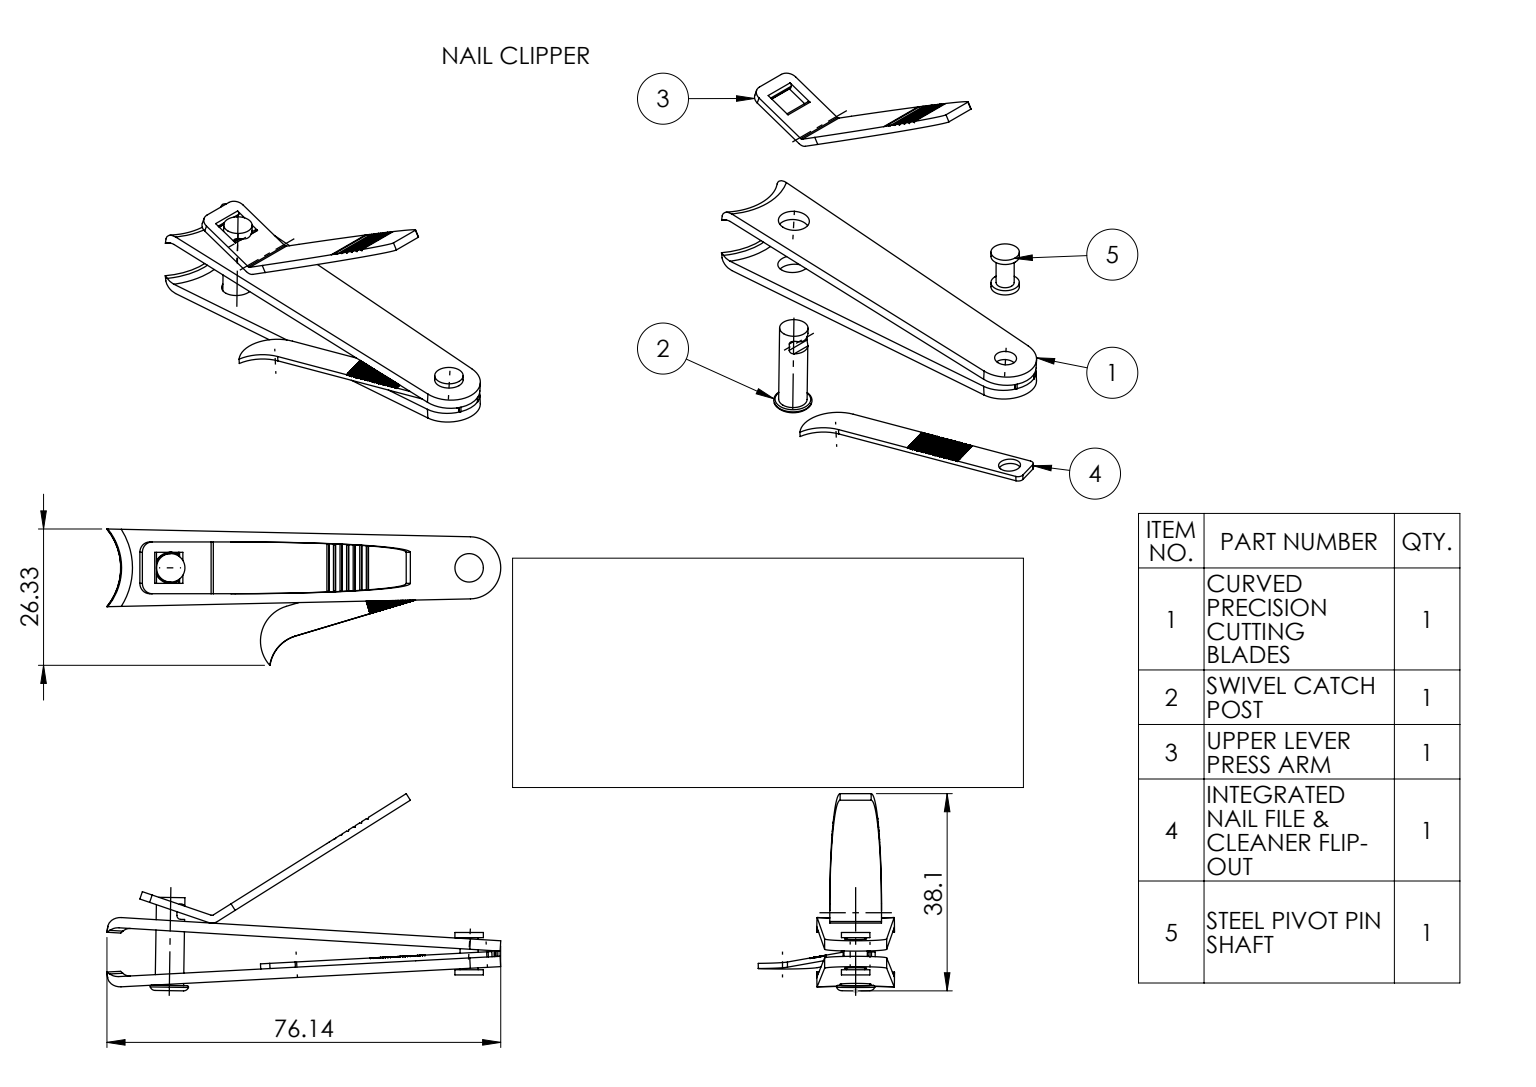
ISO-10303-21;
HEADER;
FILE_DESCRIPTION (('STEP AP214'),
    '1' );
FILE_NAME ('BR-836',
    '2026-09-30T04:43:20',
    ( '' ),
    ( '' ),
    'SwSTEP 2.0',
    'SolidWorks 2026',
    '' );
FILE_SCHEMA (( 'AUTOMOTIVE_DESIGN' ));
ENDSEC;

DATA;
#1 = LINE ( 'NONE', #25573, #52192 ) ;
#2 = VERTEX_POINT ( 'NONE', #10749 ) ;
#3 = B_SPLINE_CURVE_WITH_KNOTS ( 'NONE', 3,
 ( #22146, #34945, #44004, #5128 ),
 .UNSPECIFIED., .F., .F.,
 ( 4, 4 ),
 ( 1.885719144749635755E-05, 0.0003537736795864013565 ),
 .UNSPECIFIED. ) ;
#4 = DIRECTION ( 'NONE',  ( 0.9659258262890682012, -0.2588190451025213501, 0.000000000000000000 ) ) ;
#5 = EDGE_CURVE ( 'NONE', #33225, #52332, #37701, .T. ) ;
#6 = ORIENTED_EDGE ( 'NONE', *, *, #640, .F. ) ;
#7 = FACE_OUTER_BOUND ( 'NONE', #50203, .T. ) ;
#8 = ORIENTED_EDGE ( 'NONE', *, *, #49782, .T. ) ;
#9 = DIRECTION ( 'NONE',  ( 0.7660212471507180654, -0.6427876096865404731, 0.005961354470445141482 ) ) ;
#10 = EDGE_CURVE ( 'NONE', #34917, #49361, #53883, .T. ) ;
#11 = ORIENTED_EDGE ( 'NONE', *, *, #22264, .F. ) ;
#12 = ORIENTED_EDGE ( 'NONE', *, *, #56053, .T. ) ;
#13 = ORIENTED_EDGE ( 'NONE', *, *, #9607, .F. ) ;
#14 = DIRECTION ( 'NONE',  ( -0.6427681459581293666, -0.7660444431189770143, -0.005002170337467561935 ) ) ;
#15 = CARTESIAN_POINT ( 'NONE',  ( -14.94838282604900748, -0.1191753592594197858, 2.588085963191248506 ) ) ;
#16 = FACE_OUTER_BOUND ( 'NONE', #22473, .T. ) ;
#17 = CARTESIAN_POINT ( 'NONE',  ( -15.43471928309396013, -0.1191753592594189115, 4.430961529461709070 ) ) ;
#18 = VERTEX_POINT ( 'NONE', #46192 ) ;
#19 = ORIENTED_EDGE ( 'NONE', *, *, #1841, .F. ) ;
#20 = ORIENTED_EDGE ( 'NONE', *, *, #40291, .F. ) ;
#21 = CARTESIAN_POINT ( 'NONE',  ( -27.06630483948590893, -0.1191753592594197858, 7.295098399573937797 ) ) ;
#22 = EDGE_LOOP ( 'NONE', ( #47630, #41472, #34640 ) ) ;
#23 = PLANE ( 'NONE',  #10320 ) ;
#24 = ORIENTED_EDGE ( 'NONE', *, *, #10341, .T. ) ;
#25 = LINE ( 'NONE', #55156, #19677 ) ;
#26 = FACE_OUTER_BOUND ( 'NONE', #52687, .T. ) ;
#27 = B_SPLINE_CURVE_WITH_KNOTS ( 'NONE', 3,
 ( #5781, #31047, #23391, #22809, #48941, #35902, #48672, #40707, #18006, #52911, #26803, #36426 ),
 .UNSPECIFIED., .F., .F.,
 ( 4, 2, 2, 2, 2, 4 ),
 ( 0.07980989636644560126, 0.1159099261691615840, 0.2318198523383231402, 0.4636397046766463914, 0.6954595570149695316, 0.9272794093314227215 ),
 .UNSPECIFIED. ) ;
#28 = EDGE_LOOP ( 'NONE', ( #23520, #5098, #48877, #45921 ) ) ;
#29 = DIRECTION ( 'NONE',  ( -0.005961354470445682716, -0.6427876096865404731, 0.7660212471507180654 ) ) ;
#30 = EDGE_CURVE ( 'NONE', #53080, #21477, #45939, .T. ) ;
#31 = VERTEX_POINT ( 'NONE', #49893 ) ;
#32 = AXIS2_PLACEMENT_3D ( 'NONE', #18822, #46039, #24446 ) ;
#33 = CARTESIAN_POINT ( 'NONE',  ( -8.975993561185934055, -0.1191753592594197858, 10.41700724906143982 ) ) ;
#34 = EDGE_LOOP ( 'NONE', ( #54000, #22369, #27701, #44259 ) ) ;
#35 = CARTESIAN_POINT ( 'NONE',  ( -12.70458494993575194, -0.1191753592594197858, 11.86531876794841978 ) ) ;
#36 = FACE_OUTER_BOUND ( 'NONE', #31619, .T. ) ;
#37 = CARTESIAN_POINT ( 'NONE',  ( -13.73672976910459909, 0.000000000000000000, 12.22661844811216270 ) ) ;
#38 = ORIENTED_EDGE ( 'NONE', *, *, #21938, .F. ) ;
#39 = CARTESIAN_POINT ( 'NONE',  ( -16.82003048110239973, -0.1191753592594181482, 3.315097473835892039 ) ) ;
#40 = CARTESIAN_POINT ( 'NONE',  ( -17.38829393498713571, 0.000000000000000000, 3.777097248297537124 ) ) ;
#41 = DIRECTION ( 'NONE',  ( 0.007781995580012663651, -3.146120232559066537E-19, -0.9999697198139514409 ) ) ;
#42 = CARTESIAN_POINT ( 'NONE',  ( -4.289188282875421088, -6.206962462949310755, 4.884439966179827231 ) ) ;
#43 = CARTESIAN_POINT ( 'NONE',  ( -6.343177736738851102, -8.196582280829671774, 5.682279223835847937 ) ) ;
#45 = EDGE_CURVE ( 'NONE', #30649, #39352, #46465, .T. ) ;
#44 = LINE ( 'NONE', #33333, #46041 ) ;
#46 = CARTESIAN_POINT ( 'NONE',  ( -17.46532115785441519, 0.000000000000000000, 13.67492996699914265 ) ) ;
#47 = ORIENTED_EDGE ( 'NONE', *, *, #3666, .T. ) ;
#48 = CARTESIAN_POINT ( 'NONE',  ( -10.21144203228149117, 0.000000000000000000, 2.894278973455366444 ) ) ;
#49 = FACE_OUTER_BOUND ( 'NONE', #34512, .T. ) ;
#50 = DIRECTION ( 'NONE',  ( -0.5449076811759708816, 0.6444004775717707689, 0.5364919789714475140 ) ) ;
#51 = ORIENTED_EDGE ( 'NONE', *, *, #37599, .T. ) ;
#52 = CARTESIAN_POINT ( 'NONE',  ( -19.46232870854519703, -3.756034771668159689, 10.40605410012864773 ) ) ;
#53 = CARTESIAN_POINT ( 'NONE',  ( -14.22677752833734566, -0.3560938001956537868, 2.792505858709713795 ) ) ;
#54 = ORIENTED_EDGE ( 'NONE', *, *, #55093, .T. ) ;
#55 = DIRECTION ( 'NONE',  ( -0.005002170337468016433, -0.7660444431189770143, 0.6427681459581293666 ) ) ;
#56 = AXIS2_PLACEMENT_3D ( 'NONE', #16443, #12198, #42577 ) ;
#57 = EDGE_CURVE ( 'NONE', #19141, #38385, #32336, .T. ) ;
#58 = LINE ( 'NONE', #52599, #10348 ) ;
#59 = DIRECTION ( 'NONE',  ( 0.7660212471507180654, -0.6427876096865404731, 0.005961354470445141482 ) ) ;
#60 = ADVANCED_FACE ( 'NONE', ( #15818 ), #6753, .F. ) ;
#61 = CARTESIAN_POINT ( 'NONE',  ( -69.74692240850775704, 2.000000000000830003, -7.382776467523781250 ) ) ;
#62 = ORIENTED_EDGE ( 'NONE', *, *, #8095, .T. ) ;
#63 = ORIENTED_EDGE ( 'NONE', *, *, #47329, .F. ) ;
#64 = PLANE ( 'NONE',  #40295 ) ;
#65 = CARTESIAN_POINT ( 'NONE',  ( 2.072287782118878319, 0.000000000000000000, -2.950529333540147015 ) ) ;
#66 = CARTESIAN_POINT ( 'NONE',  ( -10.20856797877621069, 0.000000000000000000, 2.524969270197602089 ) ) ;
#67 = LINE ( 'NONE', #34732, #24784 ) ;
#68 = EDGE_CURVE ( 'NONE', #2840, #34483, #50479, .T. ) ;
#69 = LINE ( 'NONE', #17405, #45540 ) ;
#70 = VECTOR ( 'NONE', #21292, 999.9999999999998863 ) ;
#71 = FACE_OUTER_BOUND ( 'NONE', #956, .T. ) ;
#72 = ORIENTED_EDGE ( 'NONE', *, *, #35043, .F. ) ;
#73 = DIRECTION ( 'NONE',  ( -0.6427681459581293666, -0.7660444431189770143, -0.005002170337467561935 ) ) ;
#74 = VECTOR ( 'NONE', #36543, 999.9999999999998863 ) ;
#75 = ADVANCED_FACE ( 'NONE', ( #45360 ), #6472, .F. ) ;
#76 = PLANE ( 'NONE',  #14275 ) ;
#77 = EDGE_LOOP ( 'NONE', ( #29388, #6905, #15789, #43672 ) ) ;
#78 = LINE ( 'NONE', #17411, #16572 ) ;
#79 = LINE ( 'NONE', #52063, #49503 ) ;
#80 = DIRECTION ( 'NONE',  ( 0.005002170337468016433, -0.7660444431189770143, -0.6427681459581293666 ) ) ;
#81 = ORIENTED_EDGE ( 'NONE', *, *, #39049, .F. ) ;
#82 = FACE_OUTER_BOUND ( 'NONE', #1972, .T. ) ;
#83 = VERTEX_POINT ( 'NONE', #15002 ) ;
#84 = ORIENTED_EDGE ( 'NONE', *, *, #47098, .T. ) ;
#85 = ORIENTED_EDGE ( 'NONE', *, *, #23256, .T. ) ;
#86 = ORIENTED_EDGE ( 'NONE', *, *, #47911, .T. ) ;
#87 = DIRECTION ( 'NONE',  ( 0.005002170337468016433, -0.7660444431189770143, -0.6427681459581293666 ) ) ;
#89 = EDGE_CURVE ( 'NONE', #51823, #2618, #23778, .T. ) ;
#88 = ORIENTED_EDGE ( 'NONE', *, *, #42803, .T. ) ;
#90 = DIRECTION ( 'NONE',  ( -0.5364919789714478471, 0.6444004775717705469, -0.5449076811759709926 ) ) ;
#91 = AXIS2_PLACEMENT_3D ( 'NONE', #49933, #23822, #53928 ) ;
#92 = VECTOR ( 'NONE', #28630, 1000.000000000000227 ) ;
#93 = VERTEX_POINT ( 'NONE', #7584 ) ;
#94 = CARTESIAN_POINT ( 'NONE',  ( -17.93139508144814442, 0.000000000000000000, 13.85596890686001537 ) ) ;
#95 = ORIENTED_EDGE ( 'NONE', *, *, #27439, .T. ) ;
#96 = CARTESIAN_POINT ( 'NONE',  ( -15.04104892662381054, -1.327505506330656670, 2.681420940547515563 ) ) ;
#97 = EDGE_CURVE ( 'NONE', #51394, #16631, #45637, .T. ) ;
#98 = VERTEX_POINT ( 'NONE', #19810 ) ;
#99 = DIRECTION ( 'NONE',  ( -0.5449076811759708816, 0.6444004775717707689, 0.5364919789714475140 ) ) ;
#100 = DIRECTION ( 'NONE',  ( 0.5449076811759707706, 0.6444004775717708799, -0.5364919789714476250 ) ) ;
#101 = EDGE_CURVE ( 'NONE', #33893, #38385, #37132, .T. ) ;
#102 = DIRECTION ( 'NONE',  ( 0.6427681459581294776, -0.7660444431189769032, 0.005002170337467562802 ) ) ;
#103 = PLANE ( 'NONE',  #32324 ) ;
#104 = DIRECTION ( 'NONE',  ( 0.9999697198139515519, 0.000000000000000000, 0.007781995580013368816 ) ) ;
#105 = ORIENTED_EDGE ( 'NONE', *, *, #27186, .T. ) ;
#106 = EDGE_CURVE ( 'NONE', #30303, #19164, #12974, .T. ) ;
#107 = EDGE_CURVE ( 'NONE', #29873, #51521, #8427, .T. ) ;
#108 = ADVANCED_FACE ( 'NONE', ( #21512 ), #30012, .F. ) ;
#109 = ORIENTED_EDGE ( 'NONE', *, *, #25096, .F. ) ;
#110 = DIRECTION ( 'NONE',  ( 0.005961354470445682716, -0.6427876096865404731, -0.7660212471507180654 ) ) ;
#111 = PLANE ( 'NONE',  #41200 ) ;
#112 = AXIS2_PLACEMENT_3D ( 'NONE', #46198, #6762, #45366 ) ;
#113 = DIRECTION ( 'NONE',  ( 0.007781995580012663651, -3.146120232559066537E-19, -0.9999697198139514409 ) ) ;
#114 = DIRECTION ( 'NONE',  ( -0.7660212471507179544, -0.6427876096865405842, -0.005961354470445141482 ) ) ;
#115 = CARTESIAN_POINT ( 'NONE',  ( -12.13851405436063047, 0.000000000000000000, 11.68505802764555135 ) ) ;
#116 = CARTESIAN_POINT ( 'NONE',  ( -18.13769215924349965, 0.000000000000000000, 6.356589746681873265 ) ) ;
#117 = ORIENTED_EDGE ( 'NONE', *, *, #25709, .T. ) ;
#118 = LINE ( 'NONE', #12391, #16607 ) ;
#119 = CARTESIAN_POINT ( 'NONE',  ( -17.52554100038571860, -1.489407457353157049, 5.933818405385602013 ) ) ;
#120 = ORIENTED_EDGE ( 'NONE', *, *, #23665, .T. ) ;
#121 = DIRECTION ( 'NONE',  ( 0.5449076811759707706, 0.6444004775717708799, -0.5364919789714476250 ) ) ;
#122 = LINE ( 'NONE', #21472, #18778 ) ;
#123 = ADVANCED_FACE ( 'NONE', ( #38236 ), #25209, .F. ) ;
#124 = DIRECTION ( 'NONE',  ( -0.7660212471507179544, -0.6427876096865405842, -0.005961354470445141482 ) ) ;
#125 = FACE_OUTER_BOUND ( 'NONE', #27340, .T. ) ;
#126 = EDGE_CURVE ( 'NONE', #16128, #35650, #30301, .T. ) ;
#127 = LINE ( 'NONE', #17465, #18341 ) ;
#128 = ORIENTED_EDGE ( 'NONE', *, *, #52773, .T. ) ;
#129 = EDGE_LOOP ( 'NONE', ( #42984, #52877, #43620, #27077 ) ) ;
#130 = EDGE_CURVE ( 'NONE', #30420, #39913, #56138, .T. ) ;
#131 = DIRECTION ( 'NONE',  ( 0.007781995580012663651, 0.000000000000000000, -0.9999697198139515519 ) ) ;
#132 = CARTESIAN_POINT ( 'NONE',  ( -22.94165982901027689, 19.41290236794502277, -4.465504107374588472 ) ) ;
#133 = DIRECTION ( 'NONE',  ( -0.5449076811759708816, 0.6444004775717707689, 0.5364919789714475140 ) ) ;
#134 = AXIS2_PLACEMENT_3D ( 'NONE', #24885, #20335, #55533 ) ;
#135 = EDGE_CURVE ( 'NONE', #41809, #20314, #43076, .T. ) ;
#136 = AXIS2_PLACEMENT_3D ( 'NONE', #8040, #24490, #3201 ) ;
#137 = DIRECTION ( 'NONE',  ( 0.9999697198139515519, 0.000000000000000000, 0.007781995580013368816 ) ) ;
#138 = DIRECTION ( 'NONE',  ( 0.007781995580012663651, 0.000000000000000000, -0.9999697198139515519 ) ) ;
#139 = CARTESIAN_POINT ( 'NONE',  ( -18.03530320978490664, 0.7721120973665048792, 3.662821561289850703 ) ) ;
#140 = DIRECTION ( 'NONE',  ( 0.5364919789714477361, 0.6444004775717706579, 0.5449076811759711036 ) ) ;
#141 = EDGE_CURVE ( 'NONE', #45048, #20126, #4465, .T. ) ;
#142 = EDGE_LOOP ( 'NONE', ( #43408, #23853, #54595 ) ) ;
#143 = DIRECTION ( 'NONE',  ( 0.5449076811759707706, 0.6444004775717708799, -0.5364919789714476250 ) ) ;
#144 = CARTESIAN_POINT ( 'NONE',  ( -12.60458797795435615, 0.000000000000000000, 11.86609696750642229 ) ) ;
#145 = AXIS2_PLACEMENT_3D ( 'NONE', #38403, #43503, #3755 ) ;
#146 = ORIENTED_EDGE ( 'NONE', *, *, #35409, .F. ) ;
#147 = LINE ( 'NONE', #43889, #14715 ) ;
#148 = ORIENTED_EDGE ( 'NONE', *, *, #30639, .T. ) ;
#149 = DIRECTION ( 'NONE',  ( 0.007781995580012663651, 0.000000000000000000, -0.9999697198139515519 ) ) ;
#150 = DIRECTION ( 'NONE',  ( 0.005961354470445682716, -0.6427876096865404731, -0.7660212471507180654 ) ) ;
#151 = ORIENTED_EDGE ( 'NONE', *, *, #26951, .F. ) ;
#152 = AXIS2_PLACEMENT_3D ( 'NONE', #22680, #53358, #9066 ) ;
#153 = ORIENTED_EDGE ( 'NONE', *, *, #46826, .T. ) ;
#154 = VECTOR ( 'NONE', #54316, 999.9999999999998863 ) ;
#155 = ORIENTED_EDGE ( 'NONE', *, *, #18719, .T. ) ;
#156 = VERTEX_POINT ( 'NONE', #55864 ) ;
#157 = ORIENTED_EDGE ( 'NONE', *, *, #3395, .T. ) ;
#158 = EDGE_LOOP ( 'NONE', ( #12558, #55338, #5576, #52336 ) ) ;
#159 = LINE ( 'NONE', #30004, #37792 ) ;
#160 = DIRECTION ( 'NONE',  ( -0.5364919789714478471, 0.6444004775717705469, -0.5449076811759709926 ) ) ;
#161 = LINE ( 'NONE', #43615, #10427 ) ;
#162 = ORIENTED_EDGE ( 'NONE', *, *, #35168, .T. ) ;
#163 = DIRECTION ( 'NONE',  ( 0.9999697198139515519, 0.000000000000000000, 0.007781995580013368816 ) ) ;
#164 = ORIENTED_EDGE ( 'NONE', *, *, #30145, .F. ) ;
#165 = VERTEX_POINT ( 'NONE', #25754 ) ;
#166 = CARTESIAN_POINT ( 'NONE',  ( -28.92982233430281980, 0.000000000000000000, 7.919257187036034651 ) ) ;
#167 = DIRECTION ( 'NONE',  ( 0.000000000000000000, -0.000000000000000000, -1.000000000000000000 ) ) ;
#168 = PLANE ( 'NONE',  #1458 ) ;
#169 = ORIENTED_EDGE ( 'NONE', *, *, #7771, .F. ) ;
#170 = LINE ( 'NONE', #34552, #2862 ) ;
#171 = VERTEX_POINT ( 'NONE', #17226 ) ;
#172 = EDGE_CURVE ( 'NONE', #2345, #30417, #47903, .T. ) ;
#173 = EDGE_CURVE ( 'NONE', #12870, #165, #47619, .T. ) ;
#174 = VECTOR ( 'NONE', #52609, 999.9999999999998863 ) ;
#175 = AXIS2_PLACEMENT_3D ( 'NONE', #29245, #50566, #11082 ) ;
#176 = DIRECTION ( 'NONE',  ( -0.6246952433987893460, -0.7422098413412802076, 0.2426528472758542054 ) ) ;
#177 = FACE_OUTER_BOUND ( 'NONE', #19384, .T. ) ;
#178 = ADVANCED_FACE ( 'NONE', ( #38828 ), #34544, .F. ) ;
#179 = PLANE ( 'NONE',  #54119 ) ;
#180 = VECTOR ( 'NONE', #20646, 999.9999999999998863 ) ;
#181 = VECTOR ( 'NONE', #8523, 999.9999999999998863 ) ;
#182 = CARTESIAN_POINT ( 'NONE',  ( -13.92566315350489958, 0.000000000000000000, 2.496041976053526401 ) ) ;
#183 = DIRECTION ( 'NONE',  ( 0.9999697198139515519, 0.000000000000000000, 0.007781995580013368816 ) ) ;
#184 = PLANE ( 'NONE',  #4946 ) ;
#185 = DIRECTION ( 'NONE',  ( 0.9999697198139515519, 0.000000000000000000, 0.007781995580013368816 ) ) ;
#186 = CARTESIAN_POINT ( 'NONE',  ( -66.51694242614880181, -11.33548347488676278, 2.024546322512585039 ) ) ;
#187 = VERTEX_POINT ( 'NONE', #9005 ) ;
#188 = LINE ( 'NONE', #21229, #46462 ) ;
#189 = LINE ( 'NONE', #16995, #9319 ) ;
#190 = FACE_OUTER_BOUND ( 'NONE', #52164, .T. ) ;
#191 = CARTESIAN_POINT ( 'NONE',  ( -10.67549210721878694, 8.288742281967422798, 0.9283501000179719131 ) ) ;
#192 = PRESENTATION_LAYER_ASSIGNMENT (  '', '', ( #25623 ) ) ;
#193 = CARTESIAN_POINT ( 'NONE',  ( -28.44450197225234334, 14.50378416766731959, -4.731833325462559969 ) ) ;
#194 = DIRECTION ( 'NONE',  ( 0.000000000000000000, -0.000000000000000000, -1.000000000000000000 ) ) ;
#195 = ADVANCED_FACE ( 'NONE', ( #42236 ), #20662, .F. ) ;
#196 = DIRECTION ( 'NONE',  ( 0.005961354470445682716, -0.6427876096865404731, -0.7660212471507180654 ) ) ;
#197 = DIRECTION ( 'NONE',  ( 0.5449076811759707706, 0.6444004775717708799, -0.5364919789714476250 ) ) ;
#198 = CONTEXT_DEPENDENT_SHAPE_REPRESENTATION ( #49272, #18769 ) ;
#199 = ORIENTED_EDGE ( 'NONE', *, *, #4188, .F. ) ;
#200 = ADVANCED_FACE ( 'NONE', ( #33997 ), #16371, .F. ) ;
#201 = FACE_OUTER_BOUND ( 'NONE', #9129, .T. ) ;
#202 = FACE_OUTER_BOUND ( 'NONE', #53678, .T. ) ;
#203 = DIRECTION ( 'NONE',  ( 0.6427681459581294776, -0.7660444431189769032, 0.005002170337467562802 ) ) ;
#204 = EDGE_CURVE ( 'NONE', #54577, #15326, #19532, .T. ) ;
#205 = DIRECTION ( 'NONE',  ( 0.9999697198139515519, 0.000000000000000000, 0.007781995580013368816 ) ) ;
#206 = CARTESIAN_POINT ( 'NONE',  ( -13.48976679171663484, 0.000000000000000000, 6.192754920399180740 ) ) ;
#207 = VECTOR ( 'NONE', #19976, 1000.000000000000227 ) ;
#208 = EDGE_CURVE ( 'NONE', #16268, #38932, #12121, .T. ) ;
#209 = CARTESIAN_POINT ( 'NONE',  ( -15.52531589500150666, 0.000000000000000000, 3.222257248149021258 ) ) ;
#210 = LINE ( 'NONE', #17557, #51006 ) ;
#211 = CARTESIAN_POINT ( 'NONE',  ( -19.32961685222932147, 0.000000000000000000, 14.39908572644263351 ) ) ;
#212 = CARTESIAN_POINT ( 'NONE',  ( -17.36187534420177769, 4.333955019861509328, 10.73802165171122347 ) ) ;
#213 = EDGE_CURVE ( 'NONE', #291, #19762, #47053, .T. ) ;
#214 = AXIS2_PLACEMENT_3D ( 'NONE', #5223, #35051, #73 ) ;
#215 = EDGE_LOOP ( 'NONE', ( #36869, #50678, #13094, #16447 ) ) ;
#216 = DIRECTION ( 'NONE',  ( 0.5364919789714477361, 0.6444004775717706579, 0.5449076811759711036 ) ) ;
#217 = EDGE_CURVE ( 'NONE', #7467, #3951, #3878, .T. ) ;
#218 = VECTOR ( 'NONE', #12479, 1000.000000000000227 ) ;
#219 = AXIS2_PLACEMENT_3D ( 'NONE', #34025, #46802, #8180 ) ;
#220 = EDGE_LOOP ( 'NONE', ( #56199, #45802, #49366, #38955 ) ) ;
#221 = ADVANCED_FACE ( 'NONE', ( #13537 ), #1011, .F. ) ;
#222 = VECTOR ( 'NONE', #40260, 1000.000000000000227 ) ;
#223 = VERTEX_POINT ( 'NONE', #1301 ) ;
#224 = EDGE_LOOP ( 'NONE', ( #49282, #54509, #50774, #34578 ) ) ;
#225 = AXIS2_PLACEMENT_3D ( 'NONE', #48781, #44235, #9876 ) ;
#226 = ORIENTED_EDGE ( 'NONE', *, *, #56206, .F. ) ;
#227 = ORIENTED_EDGE ( 'NONE', *, *, #29291, .F. ) ;
#228 = CARTESIAN_POINT ( 'NONE',  ( -14.01701317841955508, 0.000000000000000000, 2.326005055450897085 ) ) ;
#229 = DIRECTION ( 'NONE',  ( -0.005961354470445682716, -0.6427876096865404731, 0.7660212471507180654 ) ) ;
#230 = ORIENTED_EDGE ( 'NONE', *, *, #6847, .F. ) ;
#231 = ORIENTED_EDGE ( 'NONE', *, *, #14544, .F. ) ;
#232 = VECTOR ( 'NONE', #3897, 1000.000000000000227 ) ;
#233 = AXIS2_PLACEMENT_3D ( 'NONE', #39851, #932, #52902 ) ;
#234 = LINE ( 'NONE', #25830, #10239 ) ;
#235 = VERTEX_POINT ( 'NONE', #4730 ) ;
#236 = CARTESIAN_POINT ( 'NONE',  ( -18.67619601524082285, 0.000000000000000000, 3.936400510096834893 ) ) ;
#237 = LINE ( 'NONE', #8811, #24972 ) ;
#238 = ORIENTED_EDGE ( 'NONE', *, *, #26646, .F. ) ;
#239 = FACE_OUTER_BOUND ( 'NONE', #22439, .T. ) ;
#240 = AXIS2_PLACEMENT_3D ( 'NONE', #41868, #37631, #6419 ) ;
#242 = ORIENTED_EDGE ( 'NONE', *, *, #47787, .F. ) ;
#241 = EDGE_CURVE ( 'NONE', #29572, #36873, #1603, .T. ) ;
#243 = DIRECTION ( 'NONE',  ( 0.000000000000000000, -1.000000000000000000, 0.000000000000000000 ) ) ;
#244 = VECTOR ( 'NONE', #39775, 1000.000000000000114 ) ;
#245 = EDGE_CURVE ( 'NONE', #18842, #26839, #48755, .T. ) ;
#246 = EDGE_CURVE ( 'NONE', #931, #21351, #36247, .T. ) ;
#247 = CARTESIAN_POINT ( 'NONE',  ( -13.46034487804917390, 5.305366725996514710, 1.741117822157838724 ) ) ;
#248 = EDGE_LOOP ( 'NONE', ( #22673, #25406, #16303, #10944 ) ) ;
#249 = PLANE ( 'NONE',  #50315 ) ;
#250 = CARTESIAN_POINT ( 'NONE',  ( -14.17032429916292813, 0.000000000000000000, 8.234125069766777827 ) ) ;
#251 = CARTESIAN_POINT ( 'NONE',  ( -11.20636620717317378, 0.000000000000000000, 11.32298014792380414 ) ) ;
#252 = VECTOR ( 'NONE', #13641, 999.9999999999998863 ) ;
#253 = ORIENTED_EDGE ( 'NONE', *, *, #19870, .F. ) ;
#254 = CARTESIAN_POINT ( 'NONE',  ( -23.33849165029409889, 0.000000000000000000, 5.946783852668351855 ) ) ;
#255 = ORIENTED_EDGE ( 'NONE', *, *, #35065, .T. ) ;
#256 = VECTOR ( 'NONE', #15844, 1000.000000000000227 ) ;
#257 = AXIS2_PLACEMENT_3D ( 'NONE', #26686, #13372, #44005 ) ;
#258 = DIRECTION ( 'NONE',  ( -0.6427681459581293666, -0.7660444431189770143, -0.005002170337467561935 ) ) ;
#259 = LINE ( 'NONE', #22700, #51384 ) ;
#260 = DIRECTION ( 'NONE',  ( -0.9999697198139514409, -0.000000000000000000, -0.007781995580013368816 ) ) ;
#261 = DIRECTION ( 'NONE',  ( -0.6427681459581293666, -0.7660444431189770143, -0.005002170337467561935 ) ) ;
#262 = PLANE ( 'NONE',  #7783 ) ;
#263 = CARTESIAN_POINT ( 'NONE',  ( -18.19747506107908563, 0.000000000000000000, 14.03856424583689311 ) ) ;
#264 = DIRECTION ( 'NONE',  ( -0.7660212471507179544, -0.6427876096865405842, -0.005961354470445141482 ) ) ;
#265 = AXIS2_PLACEMENT_3D ( 'NONE', #36413, #10611, #26789 ) ;
#266 = DIRECTION ( 'NONE',  ( 0.000000000000000000, -0.000000000000000000, -1.000000000000000000 ) ) ;
#267 = VECTOR ( 'NONE', #8315, 999.9999999999998863 ) ;
#268 = CARTESIAN_POINT ( 'NONE',  ( -23.33771345073609638, -0.1191753592594197858, 5.846786880686956955 ) ) ;
#269 = ORIENTED_EDGE ( 'NONE', *, *, #16189, .T. ) ;
#270 = DIRECTION ( 'NONE',  ( -0.005002170337468016433, -0.7660444431189770143, 0.6427681459581293666 ) ) ;
#271 = LINE ( 'NONE', #1112, #10920 ) ;
#272 = CARTESIAN_POINT ( 'NONE',  ( 2.072287782118878319, 0.000000000000000000, -2.950529333540147015 ) ) ;
#273 = CARTESIAN_POINT ( 'NONE',  ( -11.87243407472968926, 0.000000000000000000, 11.50246268866867361 ) ) ;
#274 = AXIS2_PLACEMENT_3D ( 'NONE', #26963, #39157, #26121 ) ;
#275 = AXIS2_PLACEMENT_3D ( 'NONE', #49131, #52299, #27016 ) ;
#276 = EDGE_CURVE ( 'NONE', #2654, #52427, #22050, .T. ) ;
#277 = FACE_OUTER_BOUND ( 'NONE', #5267, .T. ) ;
#278 = CARTESIAN_POINT ( 'NONE',  ( -16.79925329029790149, 0.000000000000000000, 13.49544742625427496 ) ) ;
#279 = ORIENTED_EDGE ( 'NONE', *, *, #9058, .T. ) ;
#280 = VERTEX_POINT ( 'NONE', #756 ) ;
#281 = EDGE_CURVE ( 'NONE', #14069, #52686, #39928, .T. ) ;
#282 = DIRECTION ( 'NONE',  ( 0.005002170337468016433, -0.7660444431189770143, -0.6427681459581293666 ) ) ;
#283 = CARTESIAN_POINT ( 'NONE',  ( -17.73140113748535285, 0.000000000000000000, 13.85752530597602039 ) ) ;
#284 = ORIENTED_EDGE ( 'NONE', *, *, #29998, .F. ) ;
#285 = VECTOR ( 'NONE', #53236, 1000.000000000000227 ) ;
#286 = FACE_OUTER_BOUND ( 'NONE', #8165, .T. ) ;
#287 = EDGE_LOOP ( 'NONE', ( #31043, #13115, #52818, #45322 ) ) ;
#288 = CARTESIAN_POINT ( 'NONE',  ( -19.79569077582305070, 0.000000000000000000, 14.58012466630350445 ) ) ;
#289 = EDGE_CURVE ( 'NONE', #36837, #44524, #470, .T. ) ;
#290 = VECTOR ( 'NONE', #6881, 999.9999999999998863 ) ;
#291 = VERTEX_POINT ( 'NONE', #9262 ) ;
#292 = CARTESIAN_POINT ( 'NONE',  ( -18.44716714978218164, 2.876837460659007473, 8.768207690109344199 ) ) ;
#293 = ORIENTED_EDGE ( 'NONE', *, *, #18760, .T. ) ;
#294 = VERTEX_POINT ( 'NONE', #53546 ) ;
#295 = ORIENTED_EDGE ( 'NONE', *, *, #8160, .T. ) ;
#296 = CARTESIAN_POINT ( 'NONE',  ( -15.86710544311044302, 0.000000000000000000, 13.13336954653252953 ) ) ;
#297 = VECTOR ( 'NONE', #13524, 1000.000000000000000 ) ;
#298 = FACE_OUTER_BOUND ( 'NONE', #53215, .T. ) ;
#299 = DIRECTION ( 'NONE',  ( -0.1139275668495183524, 0.9934890585767659488, 4.694855797473114533E-16 ) ) ;
#300 = EDGE_CURVE ( 'NONE', #33548, #11209, #18927, .T. ) ;
#301 = AXIS2_PLACEMENT_3D ( 'NONE', #8298, #21377, #55722 ) ;
#302 = VECTOR ( 'NONE', #4764, 999.9999999999998863 ) ;
#303 = DIRECTION ( 'NONE',  ( 0.007781995580012663651, 0.000000000000000000, -0.9999697198139515519 ) ) ;
#304 = EDGE_LOOP ( 'NONE', ( #25150, #34611, #28054, #8360, #39695 ) ) ;
#305 = ORIENTED_EDGE ( 'NONE', *, *, #38261, .F. ) ;
#306 = EDGE_CURVE ( 'NONE', #53467, #42919, #52440, .T. ) ;
#307 = VECTOR ( 'NONE', #12261, 1000.000000000000114 ) ;
#308 = VERTEX_POINT ( 'NONE', #35146 ) ;
#309 = VECTOR ( 'NONE', #14747, 999.9999999999998863 ) ;
#310 = B_SPLINE_CURVE_WITH_KNOTS ( 'NONE', 3,
 ( #32716, #11134, #41787, #2878 ),
 .UNSPECIFIED., .F., .F.,
 ( 4, 4 ),
 ( 0.000000000000000000, 0.0003538863460372422966 ),
 .UNSPECIFIED. ) ;
#311 = DIRECTION ( 'NONE',  ( 0.9999697198139515519, 0.000000000000000000, 0.007781995580013368816 ) ) ;
#312 = ORIENTED_EDGE ( 'NONE', *, *, #31310, .T. ) ;
#313 = DIRECTION ( 'NONE',  ( 0.000000000000000000, -0.000000000000000000, -1.000000000000000000 ) ) ;
#314 = EDGE_CURVE ( 'NONE', #9163, #26799, #27158, .T. ) ;
#315 = ORIENTED_EDGE ( 'NONE', *, *, #40972, .T. ) ;
#316 = PLANE ( 'NONE',  #44171 ) ;
#317 = LINE ( 'NONE', #31273, #54806 ) ;
#318 = ORIENTED_EDGE ( 'NONE', *, *, #12951, .T. ) ;
#319 = EDGE_CURVE ( 'NONE', #50963, #26160, #44464, .T. ) ;
#320 = CARTESIAN_POINT ( 'NONE',  ( -27.99767448711536133, 0.000000000000000000, 7.557179307314289218 ) ) ;
#321 = ORIENTED_EDGE ( 'NONE', *, *, #1045, .T. ) ;
#322 = EDGE_CURVE ( 'NONE', #38023, #19674, #26588, .T. ) ;
#323 = LINE ( 'NONE', #12572, #26385 ) ;
#324 = VECTOR ( 'NONE', #8090, 1000.000000000000227 ) ;
#325 = ORIENTED_EDGE ( 'NONE', *, *, #12524, .F. ) ;
#326 = CARTESIAN_POINT ( 'NONE',  ( -20.54049170961573267, 0.000000000000000000, 4.660556269540326646 ) ) ;
#327 = CARTESIAN_POINT ( 'NONE',  ( -17.33634854152196780, -0.1191753592594171213, 9.952400094065581015 ) ) ;
#328 = DIRECTION ( 'NONE',  ( 0.6427681459581294776, -0.7660444431189769032, 0.005002170337467562802 ) ) ;
#329 = VERTEX_POINT ( 'NONE', #5025 ) ;
#330 = VECTOR ( 'NONE', #29769, 999.9999999999998863 ) ;
#331 = EDGE_CURVE ( 'NONE', #20000, #39753, #13803, .T. ) ;
#332 = LINE ( 'NONE', #21661, #54656 ) ;
#333 = CARTESIAN_POINT ( 'NONE',  ( -17.75117697256323268, -2.298917212465658277, 7.350006499361532164 ) ) ;
#334 = CARTESIAN_POINT ( 'NONE',  ( -17.36532418587302473, -0.1191753592594177458, 13.67570816655714516 ) ) ;
#335 = VECTOR ( 'NONE', #1032, 999.9999999999998863 ) ;
#336 = LINE ( 'NONE', #47792, #17706 ) ;
#337 = LINE ( 'NONE', #39552, #37612 ) ;
#338 = DIRECTION ( 'NONE',  ( 0.9999697198139515519, 0.000000000000000000, 0.007781995580013368816 ) ) ;
#339 = EDGE_CURVE ( 'NONE', #23586, #15428, #53300, .T. ) ;
#340 = DIRECTION ( 'NONE',  ( -0.7660212471507179544, -0.6427876096865405842, -0.005961354470445141482 ) ) ;
#341 = ORIENTED_EDGE ( 'NONE', *, *, #38336, .T. ) ;
#342 = CARTESIAN_POINT ( 'NONE',  ( 2.072287782118878319, 0.000000000000000000, -2.950529333540147015 ) ) ;
#343 = LINE ( 'NONE', #21391, #3196 ) ;
#344 = DIRECTION ( 'NONE',  ( 0.007781995580012662783, 0.000000000000000000, -0.9999697198139514409 ) ) ;
#345 = VERTEX_POINT ( 'NONE', #31128 ) ;
#346 = VECTOR ( 'NONE', #15392, 999.9999999999998863 ) ;
#347 = DIRECTION ( 'NONE',  ( 0.7660212471507180654, -0.6427876096865404731, 0.005961354470445141482 ) ) ;
#348 = FACE_OUTER_BOUND ( 'NONE', #54993, .T. ) ;
#349 = VERTEX_POINT ( 'NONE', #31706 ) ;
#350 = VECTOR ( 'NONE', #2759, 999.9999999999998863 ) ;
#351 = CARTESIAN_POINT ( 'NONE',  ( -6.110905869600904872, 1.712176620043476140E-14, 3.600000000000000089 ) ) ;
#352 = DIRECTION ( 'NONE',  ( 0.5449076811759707706, 0.6444004775717708799, -0.5364919789714476250 ) ) ;
#353 = DIRECTION ( 'NONE',  ( 0.7660212471507180654, -0.6427876096865404731, 0.005961354470445141482 ) ) ;
#354 = CARTESIAN_POINT ( 'NONE',  ( -69.95337746243399124, 0.1332479302464926740, -7.442420802399271729 ) ) ;
#355 = ORIENTED_EDGE ( 'NONE', *, *, #29279, .T. ) ;
#356 = VECTOR ( 'NONE', #10520, 1000.000000000000114 ) ;
#357 = VECTOR ( 'NONE', #13768, 1000.000000000000000 ) ;
#358 = ORIENTED_EDGE ( 'NONE', *, *, #4456, .T. ) ;
#359 = CARTESIAN_POINT ( 'NONE',  ( -19.33878870862964305, -1.975113310420658852, 7.435271445270302593 ) ) ;
#360 = DIRECTION ( 'NONE',  ( 0.007781995580012662783, 0.000000000000000000, -0.9999697198139514409 ) ) ;
#361 = DIRECTION ( 'NONE',  ( -0.9999697198139514409, -0.000000000000000000, -0.007781995580013368816 ) ) ;
#362 = PLANE ( 'NONE',  #37468 ) ;
#363 = DIRECTION ( 'NONE',  ( 0.5449076811759707706, 0.6444004775717708799, -0.5364919789714476250 ) ) ;
#364 = FACE_OUTER_BOUND ( 'NONE', #14108, .T. ) ;
#365 = EDGE_CURVE ( 'NONE', #15522, #6083, #49011, .T. ) ;
#366 = EDGE_LOOP ( 'NONE', ( #1218, #51641 ) ) ;
#367 = LINE ( 'NONE', #4924, #1109 ) ;
#368 = VECTOR ( 'NONE', #37920, 1000.000000000000227 ) ;
#369 = FACE_OUTER_BOUND ( 'NONE', #44588, .T. ) ;
#370 = VERTEX_POINT ( 'NONE', #48452 ) ;
#371 = AXIS2_PLACEMENT_3D ( 'NONE', #6600, #33303, #28757 ) ;
#372 = DIRECTION ( 'NONE',  ( 0.005961354470445682716, -0.6427876096865404731, -0.7660212471507180654 ) ) ;
#373 = CARTESIAN_POINT ( 'NONE',  ( -27.13182931993292257, 16.99370688441070953, -4.657437592157545936 ) ) ;
#374 = AXIS2_PLACEMENT_3D ( 'NONE', #30248, #4416, #8373 ) ;
#375 = LINE ( 'NONE', #930, #8550 ) ;
#376 = EDGE_CURVE ( 'NONE', #36173, #27809, #10111, .T. ) ;
#377 = ORIENTED_EDGE ( 'NONE', *, *, #20121, .F. ) ;
#378 = PLANE ( 'NONE',  #3086 ) ;
#379 = VECTOR ( 'NONE', #26653, 1000.000000000000114 ) ;
#380 = ORIENTED_EDGE ( 'NONE', *, *, #23171, .F. ) ;
#381 = EDGE_CURVE ( 'NONE', #34243, #38141, #26893, .T. ) ;
#382 = ADVANCED_FACE ( 'NONE', ( #5312 ), #20295, .F. ) ;
#383 = ORIENTED_EDGE ( 'NONE', *, *, #43761, .F. ) ;
#384 = EDGE_LOOP ( 'NONE', ( #49839, #18862, #38770, #29467 ) ) ;
#385 = ORIENTED_EDGE ( 'NONE', *, *, #20357, .F. ) ;
#386 = VECTOR ( 'NONE', #38602, 999.9999999999998863 ) ;
#387 = PLANE ( 'NONE',  #36628 ) ;
#388 = ORIENTED_EDGE ( 'NONE', *, *, #50925, .F. ) ;
#389 = CARTESIAN_POINT ( 'NONE',  ( -18.35912213213254773, 0.000000000000000000, 9.109517029665196830 ) ) ;
#390 = VECTOR ( 'NONE', #55175, 999.9999999999998863 ) ;
#391 = ORIENTED_EDGE ( 'NONE', *, *, #38213, .F. ) ;
#392 = LINE ( 'NONE', #30530, #43118 ) ;
#393 = EDGE_CURVE ( 'NONE', #50596, #19103, #2684, .T. ) ;
#394 = VERTEX_POINT ( 'NONE', #27729 ) ;
#395 = DIRECTION ( 'NONE',  ( 0.8531650599175527594, 0.4028455766673922356, -0.3313982828793700652 ) ) ;
#396 = ORIENTED_EDGE ( 'NONE', *, *, #51721, .F. ) ;
#397 = EDGE_CURVE ( 'NONE', #27291, #53062, #24006, .T. ) ;
#398 = VECTOR ( 'NONE', #12673, 999.9999999999998863 ) ;
#399 = VECTOR ( 'NONE', #24658, 1000.000000000000227 ) ;
#400 = LINE ( 'NONE', #29953, #50150 ) ;
#401 = LINE ( 'NONE', #38179, #16866 ) ;
#402 = DIRECTION ( 'NONE',  ( -0.5449076811759708816, 0.6444004775717707689, 0.5364919789714475140 ) ) ;
#403 = CARTESIAN_POINT ( 'NONE',  ( -26.13337879274045505, 0.000000000000000000, 6.833023547870798353 ) ) ;
#404 = DIRECTION ( 'NONE',  ( 0.5449076811759707706, 0.6444004775717708799, -0.5364919789714476250 ) ) ;
#405 = ORIENTED_EDGE ( 'NONE', *, *, #31844, .T. ) ;
#406 = EDGE_CURVE ( 'NONE', #17338, #35631, #37331, .T. ) ;
#407 = ORIENTED_EDGE ( 'NONE', *, *, #12412, .F. ) ;
#408 = PLANE ( 'NONE',  #43098 ) ;
#409 = LINE ( 'NONE', #47855, #23972 ) ;
#410 = FACE_OUTER_BOUND ( 'NONE', #52245, .T. ) ;
#411 = VECTOR ( 'NONE', #55065, 1000.000000000000227 ) ;
#412 = ADVANCED_FACE ( 'NONE', ( #32269 ), #15751, .F. ) ;
#413 = CARTESIAN_POINT ( 'NONE',  ( -11.79828090536769203, 0.000000000000000000, 1.973939673224830660 ) ) ;
#414 = AXIS2_PLACEMENT_3D ( 'NONE', #46926, #25913, #21902 ) ;
#415 = DIRECTION ( 'NONE',  ( 0.007781995580012662783, 0.000000000000000000, -0.9999697198139514409 ) ) ;
#416 = DIRECTION ( 'NONE',  ( 0.005002170337468016433, -0.7660444431189770143, -0.6427681459581293666 ) ) ;
#417 = ORIENTED_EDGE ( 'NONE', *, *, #24919, .T. ) ;
#418 = DIRECTION ( 'NONE',  ( -0.2588190451025176864, -0.9659258262890692004, 0.000000000000000000 ) ) ;
#419 = DIRECTION ( 'NONE',  ( 0.007781995580012663651, -3.146120232559066537E-19, -0.9999697198139514409 ) ) ;
#420 = AXIS2_PLACEMENT_3D ( 'NONE', #54266, #23873, #24706 ) ;
#421 = ORIENTED_EDGE ( 'NONE', *, *, #9837, .T. ) ;
#422 = DIRECTION ( 'NONE',  ( -0.7660212471507179544, -0.6427876096865405842, -0.005961354470445141482 ) ) ;
#423 = CARTESIAN_POINT ( 'NONE',  ( -27.99845268667336384, -0.1191753592594197858, 7.657176279295684118 ) ) ;
#424 = VECTOR ( 'NONE', #53367, 1000.000000000000227 ) ;
#425 = LINE ( 'NONE', #973, #5079 ) ;
#426 = FACE_OUTER_BOUND ( 'NONE', #14338, .T. ) ;
#427 = CARTESIAN_POINT ( 'NONE',  ( -14.15727168602579766, 0.000000000000000000, 6.556892312772929721 ) ) ;
#428 = VERTEX_POINT ( 'NONE', #28541 ) ;
#429 = VECTOR ( 'NONE', #53252, 999.9999999999998863 ) ;
#430 = ORIENTED_EDGE ( 'NONE', *, *, #18527, .F. ) ;
#431 = AXIS2_PLACEMENT_3D ( 'NONE', #56006, #3733, #42926 ) ;
#432 = CARTESIAN_POINT ( 'NONE',  ( -11.26448342554532012, -0.1191753592594185784, 5.940743548404852525 ) ) ;
#433 = CARTESIAN_POINT ( 'NONE',  ( 0.4518049228021103203, -3.655895688227122076, 5.998622290806040702 ) ) ;
#434 = LINE ( 'NONE', #30827, #44226 ) ;
#435 = AXIS2_PLACEMENT_3D ( 'NONE', #40606, #36325, #43706 ) ;
#436 = CARTESIAN_POINT ( 'NONE',  ( -13.73672976910459909, 0.000000000000000000, 12.22661844811216270 ) ) ;
#437 = DIRECTION ( 'NONE',  ( 0.6427681459581294776, -0.7660444431189769032, 0.005002170337467562802 ) ) ;
#438 = EDGE_CURVE ( 'NONE', #41253, #2345, #2131, .T. ) ;
#439 = DIRECTION ( 'NONE',  ( -0.5449076811759708816, 0.6444004775717707689, 0.5364919789714475140 ) ) ;
#440 = CARTESIAN_POINT ( 'NONE',  ( -27.06552663992790997, 0.000000000000000000, 7.195101427592543786 ) ) ;
#441 = VERTEX_POINT ( 'NONE', #46137 ) ;
#442 = VECTOR ( 'NONE', #33608, 999.9999999999998863 ) ;
#443 = FACE_OUTER_BOUND ( 'NONE', #30904, .T. ) ;
#444 = VECTOR ( 'NONE', #34245, 1000.000000000000000 ) ;
#445 = LINE ( 'NONE', #48427, #46891 ) ;
#446 = ADVANCED_FACE ( 'NONE', ( #32795 ), #44037, .T. ) ;
#447 = EDGE_CURVE ( 'NONE', #485, #27823, #40779, .T. ) ;
#448 = ORIENTED_EDGE ( 'NONE', *, *, #34618, .F. ) ;
#449 = CARTESIAN_POINT ( 'NONE',  ( -16.04172443374966761, 4.495856970884011261, 2.769640905047572321 ) ) ;
#450 = EDGE_LOOP ( 'NONE', ( #19965, #9347, #24938, #27730 ) ) ;
#451 = DIRECTION ( 'NONE',  ( 0.9321478471874541372, 0.000000000000000000, -0.3620778797217453771 ) ) ;
#452 = ADVANCED_FACE ( 'NONE', ( #1852 ), #50104, .F. ) ;
#453 = ADVANCED_FACE ( 'NONE', ( #7244 ), #2428, .F. ) ;
#454 = LINE ( 'NONE', #35131, #43843 ) ;
#455 = EDGE_CURVE ( 'NONE', #37705, #6581, #56077, .T. ) ;
#456 = ORIENTED_EDGE ( 'NONE', *, *, #13239, .F. ) ;
#457 = ORIENTED_EDGE ( 'NONE', *, *, #32580, .T. ) ;
#458 = EDGE_CURVE ( 'NONE', #51710, #23249, #53825, .T. ) ;
#459 = VECTOR ( 'NONE', #16090, 1000.000000000000114 ) ;
#460 = VERTEX_POINT ( 'NONE', #2963 ) ;
#461 = ORIENTED_EDGE ( 'NONE', *, *, #35316, .F. ) ;
#462 = ORIENTED_EDGE ( 'NONE', *, *, #15003, .T. ) ;
#463 = AXIS2_PLACEMENT_3D ( 'NONE', #24547, #54121, #23720 ) ;
#464 = ORIENTED_EDGE ( 'NONE', *, *, #30689, .T. ) ;
#465 = DIRECTION ( 'NONE',  ( -0.005002170337468016433, -0.7660444431189770143, 0.6427681459581293666 ) ) ;
#466 = CARTESIAN_POINT ( 'NONE',  ( 2.072287782118878319, 0.000000000000000000, -2.950529333540147015 ) ) ;
#467 = DIRECTION ( 'NONE',  ( 0.007781995580012663651, -3.146120232559066537E-19, -0.9999697198139514409 ) ) ;
#468 = AXIS2_PLACEMENT_3D ( 'NONE', #39473, #17904, #31219 ) ;
#469 = EDGE_LOOP ( 'NONE', ( #53568, #47753, #23192, #24265 ) ) ;
#470 = LINE ( 'NONE', #52994, #35822 ) ;
#471 = EDGE_CURVE ( 'NONE', #12574, #40953, #33382, .T. ) ;
#472 = ORIENTED_EDGE ( 'NONE', *, *, #19438, .F. ) ;
#473 = AXIS2_PLACEMENT_3D ( 'NONE', #21788, #43922, #34860 ) ;
#474 = EDGE_LOOP ( 'NONE', ( #13344, #7979, #54982, #50764 ) ) ;
#475 = EDGE_CURVE ( 'NONE', #5277, #30292, #6413, .T. ) ;
#476 = AXIS2_PLACEMENT_3D ( 'NONE', #44666, #26511, #49210 ) ;
#477 = AXIS2_PLACEMENT_3D ( 'NONE', #5497, #53744, #35905 ) ;
#478 = CARTESIAN_POINT ( 'NONE',  ( -16.79925329029790149, 0.000000000000000000, 13.49544742625427496 ) ) ;
#479 = DIRECTION ( 'NONE',  ( -0.6427681459581293666, -0.7660444431189770143, -0.005002170337467561935 ) ) ;
#480 = EDGE_CURVE ( 'NONE', #29959, #40913, #28257, .T. ) ;
#481 = AXIS2_PLACEMENT_3D ( 'NONE', #37816, #3148, #21324 ) ;
#482 = CARTESIAN_POINT ( 'NONE',  ( -17.46532115785441519, 0.000000000000000000, 13.67492996699914265 ) ) ;
#483 = ORIENTED_EDGE ( 'NONE', *, *, #47027, .F. ) ;
#484 = DIRECTION ( 'NONE',  ( 0.000000000000000000, 0.000000000000000000, 1.000000000000000000 ) ) ;
#485 = VERTEX_POINT ( 'NONE', #6690 ) ;
#486 = VECTOR ( 'NONE', #22922, 1000.000000000000000 ) ;
#487 = ADVANCED_FACE ( 'NONE', ( #41340 ), #54375, .F. ) ;
#488 = VECTOR ( 'NONE', #16446, 1000.000000000000227 ) ;
#489 = CARTESIAN_POINT ( 'NONE',  ( -9.274408763410345813, 2.384096728371167817, 3.117008339208958034 ) ) ;
#490 = FACE_OUTER_BOUND ( 'NONE', #41737, .T. ) ;
#491 = AXIS2_PLACEMENT_3D ( 'NONE', #51141, #37826, #24737 ) ;
#492 = DIRECTION ( 'NONE',  ( -0.9997703818010067467, 0.000000000000000000, -0.02142857142857158143 ) ) ;
#493 = AXIS2_PLACEMENT_3D ( 'NONE', #21084, #8312, #42665 ) ;
#494 = DIRECTION ( 'NONE',  ( 0.007781995580012663651, -3.146120232559066537E-19, -0.9999697198139514409 ) ) ;
#495 = CARTESIAN_POINT ( 'NONE',  ( 4.866417447938704122, 0.000000000000000000, 1.967953638241001002 ) ) ;
#496 = CARTESIAN_POINT ( 'NONE',  ( 6.057149706651311583, -1.000000014492634426, -0.7725429650402538817 ) ) ;
#497 = LINE ( 'NONE', #34563, #49322 ) ;
#498 = CARTESIAN_POINT ( 'NONE',  ( -16.43317633868556626, -0.1191753592594197858, 13.31363028683540151 ) ) ;
#499 = ORIENTED_EDGE ( 'NONE', *, *, #29532, .F. ) ;
#500 = CARTESIAN_POINT ( 'NONE',  ( -16.81190032086591302, 0.000000000000000000, 3.212244750653343583 ) ) ;
#501 = LINE ( 'NONE', #50440, #2942 ) ;
#502 = CARTESIAN_POINT ( 'NONE',  ( -8.129252104341238905, 0.000000000000000000, 6.065145671608219935 ) ) ;
#503 = DIRECTION ( 'NONE',  ( -0.7660212471507179544, -0.6427876096865405842, -0.005961354470445141482 ) ) ;
#504 = DIRECTION ( 'NONE',  ( 0.000000000000000000, -0.000000000000000000, -1.000000000000000000 ) ) ;
#505 = LINE ( 'NONE', #40549, #49453 ) ;
#506 = LINE ( 'NONE', #14144, #19589 ) ;
#507 = AXIS2_PLACEMENT_3D ( 'NONE', #4307, #52278, #48266 ) ;
#508 = LINE ( 'NONE', #12467, #14837 ) ;
#509 = VECTOR ( 'NONE', #35497, 999.9999999999998863 ) ;
#510 = ORIENTED_EDGE ( 'NONE', *, *, #7779, .T. ) ;
#511 = DIRECTION ( 'NONE',  ( 0.005002170337468016433, -0.7660444431189770143, -0.6427681459581293666 ) ) ;
#512 = DIRECTION ( 'NONE',  ( -0.7660212471507179544, -0.6427876096865405842, -0.005961354470445141482 ) ) ;
#513 = CARTESIAN_POINT ( 'NONE',  ( -11.87243407472968926, 0.000000000000000000, 11.50246268866867361 ) ) ;
#514 = AXIS2_PLACEMENT_3D ( 'NONE', #20814, #20245, #54594 ) ;
#515 = DIRECTION ( 'NONE',  ( 0.6427681459581294776, -0.7660444431189769032, 0.005002170337467562802 ) ) ;
#516 = AXIS2_PLACEMENT_3D ( 'NONE', #41205, #19635, #11091 ) ;
#517 = DIRECTION ( 'NONE',  ( 0.5449076811759707706, 0.6444004775717708799, -0.5364919789714476250 ) ) ;
#518 = EDGE_CURVE ( 'NONE', #53934, #18987, #43004, .T. ) ;
#519 = DIRECTION ( 'NONE',  ( 0.007781995580012662783, 0.000000000000000000, -0.9999697198139514409 ) ) ;
#520 = DIRECTION ( 'NONE',  ( -0.5449076811759708816, 0.6444004775717707689, 0.5364919789714475140 ) ) ;
#521 = AXIS2_PLACEMENT_3D ( 'NONE', #2355, #53746, #14865 ) ;
#522 = EDGE_CURVE ( 'NONE', #20635, #3861, #4114, .T. ) ;
#523 = FACE_OUTER_BOUND ( 'NONE', #1524, .T. ) ;
#524 = VECTOR ( 'NONE', #3188, 999.9999999999998863 ) ;
#525 = DIRECTION ( 'NONE',  ( 0.007781995580012663651, 0.000000000000000000, -0.9999697198139515519 ) ) ;
#526 = EDGE_CURVE ( 'NONE', #25674, #51083, #56082, .T. ) ;
#527 = VECTOR ( 'NONE', #10360, 1000.000000000000227 ) ;
#528 = EDGE_CURVE ( 'NONE', #1446, #21707, #38460, .T. ) ;
#529 = EDGE_CURVE ( 'NONE', #49849, #20973, #21442, .T. ) ;
#530 = VERTEX_POINT ( 'NONE', #7826 ) ;
#531 = AXIS2_PLACEMENT_3D ( 'NONE', #51602, #12442, #13280 ) ;
#532 = VECTOR ( 'NONE', #47092, 1000.000000000000227 ) ;
#533 = ADVANCED_FACE ( 'NONE', ( #51248 ), #3542, .F. ) ;
#534 = AXIS2_PLACEMENT_3D ( 'NONE', #24826, #46384, #7499 ) ;
#535 = ORIENTED_EDGE ( 'NONE', *, *, #54295, .T. ) ;
#536 = VECTOR ( 'NONE', #8972, 999.9999999999998863 ) ;
#537 = ORIENTED_EDGE ( 'NONE', *, *, #7657, .T. ) ;
#538 = ORIENTED_EDGE ( 'NONE', *, *, #30952, .T. ) ;
#539 = ORIENTED_EDGE ( 'NONE', *, *, #36020, .F. ) ;
#540 = DIRECTION ( 'NONE',  ( 0.000000000000000000, -1.000000000000000000, 0.000000000000000000 ) ) ;
#541 = CARTESIAN_POINT ( 'NONE',  ( -29.86352658060627618, 0.000000000000000000, 8.481329010720569883 ) ) ;
#542 = ORIENTED_EDGE ( 'NONE', *, *, #52767, .T. ) ;
#543 = ORIENTED_EDGE ( 'NONE', *, *, #26233, .T. ) ;
#544 = EDGE_CURVE ( 'NONE', #8877, #51526, #29948, .T. ) ;
#545 = VECTOR ( 'NONE', #143, 1000.000000000000114 ) ;
#546 = DIRECTION ( 'NONE',  ( 0.007781995580012663651, 0.000000000000000000, -0.9999697198139515519 ) ) ;
#547 = VERTEX_POINT ( 'NONE', #50943 ) ;
#548 = EDGE_CURVE ( 'NONE', #41034, #45002, #12631, .T. ) ;
#549 = PLANE ( 'NONE',  #48198 ) ;
#550 = CARTESIAN_POINT ( 'NONE',  ( -18.76354595665420177, -0.1191753592594177458, 14.21882498613976331 ) ) ;
#551 = ORIENTED_EDGE ( 'NONE', *, *, #39784, .T. ) ;
#552 = VECTOR ( 'NONE', #28211, 1000.000000000000227 ) ;
#553 = CARTESIAN_POINT ( 'NONE',  ( 2.072287782118878319, 0.000000000000000000, -2.950529333540147015 ) ) ;
#554 = EDGE_LOOP ( 'NONE', ( #27214, #4765, #35761, #21660 ) ) ;
#555 = EDGE_CURVE ( 'NONE', #23263, #55993, #51792, .T. ) ;
#556 = DIRECTION ( 'NONE',  ( 0.007781995580012662783, 0.000000000000000000, -0.9999697198139514409 ) ) ;
#557 = VECTOR ( 'NONE', #29488, 999.9999999999998863 ) ;
#558 = EDGE_CURVE ( 'NONE', #9839, #31046, #34234, .T. ) ;
#559 = CARTESIAN_POINT ( 'NONE',  ( -16.72498074857254124, 0.000000000000000000, 3.951585318476526165 ) ) ;
#560 = CARTESIAN_POINT ( 'NONE',  ( -12.14776819164751309, 3.686347215771509145, 7.649850626033056322 ) ) ;
#561 = AXIS2_PLACEMENT_3D ( 'NONE', #36902, #10769, #32613 ) ;
#562 = VECTOR ( 'NONE', #9493, 1000.000000000000000 ) ;
#563 = VERTEX_POINT ( 'NONE', #20602 ) ;
#564 = DIRECTION ( 'NONE',  ( -0.005961354470445682716, -0.6427876096865404731, 0.7660212471507180654 ) ) ;
#565 = LINE ( 'NONE', #9928, #26557 ) ;
#566 = FACE_OUTER_BOUND ( 'NONE', #49151, .T. ) ;
#567 = ORIENTED_EDGE ( 'NONE', *, *, #4643, .T. ) ;
#568 = CARTESIAN_POINT ( 'NONE',  ( -24.26908309836554878, 0.000000000000000000, 6.108867788427308376 ) ) ;
#569 = ORIENTED_EDGE ( 'NONE', *, *, #49303, .F. ) ;
#570 = VECTOR ( 'NONE', #19577, 1000.000000000000227 ) ;
#571 = AXIS2_PLACEMENT_3D ( 'NONE', #25411, #12058, #16909 ) ;
#572 = CARTESIAN_POINT ( 'NONE',  ( -14.31835180280831032, 0.7721120973665051013, 3.710222702829293784 ) ) ;
#573 = LINE ( 'NONE', #48546, #32385 ) ;
#574 = CARTESIAN_POINT ( 'NONE',  ( -14.56888064431065821, -0.1191753592594197858, 12.58947452739191064 ) ) ;
#575 = CARTESIAN_POINT ( 'NONE',  ( -18.67775241435682432, 0.000000000000000000, 4.136394454059623804 ) ) ;
#576 = DIRECTION ( 'NONE',  ( -0.7660212471507179544, -0.6427876096865405842, -0.005961354470445141482 ) ) ;
#577 = DIRECTION ( 'NONE',  ( -0.005961354470445682716, -0.6427876096865404731, 0.7660212471507180654 ) ) ;
#578 = FACE_OUTER_BOUND ( 'NONE', #34988, .T. ) ;
#579 = AXIS2_PLACEMENT_3D ( 'NONE', #39286, #43295, #22800 ) ;
#580 = VECTOR ( 'NONE', #27612, 1000.000000000000227 ) ;
#581 = DIRECTION ( 'NONE',  ( -0.6427681459581293666, -0.7660444431189770143, -0.005002170337467561935 ) ) ;
#582 =( NAMED_UNIT ( * ) PLANE_ANGLE_UNIT ( ) SI_UNIT ( $, .RADIAN. ) );
#583 = DIRECTION ( 'NONE',  ( 0.007781995580012662783, 0.000000000000000000, -0.9999697198139514409 ) ) ;
#584 = ORIENTED_EDGE ( 'NONE', *, *, #25515, .T. ) ;
#585 = CARTESIAN_POINT ( 'NONE',  ( -29.86352658060627618, 0.000000000000000000, 8.481329010720569883 ) ) ;
#586 = DIRECTION ( 'NONE',  ( 0.005961354470445682716, -0.6427876096865404731, -0.7660212471507180654 ) ) ;
#587 = DIRECTION ( 'NONE',  ( 0.5364919789714477361, 0.6444004775717706579, 0.5449076811759711036 ) ) ;
#588 = FACE_OUTER_BOUND ( 'NONE', #19042, .T. ) ;
#589 = DIRECTION ( 'NONE',  ( 0.7660212471507180654, -0.6427876096865404731, 0.005961354470445141482 ) ) ;
#590 = CARTESIAN_POINT ( 'NONE',  ( -16.06709938707323460, 0.000000000000000000, 13.13181314741652628 ) ) ;
#591 = VECTOR ( 'NONE', #18457, 1000.000000000000227 ) ;
#592 = EDGE_LOOP ( 'NONE', ( #35703, #16663, #21212, #3946 ) ) ;
#593 = VERTEX_POINT ( 'NONE', #47249 ) ;
#594 = DIRECTION ( 'NONE',  ( 0.005002170337468016433, -0.7660444431189770143, -0.6427681459581293666 ) ) ;
#595 = CARTESIAN_POINT ( 'NONE',  ( -30.79411802867772607, 0.000000000000000000, 8.643412946479525516 ) ) ;
#596 = AXIS2_PLACEMENT_3D ( 'NONE', #22993, #40312, #41442 ) ;
#597 = ADVANCED_FACE ( 'NONE', ( #12900 ), #30231, .F. ) ;
#598 = ORIENTED_EDGE ( 'NONE', *, *, #54063, .F. ) ;
#599 = LINE ( 'NONE', #43470, #29524 ) ;
#600 = AXIS2_PLACEMENT_3D ( 'NONE', #53044, #795, #17864 ) ;
#601 = ORIENTED_EDGE ( 'NONE', *, *, #47560, .F. ) ;
#602 = DIRECTION ( 'NONE',  ( 0.5364919789714477361, 0.6444004775717706579, 0.5449076811759711036 ) ) ;
#603 = ADVANCED_FACE ( 'NONE', ( #16312 ), #46704, .F. ) ;
#604 = ADVANCED_FACE ( 'NONE', ( #8660 ), #46992, .F. ) ;
#605 = VECTOR ( 'NONE', #30042, 1000.000000000000227 ) ;
#606 = VERTEX_POINT ( 'NONE', #33927 ) ;
#607 = VERTEX_POINT ( 'NONE', #29699 ) ;
#608 = VERTEX_POINT ( 'NONE', #43310 ) ;
#609 = CARTESIAN_POINT ( 'NONE',  ( -19.53004645065075096, 0.000000000000000000, 6.145748067415055971 ) ) ;
#610 = PLANE ( 'NONE',  #25062 ) ;
#611 = DIRECTION ( 'NONE',  ( -0.6246952433987894571, 0.7422098413412802076, 0.2426528472758539834 ) ) ;
#612 = VECTOR ( 'NONE', #28011, 1000.000000000000227 ) ;
#613 = LINE ( 'NONE', #17941, #43776 ) ;
#614 = ORIENTED_EDGE ( 'NONE', *, *, #13717, .F. ) ;
#615 = ORIENTED_EDGE ( 'NONE', *, *, #49932, .F. ) ;
#616 = VECTOR ( 'NONE', #50544, 1000.000000000000000 ) ;
#617 = VECTOR ( 'NONE', #49691, 1000.000000000000000 ) ;
#618 = CARTESIAN_POINT ( 'NONE',  ( -24.26986129792355129, -0.1191753592594197858, 6.208864760408702388 ) ) ;
#619 = EDGE_LOOP ( 'NONE', ( #16851, #28850, #45454, #750 ) ) ;
#620 = DIRECTION ( 'NONE',  ( -0.6427681459581293666, -0.7660444431189770143, -0.005002170337467561935 ) ) ;
#621 = VERTEX_POINT ( 'NONE', #21132 ) ;
#622 = DIRECTION ( 'NONE',  ( 0.007781995580012663651, -3.146120232559066537E-19, -0.9999697198139514409 ) ) ;
#623 = LINE ( 'NONE', #13414, #8577 ) ;
#624 = ORIENTED_EDGE ( 'NONE', *, *, #35606, .T. ) ;
#625 = LINE ( 'NONE', #17951, #37691 ) ;
#626 = ORIENTED_EDGE ( 'NONE', *, *, #33083, .F. ) ;
#627 = EDGE_CURVE ( 'NONE', #9201, #34530, #21715, .T. ) ;
#628 = VECTOR ( 'NONE', #26135, 1000.000000000000000 ) ;
#629 = DIRECTION ( 'NONE',  ( 0.7660212471507180654, -0.6427876096865404731, 0.005961354470445141482 ) ) ;
#631 = ADVANCED_FACE ( 'NONE', ( #8097 ), #25681, .F. ) ;
#630 = ORIENTED_EDGE ( 'NONE', *, *, #51305, .F. ) ;
#632 = PLANE ( 'NONE',  #51220 ) ;
#633 = DIRECTION ( 'NONE',  ( 0.7660212471507180654, -0.6427876096865404731, 0.005961354470445141482 ) ) ;
#634 = PLANE ( 'NONE',  #54566 ) ;
#635 = EDGE_CURVE ( 'NONE', #12509, #54234, #44135, .T. ) ;
#636 = VERTEX_POINT ( 'NONE', #26809 ) ;
#637 = FACE_OUTER_BOUND ( 'NONE', #19734, .T. ) ;
#638 = CARTESIAN_POINT ( 'NONE',  ( -12.13851405436063047, 0.000000000000000000, 11.68505802764555135 ) ) ;
#639 = VECTOR ( 'NONE', #8987, 1000.000000000000227 ) ;
#640 = EDGE_CURVE ( 'NONE', #7467, #15470, #13194, .T. ) ;
#641 = CARTESIAN_POINT ( 'NONE',  ( -69.63135658628988267, 1.044799017367015193, 7.493821216008851316 ) ) ;
#642 = PLANE ( 'NONE',  #54018 ) ;
#643 = FACE_OUTER_BOUND ( 'NONE', #43485, .T. ) ;
#644 = CARTESIAN_POINT ( 'NONE',  ( -6.856675100204708606, -8.693987235299761807, 5.881739038249853557 ) ) ;
#645 = VECTOR ( 'NONE', #14355, 999.9999999999998863 ) ;
#646 = PLANE ( 'NONE',  #28564 ) ;
#647 = ORIENTED_EDGE ( 'NONE', *, *, #17303, .F. ) ;
#648 = LINE ( 'NONE', #35292, #46115 ) ;
#649 = LINE ( 'NONE', #10277, #15006 ) ;
#650 = DIRECTION ( 'NONE',  ( 0.5449076811759707706, 0.6444004775717708799, -0.5364919789714476250 ) ) ;
#651 = ORIENTED_EDGE ( 'NONE', *, *, #50347, .T. ) ;
#652 = DIRECTION ( 'NONE',  ( 0.000000000000000000, -0.000000000000000000, -1.000000000000000000 ) ) ;
#653 = CARTESIAN_POINT ( 'NONE',  ( 4.930947970565944694, -1.129146301979397693, 1.967953638241001446 ) ) ;
#654 = EDGE_LOOP ( 'NONE', ( #18887, #14699, #6276, #17282 ) ) ;
#655 = DIRECTION ( 'NONE',  ( 0.6427681459581294776, -0.7660444431189769032, 0.005002170337467562802 ) ) ;
#656 = AXIS2_PLACEMENT_3D ( 'NONE', #49372, #27815, #45127 ) ;
#657 = CARTESIAN_POINT ( 'NONE',  ( -32.65841372305263235, 0.000000000000000000, 9.367568705923016381 ) ) ;
#658 = LINE ( 'NONE', #8914, #45018 ) ;
#659 = FACE_OUTER_BOUND ( 'NONE', #24133, .T. ) ;
#660 = EDGE_LOOP ( 'NONE', ( #9631, #12538, #45330, #12184 ) ) ;
#661 = VERTEX_POINT ( 'NONE', #44397 ) ;
#662 = PLANE ( 'NONE',  #17637 ) ;
#663 = CARTESIAN_POINT ( 'NONE',  ( -13.07066190154808361, 0.000000000000000000, 12.04713590736729678 ) ) ;
#664 = DIRECTION ( 'NONE',  ( -0.6427681459581293666, -0.7660444431189770143, -0.005002170337467561935 ) ) ;
#665 = ADVANCED_FACE ( 'NONE', ( #14026 ), #9200, .F. ) ;
#666 = CARTESIAN_POINT ( 'NONE',  ( -17.73140113748535285, 0.000000000000000000, 13.85752530597602039 ) ) ;
#667 = EDGE_CURVE ( 'NONE', #48589, #43836, #26245, .T. ) ;
#668 = CARTESIAN_POINT ( 'NONE',  ( -14.15179153153711944, -3.594132820645663084, 2.263685890564126613 ) ) ;
#669 = DIRECTION ( 'NONE',  ( -0.5364919789714478471, 0.6444004775717705469, -0.5449076811759709926 ) ) ;
#670 = ORIENTED_EDGE ( 'NONE', *, *, #55307, .F. ) ;
#671 = LINE ( 'NONE', #17991, #33788 ) ;
#672 = EDGE_CURVE ( 'NONE', #23998, #48095, #5247, .T. ) ;
#673 = DIRECTION ( 'NONE',  ( 0.007781995580012663651, 0.000000000000000000, -0.9999697198139515519 ) ) ;
#674 = ORIENTED_EDGE ( 'NONE', *, *, #1413, .T. ) ;
#675 = DIRECTION ( 'NONE',  ( 0.2113248654051873565, 0.7886751345948123104, 0.5773502691896265082 ) ) ;
#676 = LINE ( 'NONE', #5229, #15931 ) ;
#677 = DIRECTION ( 'NONE',  ( 0.9999697198139515519, 0.000000000000000000, 0.007781995580013368816 ) ) ;
#678 = VERTEX_POINT ( 'NONE', #1225 ) ;
#679 = CARTESIAN_POINT ( 'NONE',  ( -14.93495759592298988, 0.000000000000000000, 12.77129166681078409 ) ) ;
#680 = ORIENTED_EDGE ( 'NONE', *, *, #9478, .T. ) ;
#681 = EDGE_CURVE ( 'NONE', #23840, #12179, #22555, .T. ) ;
#682 = VERTEX_POINT ( 'NONE', #21973 ) ;
#683 = AXIS2_PLACEMENT_3D ( 'NONE', #13512, #43590, #4698 ) ;
#684 = ORIENTED_EDGE ( 'NONE', *, *, #35245, .F. ) ;
#685 =( BOUNDED_SURFACE ( )  B_SPLINE_SURFACE ( 3, 2, ( 
 ( #15116, #40673, #41213 ),
 ( #40925, #15367, #2009 ),
 ( #44927, #36680, #10586 ),
 ( #28148, #36390, #6041 ),
 ( #45740, #50283, #49989 ),
 ( #19904, #11101, #45457 ),
 ( #10837, #28728, #2308 ),
 ( #24185, #6868, #23354 ),
 ( #1745, #11397, #28423 ),
 ( #45205, #10278, #53441 ),
 ( #19067, #14539, #27899 ),
 ( #6572, #36975, #5739 ),
 ( #23063, #6307, #41503 ),
 ( #54273, #19644, #32439 ),
 ( #32683, #2586, #37220 ),
 ( #53703, #54524, #40385 ),
 ( #49165, #15631, #14818 ),
 ( #32970, #27603, #31853 ),
 ( #1480, #32145, #49470 ),
 ( #18819, #23610, #19344 ),
 ( #53999, #36140, #49740 ),
 ( #23885, #12789, #11933 ),
 ( #42345, #38343, #25300 ),
 ( #33807, #42604, #51427 ),
 ( #41750, #37811, #12527 ),
 ( #7144, #33274, #34109 ),
 ( #3698, #29846, #24716 ),
 ( #54824, #34380, #55668 ) ),
 .UNSPECIFIED., .F., .F., .T. ) 
 B_SPLINE_SURFACE_WITH_KNOTS ( ( 4, 2, 2, 2, 2, 2, 2, 2, 2, 2, 2, 2, 2, 4 ),
 ( 3, 3 ),
 ( 0.005951394764495079696, 0.008223488340404871977, 0.009359535128359769418, 0.01049558191631466512, 0.01276767549222445827, 0.01390372228017935571, 0.01503976906813425142, 0.01617581585608914713, 0.01731186264404404457, 0.01958395621995383598, 0.02072000300790872995, 0.02185604979586362739, 0.02299209658381852484, 0.02412814337177342228 ),
 ( 0.000000000000000000, 1.000000000000000000 ),
 .UNSPECIFIED. ) 
 GEOMETRIC_REPRESENTATION_ITEM ( )  RATIONAL_B_SPLINE_SURFACE ( (
 ( 1.000000000000000000, 0.9218171296615420562, 1.000000000000000000),
 ( 1.000000000000000000, 0.9219582590456437687, 1.000000000000000000),
 ( 1.000000000000000000, 0.9217654209472763149, 1.000000000000000000),
 ( 1.000000000000000000, 0.9218193965238216103, 1.000000000000000000),
 ( 1.000000000000000000, 0.9217886515250015567, 1.000000000000000000),
 ( 1.000000000000000000, 0.9217705453232085677, 1.000000000000000000),
 ( 1.000000000000000000, 0.9217728555239398380, 1.000000000000000000),
 ( 1.000000000000000000, 0.9217839018313299659, 1.000000000000000000),
 ( 1.000000000000000000, 0.9217902773711394993, 1.000000000000000000),
 ( 1.000000000000000000, 0.9218159477363486731, 1.000000000000000000),
 ( 1.000000000000000000, 0.9218381644591753243, 1.000000000000000000),
 ( 1.000000000000000000, 0.9218170478689924341, 1.000000000000000000),
 ( 1.000000000000000000, 0.9218183721981643153, 1.000000000000000000),
 ( 1.000000000000000000, 0.9218243750428467553, 1.000000000000000000),
 ( 1.000000000000000000, 0.9218291361982778875, 1.000000000000000000),
 ( 1.000000000000000000, 0.9218339850783857647, 1.000000000000000000),
 ( 1.000000000000000000, 0.9218340914611712344, 1.000000000000000000),
 ( 1.000000000000000000, 0.9218311426327383540, 1.000000000000000000),
 ( 1.000000000000000000, 0.9218408506515718415, 1.000000000000000000),
 ( 1.000000000000000000, 0.9218298856236216698, 1.000000000000000000),
 ( 1.000000000000000000, 0.9218235216668148047, 1.000000000000000000),
 ( 1.000000000000000000, 0.9218049054835019129, 1.000000000000000000),
 ( 1.000000000000000000, 0.9217926302239767278, 1.000000000000000000),
 ( 1.000000000000000000, 0.9217749384505029564, 1.000000000000000000),
 ( 1.000000000000000000, 0.9217695517188592147, 1.000000000000000000),
 ( 1.000000000000000000, 0.9217886187906866313, 1.000000000000000000),
 ( 1.000000000000000000, 0.9218984684751942993, 1.000000000000000000),
 ( 1.000000000000000000, 0.9217608302862917435, 1.000000000000000000) ) ) 
 REPRESENTATION_ITEM ( '' )  SURFACE ( )  );
#686 = ORIENTED_EDGE ( 'NONE', *, *, #20248, .T. ) ;
#687 = DIRECTION ( 'NONE',  ( 0.5364919789714477361, 0.6444004775717706579, 0.5449076811759711036 ) ) ;
#688 = ORIENTED_EDGE ( 'NONE', *, *, #44373, .T. ) ;
#689 = CYLINDRICAL_SURFACE ( 'NONE', #24963, 5.241923709989091407 ) ;
#690 = VECTOR ( 'NONE', #32497, 999.9999999999998863 ) ;
#691 = ORIENTED_EDGE ( 'NONE', *, *, #53911, .F. ) ;
#692 = LINE ( 'NONE', #17737, #6878 ) ;
#693 = VERTEX_POINT ( 'NONE', #18268 ) ;
#694 = CARTESIAN_POINT ( 'NONE',  ( -30.79489622823572859, -0.1191753592594197858, 8.743409918460921304 ) ) ;
#695 = VERTEX_POINT ( 'NONE', #5499 ) ;
#696 = CARTESIAN_POINT ( 'NONE',  ( -11.33208760941060333, 0.000000000000000000, 1.777561641030050543 ) ) ;
#697 = CARTESIAN_POINT ( 'NONE',  ( -23.39689027546016220, 18.96061615304027370, 4.493364425890089109 ) ) ;
#698 = DIRECTION ( 'NONE',  ( 0.5449076811759707706, 0.6444004775717708799, -0.5364919789714476250 ) ) ;
#699 = DIRECTION ( 'NONE',  ( 0.5364919789714477361, 0.6444004775717706579, 0.5449076811759711036 ) ) ;
#700 = FACE_OUTER_BOUND ( 'NONE', #10945, .T. ) ;
#701 = ORIENTED_EDGE ( 'NONE', *, *, #46881, .T. ) ;
#702 = ORIENTED_EDGE ( 'NONE', *, *, #51890, .F. ) ;
#703 = DIRECTION ( 'NONE',  ( 0.5449076811759707706, 0.6444004775717708799, -0.5364919789714476250 ) ) ;
#704 = EDGE_CURVE ( 'NONE', #51394, #48900, #35074, .T. ) ;
#705 = PLANE ( 'NONE',  #42988 ) ;
#706 = CARTESIAN_POINT ( 'NONE',  ( -17.92576495860976493, -3.594132820645661308, 9.543491873778670254 ) ) ;
#707 = LINE ( 'NONE', #5517, #23983 ) ;
#708 = LINE ( 'NONE', #56098, #4999 ) ;
#709 = CARTESIAN_POINT ( 'NONE',  ( -70.02519189693502710, -0.1222117011752772570, -7.502262482362483276 ) ) ;
#710 = ORIENTED_EDGE ( 'NONE', *, *, #19298, .F. ) ;
#711 = CARTESIAN_POINT ( 'NONE',  ( -11.16526465312192506, 0.000000000000000000, 6.041518719944250826 ) ) ;
#712 = CARTESIAN_POINT ( 'NONE',  ( -18.61514292449499663, 0.000000000000000000, 7.999528407239896666 ) ) ;
#713 = VERTEX_POINT ( 'NONE', #30793 ) ;
#714 = EDGE_CURVE ( 'NONE', #18910, #36080, #39864, .T. ) ;
#715 = LINE ( 'NONE', #35102, #2539 ) ;
#716 = DIRECTION ( 'NONE',  ( -0.5364919789714478471, 0.6444004775717705469, -0.5449076811759709926 ) ) ;
#717 = FACE_OUTER_BOUND ( 'NONE', #44823, .T. ) ;
#718 = EDGE_CURVE ( 'NONE', #14438, #53765, #392, .T. ) ;
#719 = EDGE_CURVE ( 'NONE', #45990, #23916, #47841, .T. ) ;
#720 = CARTESIAN_POINT ( 'NONE',  ( -28.93137873341882127, 0.000000000000000000, 8.119251130998824451 ) ) ;
#721 = CARTESIAN_POINT ( 'NONE',  ( -11.19767518203325807, -2.298917212465660054, 1.157530937302438057 ) ) ;
#722 = VERTEX_POINT ( 'NONE', #35907 ) ;
#723 = ORIENTED_EDGE ( 'NONE', *, *, #7385, .F. ) ;
#724 = LINE ( 'NONE', #22590, #4018 ) ;
#725 = PLANE ( 'NONE',  #5945 ) ;
#726 = CARTESIAN_POINT ( 'NONE',  ( -8.409922665610809034, 0.000000000000000000, 10.23674650875856962 ) ) ;
#727 = EDGE_CURVE ( 'NONE', #44683, #32191, #692, .T. ) ;
#728 = VECTOR ( 'NONE', #25296, 999.9999999999998863 ) ;
#729 = CARTESIAN_POINT ( 'NONE',  ( -13.20656186341736316, 0.000000000000000000, 3.809640454209623606 ) ) ;
#730 = EDGE_CURVE ( 'NONE', #36112, #44493, #22276, .T. ) ;
#731 = LINE ( 'NONE', #17782, #17679 ) ;
#732 = CARTESIAN_POINT ( 'NONE',  ( -16.70782865829815833, 23.01200647243835462, -4.019104856592038644 ) ) ;
#733 = DIRECTION ( 'NONE',  ( -0.7660212471507179544, -0.6427876096865405842, -0.005961354470445141482 ) ) ;
#734 = EDGE_CURVE ( 'NONE', #931, #20189, #34762, .T. ) ;
#735 = LINE ( 'NONE', #27135, #14181 ) ;
#736 = CARTESIAN_POINT ( 'NONE',  ( -10.47421230394850866, 0.000000000000000000, 10.95934586908605723 ) ) ;
#737 = EDGE_LOOP ( 'NONE', ( #27448, #47886, #41645, #33349 ) ) ;
#738 = FACE_OUTER_BOUND ( 'NONE', #7670, .T. ) ;
#739 = EDGE_LOOP ( 'NONE', ( #34761, #3095, #2567, #15272 ) ) ;
#740 = LINE ( 'NONE', #40192, #35004 ) ;
#741 = CARTESIAN_POINT ( 'NONE',  ( -13.11188176427955021, -5.051250379848162275, 10.06499431649357135 ) ) ;
#742 = ADVANCED_FACE ( 'NONE', ( #43558 ), #48679, .F. ) ;
#743 = EDGE_LOOP ( 'NONE', ( #16734, #26904, #34478, #37376 ) ) ;
#744 = CARTESIAN_POINT ( 'NONE',  ( -19.53447690327204000, 0.000000000000000000, 6.715051714635608349 ) ) ;
#745 = ORIENTED_EDGE ( 'NONE', *, *, #46697, .F. ) ;
#746 = EDGE_CURVE ( 'NONE', #48518, #40704, #31739, .T. ) ;
#747 = EDGE_LOOP ( 'NONE', ( #1784, #12752, #14548, #47746 ) ) ;
#748 = EDGE_LOOP ( 'NONE', ( #4796, #32251, #45492, #46225 ) ) ;
#749 = CARTESIAN_POINT ( 'NONE',  ( -22.40556560354864146, -0.1191753592594197858, 5.484709000965211523 ) ) ;
#750 = ORIENTED_EDGE ( 'NONE', *, *, #21517, .T. ) ;
#751 = ORIENTED_EDGE ( 'NONE', *, *, #19934, .F. ) ;
#752 = DIRECTION ( 'NONE',  ( -0.9999697198139514409, -0.000000000000000000, -0.007781995580013368816 ) ) ;
#753 = CARTESIAN_POINT ( 'NONE',  ( -15.06223539727642446, 0.000000000000000000, 3.425867103879820519 ) ) ;
#754 = EDGE_LOOP ( 'NONE', ( #38885, #6213, #1229, #11222 ) ) ;
#755 = EDGE_LOOP ( 'NONE', ( #56123, #8490, #39156, #20788 ) ) ;
#756 = CARTESIAN_POINT ( 'NONE',  ( -57.52614991588065152, -8.291364278369169227, 3.000000000000006661 ) ) ;
#757 = ORIENTED_EDGE ( 'NONE', *, *, #46611, .F. ) ;
#758 = ORIENTED_EDGE ( 'NONE', *, *, #26540, .F. ) ;
#759 = DIRECTION ( 'NONE',  ( 0.5449076811759707706, 0.6444004775717708799, -0.5364919789714476250 ) ) ;
#760 = CARTESIAN_POINT ( 'NONE',  ( -19.69569380384165669, -0.1191753592594177458, 14.58090286586150697 ) ) ;
#761 = CARTESIAN_POINT ( 'NONE',  ( -67.73103538350329700, -11.31014138737506336, -7.469194291234003913 ) ) ;
#762 = ORIENTED_EDGE ( 'NONE', *, *, #37791, .F. ) ;
#763 = FACE_OUTER_BOUND ( 'NONE', #43535, .T. ) ;
#764 = EDGE_LOOP ( 'NONE', ( #4573, #19800, #42115, #4177 ) ) ;
#765 = CIRCLE ( 'NONE', #52451, 6.999999999999988454 ) ;
#766 = EDGE_CURVE ( 'NONE', #40769, #6080, #17627, .T. ) ;
#767 = DIRECTION ( 'NONE',  ( 0.7660212471507180654, -0.6427876096865404731, 0.005961354470445141482 ) ) ;
#768 = CARTESIAN_POINT ( 'NONE',  ( -17.73140113748535285, 0.000000000000000000, 13.85752530597602039 ) ) ;
#769 = CARTESIAN_POINT ( 'NONE',  ( -18.33768610320628767, 0.000000000000000000, 6.355033347565870017 ) ) ;
#770 = CARTESIAN_POINT ( 'NONE',  ( -18.13038765311693368, 0.000000000000000000, 5.417976396203555645 ) ) ;
#771 = CARTESIAN_POINT ( 'NONE',  ( 6.057149959413268725, -0.9999999855073579136, 0.7725409890818936143 ) ) ;
#772 = DIRECTION ( 'NONE',  ( 0.6427681459581294776, -0.7660444431189769032, 0.005002170337467562802 ) ) ;
#773 = LINE ( 'NONE', #5051, #27725 ) ;
#774 = ORIENTED_EDGE ( 'NONE', *, *, #17283, .T. ) ;
#775 = LINE ( 'NONE', #14417, #8425 ) ;
#776 = ADVANCED_FACE ( 'NONE', ( #4006 ), #51696, .F. ) ;
#777 = CARTESIAN_POINT ( 'NONE',  ( -15.78376999578702211, 1.419719901456505617, 2.767587519033712695 ) ) ;
#778 = DIRECTION ( 'NONE',  ( -0.9999697198139514409, -0.000000000000000000, -0.007781995580013368816 ) ) ;
#779 = DIRECTION ( 'NONE',  ( -0.5449076811759708816, 0.6444004775717707689, 0.5364919789714475140 ) ) ;
#780 = CARTESIAN_POINT ( 'NONE',  ( -20.79248460937205323, 18.92167845196996367, -4.386225263874957037 ) ) ;
#781 = FACE_OUTER_BOUND ( 'NONE', #23886, .T. ) ;
#782 = EDGE_CURVE ( 'NONE', #48488, #51983, #46900, .T. ) ;
#783 = CARTESIAN_POINT ( 'NONE',  ( -20.26176469941677993, 0.000000000000000000, 14.76116360616437895 ) ) ;
#784 = DIRECTION ( 'NONE',  ( 0.5449076811759707706, 0.6444004775717708799, -0.5364919789714476250 ) ) ;
#785 = EDGE_LOOP ( 'NONE', ( #49145, #47097, #14506, #35154 ) ) ;
#786 = LINE ( 'NONE', #27189, #22992 ) ;
#787 = DIRECTION ( 'NONE',  ( 0.6427681459581294776, -0.7660444431189769032, 0.005002170337467562802 ) ) ;
#788 = CARTESIAN_POINT ( 'NONE',  ( -20.21451535923326048, 0.000000000000000000, 5.601763288707669375 ) ) ;
#789 = CARTESIAN_POINT ( 'NONE',  ( -25.20123094555300369, 0.000000000000000000, 6.470945668149052032 ) ) ;
#790 = ADVANCED_FACE ( 'NONE', ( #42897 ), #30124, .F. ) ;
#791 = DIRECTION ( 'NONE',  ( 0.5364919789714477361, 0.6444004775717706579, 0.5449076811759711036 ) ) ;
#792 = CARTESIAN_POINT ( 'NONE',  ( -17.36532418587302473, -0.1191753592594177458, 13.67570816655714516 ) ) ;
#793 = LINE ( 'NONE', #34887, #12928 ) ;
#794 = ADVANCED_FACE ( 'NONE', ( #30422 ), #47438, .F. ) ;
#795 = DIRECTION ( 'NONE',  ( 0.005961354470445682716, -0.6427876096865404731, -0.7660212471507180654 ) ) ;
#796 = DIRECTION ( 'NONE',  ( 0.000000000000000000, -0.000000000000000000, -1.000000000000000000 ) ) ;
#797 = EDGE_CURVE ( 'NONE', #8862, #33893, #21029, .T. ) ;
#798 = AXIS2_PLACEMENT_3D ( 'NONE', #26207, #47495, #43510 ) ;
#799 = ORIENTED_EDGE ( 'NONE', *, *, #34159, .F. ) ;
#800 = EDGE_LOOP ( 'NONE', ( #34379, #40262, #53179, #16521 ) ) ;
#801 = EDGE_LOOP ( 'NONE', ( #50622, #1176, #31607, #10321 ) ) ;
#802 = ORIENTED_EDGE ( 'NONE', *, *, #22600, .F. ) ;
#803 = EDGE_LOOP ( 'NONE', ( #41732, #40202, #30983, #54274 ) ) ;
#804 = CARTESIAN_POINT ( 'NONE',  ( -20.92640044469605698, -1.651309408375657428, 7.520536391179072133 ) ) ;
#805 = DIRECTION ( 'NONE',  ( 0.005002170337468016433, -0.7660444431189770143, -0.6427681459581293666 ) ) ;
#806 = ORIENTED_EDGE ( 'NONE', *, *, #27941, .T. ) ;
#807 = ORIENTED_EDGE ( 'NONE', *, *, #43920, .T. ) ;
#808 = CARTESIAN_POINT ( 'NONE',  ( -14.87373766733476543, 0.000000000000000000, 4.904662316026882074 ) ) ;
#809 = ORIENTED_EDGE ( 'NONE', *, *, #21309, .T. ) ;
#810 = DIRECTION ( 'NONE',  ( 0.007781995580012662783, 0.000000000000000000, -0.9999697198139514409 ) ) ;
#811 = CARTESIAN_POINT ( 'NONE',  ( -13.97686547933248313, 0.9340140483890051470, 2.081221001769270718 ) ) ;
#812 = EDGE_LOOP ( 'NONE', ( #7481, #934, #10633, #30423 ) ) ;
#813 = PLANE ( 'NONE',  #17394 ) ;
#814 = ADVANCED_FACE ( 'NONE', ( #34965 ), #21621, .F. ) ;
#815 = ORIENTED_EDGE ( 'NONE', *, *, #55028, .T. ) ;
#816 = LINE ( 'NONE', #31202, #6482 ) ;
#817 = EDGE_CURVE ( 'NONE', #29054, #35683, #8551, .T. ) ;
#818 = DIRECTION ( 'NONE',  ( 0.000000000000000000, 1.000000000000000000, 0.000000000000000000 ) ) ;
#819 = CARTESIAN_POINT ( 'NONE',  ( -16.43317633868556626, -0.1191753592594197858, 13.31363028683540151 ) ) ;
#820 = DIRECTION ( 'NONE',  ( 0.9999697198139515519, 0.000000000000000000, 0.007781995580013368816 ) ) ;
#821 = ORIENTED_EDGE ( 'NONE', *, *, #1158, .F. ) ;
#822 = CARTESIAN_POINT ( 'NONE',  ( 2.072287782118878319, 0.000000000000000000, -2.950529333540147015 ) ) ;
#823 = LINE ( 'NONE', #4809, #12037 ) ;
#824 = DIRECTION ( 'NONE',  ( -0.9999697198139514409, -0.000000000000000000, -0.007781995580013368816 ) ) ;
#825 = EDGE_CURVE ( 'NONE', #18340, #40757, #55982, .T. ) ;
#826 = ORIENTED_EDGE ( 'NONE', *, *, #31707, .T. ) ;
#827 = CARTESIAN_POINT ( 'NONE',  ( -15.03495456790438389, -0.1191753592594197858, 12.77051346725278158 ) ) ;
#828 = ORIENTED_EDGE ( 'NONE', *, *, #6980, .T. ) ;
#829 = ADVANCED_FACE ( 'NONE', ( #7709 ), #51441, .F. ) ;
#830 = ADVANCED_FACE ( 'NONE', ( #43211 ), #17330, .F. ) ;
#831 = EDGE_CURVE ( 'NONE', #12964, #15779, #47153, .T. ) ;
#832 = AXIS2_PLACEMENT_3D ( 'NONE', #32437, #46287, #42036 ) ;
#833 = LINE ( 'NONE', #9080, #34650 ) ;
#834 = CARTESIAN_POINT ( 'NONE',  ( -22.40478740399063895, 0.000000000000000000, 5.384712028983816623 ) ) ;
#835 = CARTESIAN_POINT ( 'NONE',  ( -17.91524326081876950, 4.981562823951510843, 12.01580327878066790 ) ) ;
#836 = CARTESIAN_POINT ( 'NONE',  ( -19.52010663574562344, 0.000000000000000000, 4.868503198346786576 ) ) ;
#837 = LINE ( 'NONE', #17906, #4175 ) ;
#838 = DIRECTION ( 'NONE',  ( -0.6246952433987894571, 0.7422098413412802076, 0.2426528472758539834 ) ) ;
#839 = CARTESIAN_POINT ( 'NONE',  ( -15.10378980073966204, 0.000000000000000000, 8.765518708783501367 ) ) ;
#840 = CARTESIAN_POINT ( 'NONE',  ( -19.58700580672034519, -2.298917212465660054, 4.416231854798146728 ) ) ;
#841 = FILL_AREA_STYLE_COLOUR ( '', #31666 ) ;
#842 = FACE_OUTER_BOUND ( 'NONE', #30586, .T. ) ;
#843 = ORIENTED_EDGE ( 'NONE', *, *, #24261, .T. ) ;
#844 = LINE ( 'NONE', #18163, #21196 ) ;
#845 = DIRECTION ( 'NONE',  ( 0.7660212471507180654, -0.6427876096865404731, 0.005961354470445141482 ) ) ;
#846 = DIRECTION ( 'NONE',  ( 0.7660212471507180654, -0.6427876096865404731, 0.005961354470445141482 ) ) ;
#847 = CARTESIAN_POINT ( 'NONE',  ( -15.87975247367846166, 0.000000000000000000, 2.850166870931599927 ) ) ;
#848 = FACE_OUTER_BOUND ( 'NONE', #36100, .T. ) ;
#849 = EDGE_CURVE ( 'NONE', #38597, #41331, #1, .T. ) ;
#850 = DIRECTION ( 'NONE',  ( 0.9999697198139515519, 0.000000000000000000, 0.007781995580013368816 ) ) ;
#851 = EDGE_CURVE ( 'NONE', #6183, #53549, #4564, .T. ) ;
#852 = DIRECTION ( 'NONE',  ( -0.9999697198139514409, -0.000000000000000000, -0.007781995580013368816 ) ) ;
#853 = ORIENTED_EDGE ( 'NONE', *, *, #11175, .F. ) ;
#854 = ADVANCED_FACE ( 'NONE', ( #3448 ), #20765, .F. ) ;
#855 = ORIENTED_EDGE ( 'NONE', *, *, #28585, .T. ) ;
#856 = ADVANCED_FACE ( 'NONE', ( #33820 ), #23304, .F. ) ;
#857 = DIRECTION ( 'NONE',  ( 0.9999697198139515519, 0.000000000000000000, 0.007781995580013368816 ) ) ;
#858 = DIRECTION ( 'NONE',  ( -0.005002170337468016433, -0.7660444431189770143, 0.6427681459581293666 ) ) ;
#859 = ADVANCED_FACE ( 'NONE', ( #52543 ), #1124, .F. ) ;
#860 = ORIENTED_EDGE ( 'NONE', *, *, #9914, .T. ) ;
#861 = DIRECTION ( 'NONE',  ( 0.5364919789714477361, 0.6444004775717706579, 0.5449076811759711036 ) ) ;
#862 = ORIENTED_EDGE ( 'NONE', *, *, #20952, .F. ) ;
#863 = CARTESIAN_POINT ( 'NONE',  ( -9.772671616987951282, 0.000000000000000000, 6.221682214543255540 ) ) ;
#864 = EDGE_CURVE ( 'NONE', #18999, #53740, #1426, .T. ) ;
#865 = ORIENTED_EDGE ( 'NONE', *, *, #18651, .T. ) ;
#866 = VERTEX_POINT ( 'NONE', #18458 ) ;
#867 = ORIENTED_EDGE ( 'NONE', *, *, #30697, .F. ) ;
#868 = CARTESIAN_POINT ( 'NONE',  ( -13.53673582514181106, 0.000000000000000000, 12.22817484722816772 ) ) ;
#869 = DIRECTION ( 'NONE',  ( 0.007781995580012662783, 0.000000000000000000, -0.9999697198139514409 ) ) ;
#870 = CARTESIAN_POINT ( 'NONE',  ( -25.20123094555300369, 0.000000000000000000, 6.470945668149052032 ) ) ;
#871 = ORIENTED_EDGE ( 'NONE', *, *, #22259, .F. ) ;
#872 = CARTESIAN_POINT ( 'NONE',  ( -15.86710544311044302, 0.000000000000000000, 13.13336954653252953 ) ) ;
#873 = VERTEX_POINT ( 'NONE', #14235 ) ;
#874 = ORIENTED_EDGE ( 'NONE', *, *, #20758, .T. ) ;
#875 = CARTESIAN_POINT ( 'NONE',  ( -14.13140520447825388, 0.000000000000000000, 3.233104983453049641 ) ) ;
#876 = ORIENTED_EDGE ( 'NONE', *, *, #34204, .F. ) ;
#877 = DIRECTION ( 'NONE',  ( -0.005961354470445682716, -0.6427876096865404731, 0.7660212471507180654 ) ) ;
#878 = ORIENTED_EDGE ( 'NONE', *, *, #14782, .T. ) ;
#879 = CARTESIAN_POINT ( 'NONE',  ( 2.072287782118878319, 0.000000000000000000, -2.950529333540147015 ) ) ;
#880 = DIRECTION ( 'NONE',  ( 0.007781995580012663651, 0.000000000000000000, -0.9999697198139515519 ) ) ;
#881 = ORIENTED_EDGE ( 'NONE', *, *, #130, .F. ) ;
#882 = DIRECTION ( 'NONE',  ( 0.000000000000000000, -1.000000000000000000, 0.000000000000000000 ) ) ;
#883 = VERTEX_POINT ( 'NONE', #40037 ) ;
#884 = LINE ( 'NONE', #45187, #36368 ) ;
#885 = ORIENTED_EDGE ( 'NONE', *, *, #21590, .F. ) ;
#886 = CARTESIAN_POINT ( 'NONE',  ( -18.39746900504187010, 0.000000000000000000, 14.03700784672088808 ) ) ;
#887 = CARTESIAN_POINT ( 'NONE',  ( -13.16225250642930078, -4.079838673713163111, 1.863818768663334069 ) ) ;
#888 = DIRECTION ( 'NONE',  ( -0.5449076811759708816, 0.6444004775717707689, 0.5364919789714475140 ) ) ;
#889 = ORIENTED_EDGE ( 'NONE', *, *, #10422, .T. ) ;
#890 = EDGE_CURVE ( 'NONE', #5503, #38452, #22724, .T. ) ;
#891 = EDGE_CURVE ( 'NONE', #14388, #9720, #9381, .T. ) ;
#892 = LINE ( 'NONE', #47788, #42868 ) ;
#893 = LINE ( 'NONE', #48893, #11053 ) ;
#894 = DIRECTION ( 'NONE',  ( 0.9999697198139515519, 0.000000000000000000, 0.007781995580013368816 ) ) ;
#895 = CARTESIAN_POINT ( 'NONE',  ( -17.55224900710100044, -2.653845599528779520, 12.45560879478165184 ) ) ;
#896 = ADVANCED_FACE ( 'NONE', ( #27003 ), #35798, .F. ) ;
#897 = FACE_OUTER_BOUND ( 'NONE', #29201, .T. ) ;
#898 = CARTESIAN_POINT ( 'NONE',  ( -14.19192946519435417, 1.743523803501506375, 2.138931558044772085 ) ) ;
#899 = AXIS2_PLACEMENT_3D ( 'NONE', #35422, #22386, #47649 ) ;
#900 = ORIENTED_EDGE ( 'NONE', *, *, #52309, .T. ) ;
#901 = LINE ( 'NONE', #53997, #50661 ) ;
#902 = CARTESIAN_POINT ( 'NONE',  ( -16.52924358339377164, 5.629170628041515023, 2.922851259777623500 ) ) ;
#903 = CARTESIAN_POINT ( 'NONE',  ( -13.14027533394136071, -0.1191753592594181482, 8.142138120879399921 ) ) ;
#904 = VERTEX_POINT ( 'NONE', #40625 ) ;
#905 = DIRECTION ( 'NONE',  ( -0.6427681459581293666, -0.7660444431189770143, -0.005002170337467561935 ) ) ;
#906 = DIRECTION ( 'NONE',  ( -0.7660212471507179544, -0.6427876096865405842, -0.005961354470445141482 ) ) ;
#907 = ORIENTED_EDGE ( 'NONE', *, *, #38915, .F. ) ;
#908 = PLANE ( 'NONE',  #55197 ) ;
#909 = CARTESIAN_POINT ( 'NONE',  ( -17.73140113748535285, 0.000000000000000000, 13.85752530597602039 ) ) ;
#910 = DIRECTION ( 'NONE',  ( -0.5364919789714478471, 0.6444004775717705469, -0.5449076811759709926 ) ) ;
#911 = EDGE_CURVE ( 'NONE', #21477, #24227, #26703, .T. ) ;
#912 = CARTESIAN_POINT ( 'NONE',  ( -16.95658928109344288, 0.000000000000000000, 8.012435655195931261 ) ) ;
#913 = ORIENTED_EDGE ( 'NONE', *, *, #52568, .F. ) ;
#914 = ORIENTED_EDGE ( 'NONE', *, *, #11163, .T. ) ;
#915 = CARTESIAN_POINT ( 'NONE',  ( -18.32044178217458708, 0.000000000000000000, 4.139175128019283001 ) ) ;
#916 = DIRECTION ( 'NONE',  ( 0.007781995580012662783, 0.000000000000000000, -0.9999697198139514409 ) ) ;
#917 = CARTESIAN_POINT ( 'NONE',  ( -21.47419595591918906, 0.000000000000000000, 5.222628093224860102 ) ) ;
#918 = DIRECTION ( 'NONE',  ( 0.5364919789714477361, 0.6444004775717706579, 0.5449076811759711036 ) ) ;
#919 = CARTESIAN_POINT ( 'NONE',  ( -50.99228148001754590, 2.341865487272627000, 5.000000000000000000 ) ) ;
#920 = CARTESIAN_POINT ( 'NONE',  ( -12.08304223278296874, 0.000000000000000000, 4.557048083377176262 ) ) ;
#921 = ORIENTED_EDGE ( 'NONE', *, *, #19041, .F. ) ;
#922 = CARTESIAN_POINT ( 'NONE',  ( -19.59569683186026268, 0.000000000000000000, 14.58168106541950948 ) ) ;
#923 = EDGE_CURVE ( 'NONE', #2679, #53048, #44027, .T. ) ;
#924 = FACE_OUTER_BOUND ( 'NONE', #49835, .T. ) ;
#925 = ORIENTED_EDGE ( 'NONE', *, *, #9121, .F. ) ;
#926 = ADVANCED_FACE ( 'NONE', ( #44865 ), #23006, .F. ) ;
#927 = CARTESIAN_POINT ( 'NONE',  ( -56.75000000000000711, 6.050000000000001599, 2.449489742783185875 ) ) ;
#928 = DIRECTION ( 'NONE',  ( -0.3620778797217457101, 0.000000000000000000, -0.9321478471874540261 ) ) ;
#929 = EDGE_CURVE ( 'NONE', #51848, #27227, #40328, .T. ) ;
#930 = CARTESIAN_POINT ( 'NONE',  ( -16.83345271725875136, -4.565544526780663581, 3.274341045371267800 ) ) ;
#931 = VERTEX_POINT ( 'NONE', #9101 ) ;
#932 = DIRECTION ( 'NONE',  ( 0.7660212471507180654, -0.6427876096865404731, 0.005961354470445141482 ) ) ;
#933 = ADVANCED_FACE ( 'NONE', ( #27544 ), #10224, .F. ) ;
#934 = ORIENTED_EDGE ( 'NONE', *, *, #4863, .T. ) ;
#935 = VECTOR ( 'NONE', #8845, 1000.000000000000000 ) ;
#936 = EDGE_LOOP ( 'NONE', ( #37602, #6068, #49001, #22421 ) ) ;
#937 = ORIENTED_EDGE ( 'NONE', *, *, #53272, .F. ) ;
#938 = ORIENTED_EDGE ( 'NONE', *, *, #25465, .T. ) ;
#939 = CARTESIAN_POINT ( 'NONE',  ( -12.33850799832341849, 0.000000000000000000, 11.68350162852954632 ) ) ;
#940 = VERTEX_POINT ( 'NONE', #22167 ) ;
#941 = PLANE ( 'NONE',  #37648 ) ;
#942 = LINE ( 'NONE', #19105, #39482 ) ;
#943 = ORIENTED_EDGE ( 'NONE', *, *, #31942, .T. ) ;
#944 = CARTESIAN_POINT ( 'NONE',  ( -10.27421835998572064, 0.000000000000000000, 10.96090226820206048 ) ) ;
#945 = ORIENTED_EDGE ( 'NONE', *, *, #16723, .T. ) ;
#946 = DIRECTION ( 'NONE',  ( 0.5449076811759707706, 0.6444004775717708799, -0.5364919789714476250 ) ) ;
#947 = VERTEX_POINT ( 'NONE', #48859 ) ;
#948 = PLANE ( 'NONE',  #54545 ) ;
#949 = CARTESIAN_POINT ( 'NONE',  ( -14.02258558381341658, -2.298917212465657833, 5.901694980474549546 ) ) ;
#950 = CARTESIAN_POINT ( 'NONE',  ( -26.13337879274045505, 0.000000000000000000, 6.833023547870798353 ) ) ;
#951 = FILL_AREA_STYLE_COLOUR ( '', #1196 ) ;
#952 = CARTESIAN_POINT ( 'NONE',  ( -11.60822677631003152, 0.000000000000000000, 3.252740941409099751 ) ) ;
#953 = DIRECTION ( 'NONE',  ( -0.7660212471507179544, -0.6427876096865405842, -0.005961354470445141482 ) ) ;
#954 = EDGE_LOOP ( 'NONE', ( #10869, #39100, #31754, #41856 ) ) ;
#955 = ADVANCED_FACE ( 'NONE', ( #36093 ), #49115, .F. ) ;
#956 = EDGE_LOOP ( 'NONE', ( #1313, #15938, #4938, #5565 ) ) ;
#957 = CARTESIAN_POINT ( 'NONE',  ( -2.730566055856384011, -5.007877867457373178, -2.157728989155597077 ) ) ;
#958 = DIRECTION ( 'NONE',  ( 0.9335804264972041855, -0.3583679495452941621, 0.000000000000000000 ) ) ;
#959 = EDGE_CURVE ( 'NONE', #15160, #32655, #19024, .T. ) ;
#960 = EDGE_CURVE ( 'NONE', #29871, #32511, #43730, .T. ) ;
#961 = LINE ( 'NONE', #48109, #12461 ) ;
#962 = CARTESIAN_POINT ( 'NONE',  ( -15.43942292826481477, 4.333955019861512881, 2.540852065959424255 ) ) ;
#963 = EDGE_LOOP ( 'NONE', ( #48660, #54179, #26989, #34399, #45764, #5188, #19645, #55104, #36476, #32181 ) ) ;
#964 = DIRECTION ( 'NONE',  ( 0.6427681459581294776, -0.7660444431189769032, 0.005002170337467562802 ) ) ;
#965 = DIRECTION ( 'NONE',  ( -0.9999697198139514409, -0.000000000000000000, -0.007781995580013368816 ) ) ;
#966 = ORIENTED_EDGE ( 'NONE', *, *, #16669, .T. ) ;
#967 = PLANE ( 'NONE',  #37478 ) ;
#968 = CARTESIAN_POINT ( 'NONE',  ( -21.06965149344186372, 20.49370688441071664, 4.356723378946029790 ) ) ;
#969 = EDGE_LOOP ( 'NONE', ( #47151, #36627, #20030, #10583 ) ) ;
#970 = CARTESIAN_POINT ( 'NONE',  ( -69.01437307246155228, -9.005354531669947704, 7.360527835276527320 ) ) ;
#971 = LINE ( 'NONE', #18595, #52330 ) ;
#972 = VECTOR ( 'NONE', #8034, 1000.000000000000000 ) ;
#973 = CARTESIAN_POINT ( 'NONE',  ( -11.30636317915456779, -0.1191753592594197858, 11.32220194836580340 ) ) ;
#974 = DIRECTION ( 'NONE',  ( 0.000000000000000000, 0.000000000000000000, 1.000000000000000000 ) ) ;
#975 = VECTOR ( 'NONE', #31233, 1000.000000000000227 ) ;
#976 = DIRECTION ( 'NONE',  ( 0.000000000000000000, -1.000000000000000000, 0.000000000000000000 ) ) ;
#977 = ORIENTED_EDGE ( 'NONE', *, *, #21951, .F. ) ;
#978 = ORIENTED_EDGE ( 'NONE', *, *, #32584, .T. ) ;
#979 = PLANE ( 'NONE',  #20299 ) ;
#980 = DIRECTION ( 'NONE',  ( 0.000000000000000000, -0.000000000000000000, -1.000000000000000000 ) ) ;
#981 = DIRECTION ( 'NONE',  ( 0.007781995580012663651, -3.146120232559066537E-19, -0.9999697198139514409 ) ) ;
#982 = DIRECTION ( 'NONE',  ( -0.005961354470445682716, -0.6427876096865404731, 0.7660212471507180654 ) ) ;
#983 = DIRECTION ( 'NONE',  ( 0.007781995580012663651, -3.146120232559066537E-19, -0.9999697198139514409 ) ) ;
#984 = ORIENTED_EDGE ( 'NONE', *, *, #52966, .F. ) ;
#985 = CARTESIAN_POINT ( 'NONE',  ( -16.14528680376529834, 23.33679016358333769, -3.961395337094443914 ) ) ;
#986 = LINE ( 'NONE', #1824, #42914 ) ;
#987 = CARTESIAN_POINT ( 'NONE',  ( -7.416723841188632704, 7.236484701362529748, 6.099280988583309693 ) ) ;
#988 = FACE_OUTER_BOUND ( 'NONE', #30286, .T. ) ;
#989 = ORIENTED_EDGE ( 'NONE', *, *, #52773, .F. ) ;
#990 = LINE ( 'NONE', #27405, #40172 ) ;
#991 = ORIENTED_EDGE ( 'NONE', *, *, #20362, .F. ) ;
#992 = CARTESIAN_POINT ( 'NONE',  ( -9.542064456761055524, 0.000000000000000000, 10.59726798936431180 ) ) ;
#993 = DIRECTION ( 'NONE',  ( 0.000000000000000000, -1.000000000000000000, 0.000000000000000000 ) ) ;
#994 = VERTEX_POINT ( 'NONE', #48574 ) ;
#995 = VECTOR ( 'NONE', #13081, 999.9999999999998863 ) ;
#996 = VECTOR ( 'NONE', #24156, 1000.000000000000000 ) ;
#997 = LINE ( 'NONE', #53534, #29938 ) ;
#998 = EDGE_CURVE ( 'NONE', #8255, #46454, #9688, .T. ) ;
#999 = ORIENTED_EDGE ( 'NONE', *, *, #22365, .T. ) ;
#1000 = ORIENTED_EDGE ( 'NONE', *, *, #40100, .F. ) ;
#1001 = ORIENTED_EDGE ( 'NONE', *, *, #101, .T. ) ;
#1002 = CARTESIAN_POINT ( 'NONE',  ( -16.53317331066696383, 0.000000000000000000, 13.31285208727739899 ) ) ;
#1003 = VERTEX_POINT ( 'NONE', #37450 ) ;
#1004 = VERTEX_POINT ( 'NONE', #19594 ) ;
#1005 = CARTESIAN_POINT ( 'NONE',  ( -13.70700505671111991, 0.000000000000000000, 8.407056740829760955 ) ) ;
#1006 = CARTESIAN_POINT ( 'NONE',  ( -11.74258550959773473, -2.946525016555661125, 1.348530534211536569 ) ) ;
#1007 = EDGE_LOOP ( 'NONE', ( #32540, #50590, #12185 ) ) ;
#1008 = EDGE_CURVE ( 'NONE', #16356, #25458, #53651, .T. ) ;
#1009 = CIRCLE ( 'NONE', #16413, 2.750000000000001776 ) ;
#1010 = ORIENTED_EDGE ( 'NONE', *, *, #51804, .T. ) ;
#1011 = PLANE ( 'NONE',  #21343 ) ;
#1012 = ORIENTED_EDGE ( 'NONE', *, *, #34768, .T. ) ;
#1013 = EDGE_CURVE ( 'NONE', #52907, #40102, #40881, .T. ) ;
#1014 = ORIENTED_EDGE ( 'NONE', *, *, #44687, .F. ) ;
#1015 = EDGE_CURVE ( 'NONE', #6174, #4939, #19857, .T. ) ;
#1016 = AXIS2_PLACEMENT_3D ( 'NONE', #11002, #28060, #6476 ) ;
#1017 = CARTESIAN_POINT ( 'NONE',  ( -14.01545677930355183, 0.000000000000000000, 2.126011111488108174 ) ) ;
#1018 = DIRECTION ( 'NONE',  ( 0.007781995580012662783, 0.000000000000000000, -0.9999697198139514409 ) ) ;
#1019 = DIRECTION ( 'NONE',  ( 0.9999697198139515519, 0.000000000000000000, 0.007781995580013368816 ) ) ;
#1020 = DIRECTION ( 'NONE',  ( 0.5449076811759707706, 0.6444004775717708799, -0.5364919789714476250 ) ) ;
#1021 = ADVANCED_FACE ( 'NONE', ( #54225 ), #6262, .F. ) ;
#1022 = EDGE_LOOP ( 'NONE', ( #31924, #11783, #54419, #4672 ) ) ;
#1023 = DIRECTION ( 'NONE',  ( -0.7660212471507179544, -0.6427876096865405842, -0.005961354470445141482 ) ) ;
#1024 = ORIENTED_EDGE ( 'NONE', *, *, #4151, .F. ) ;
#1025 = EDGE_CURVE ( 'NONE', #25299, #40139, #41984, .T. ) ;
#1026 = CARTESIAN_POINT ( 'NONE',  ( -24.26908309836554878, 0.000000000000000000, 6.108867788427308376 ) ) ;
#1027 = ADVANCED_FACE ( 'NONE', ( #28102 ), #46241, .F. ) ;
#1028 = CARTESIAN_POINT ( 'NONE',  ( -21.47263955680318404, 0.000000000000000000, 5.022634149262071190 ) ) ;
#1029 = CARTESIAN_POINT ( 'NONE',  ( -27.99923088623136636, 0.000000000000000000, 7.757173251277078130 ) ) ;
#1030 = CARTESIAN_POINT ( 'NONE',  ( -16.99924723426068951, 0.000000000000000000, 13.49389102713827171 ) ) ;
#1031 = CARTESIAN_POINT ( 'NONE',  ( 5.616557846695583223, -1.037130572669888506, -2.260114876317554700 ) ) ;
#1032 = DIRECTION ( 'NONE',  ( 0.9999697198139515519, 0.000000000000000000, 0.007781995580013368816 ) ) ;
#1033 = DIRECTION ( 'NONE',  ( 0.8531650599175529814, -0.4028455766673920135, -0.3313982828793697877 ) ) ;
#1034 = ORIENTED_EDGE ( 'NONE', *, *, #29741, .T. ) ;
#1035 = DIRECTION ( 'NONE',  ( -0.7660212471507179544, -0.6427876096865405842, -0.005961354470445141482 ) ) ;
#1036 = EDGE_CURVE ( 'NONE', #40968, #15460, #7347, .T. ) ;
#1037 = VECTOR ( 'NONE', #30828, 1000.000000000000227 ) ;
#1038 = VECTOR ( 'NONE', #2284, 1000.000000000000227 ) ;
#1039 = FACE_BOUND ( 'NONE', #10706, .T. ) ;
#1040 = PLANE ( 'NONE',  #55004 ) ;
#1041 = PLANE ( 'NONE',  #6322 ) ;
#1042 = CARTESIAN_POINT ( 'NONE',  ( -28.39101450145270178, 14.53466517333176533, -4.730044803147324117 ) ) ;
#1043 = PLANE ( 'NONE',  #11381 ) ;
#1044 = PLANE ( 'NONE',  #25022 ) ;
#1045 = EDGE_CURVE ( 'NONE', #53756, #29871, #2790, .T. ) ;
#1046 = DIRECTION ( 'NONE',  ( 0.007781995580012663651, 0.000000000000000000, -0.9999697198139515519 ) ) ;
#1047 = VECTOR ( 'NONE', #21180, 1000.000000000000114 ) ;
#1048 = ORIENTED_EDGE ( 'NONE', *, *, #6882, .T. ) ;
#1049 = CARTESIAN_POINT ( 'NONE',  ( 2.072287782118878319, 0.000000000000000000, -2.950529333540147015 ) ) ;
#1050 = CARTESIAN_POINT ( 'NONE',  ( -22.26155136248034694, 19.71499928042501537, 4.429874044484920503 ) ) ;
#1051 = DIRECTION ( 'NONE',  ( 0.9999697198139515519, 0.000000000000000000, 0.007781995580013368816 ) ) ;
#1052 = CARTESIAN_POINT ( 'NONE',  ( -15.45392365408441826, 1.581621852479004664, 2.634298478400116661 ) ) ;
#1053 = LINE ( 'NONE', #49050, #32156 ) ;
#1054 = DIRECTION ( 'NONE',  ( -0.6427681459581293666, -0.7660444431189770143, -0.005002170337467561935 ) ) ;
#1055 = DIRECTION ( 'NONE',  ( 0.9999697198139515519, 0.000000000000000000, 0.007781995580013368816 ) ) ;
#1056 = AXIS2_PLACEMENT_3D ( 'NONE', #46333, #7749, #45795 ) ;
#1057 = CARTESIAN_POINT ( 'NONE',  ( -10.42448858938141321, 0.000000000000000000, 4.569955331333209969 ) ) ;
#1058 = LINE ( 'NONE', #4508, #34692 ) ;
#1059 = ORIENTED_EDGE ( 'NONE', *, *, #9491, .T. ) ;
#1060 = EDGE_CURVE ( 'NONE', #52765, #2187, #54478, .T. ) ;
#1061 = ORIENTED_EDGE ( 'NONE', *, *, #28759, .T. ) ;
#1062 = ORIENTED_EDGE ( 'NONE', *, *, #16103, .T. ) ;
#1063 = ORIENTED_EDGE ( 'NONE', *, *, #52829, .T. ) ;
#1064 = ORIENTED_EDGE ( 'NONE', *, *, #44421, .T. ) ;
#1065 = DIRECTION ( 'NONE',  ( 0.000000000000000000, 0.000000000000000000, -1.000000000000000000 ) ) ;
#1066 = CARTESIAN_POINT ( 'NONE',  ( -22.40556560354864146, -0.1191753592594197858, 5.484709000965211523 ) ) ;
#1067 = EDGE_CURVE ( 'NONE', #38273, #21098, #53942, .T. ) ;
#1068 = AXIS2_PLACEMENT_3D ( 'NONE', #38433, #16875, #51514 ) ;
#1069 = VECTOR ( 'NONE', #18804, 999.9999999999998863 ) ;
#1070 = ORIENTED_EDGE ( 'NONE', *, *, #44192, .T. ) ;
#1071 = ORIENTED_EDGE ( 'NONE', *, *, #14890, .T. ) ;
#1072 = EDGE_CURVE ( 'NONE', #30915, #18980, #14765, .T. ) ;
#1073 = VECTOR ( 'NONE', #39471, 1000.000000000000227 ) ;
#1074 = CARTESIAN_POINT ( 'NONE',  ( -66.40205603077350816, -9.309201745752147872, -5.905017180569076096 ) ) ;
#1075 = ORIENTED_EDGE ( 'NONE', *, *, #36477, .T. ) ;
#1076 = PLANE ( 'NONE',  #9214 ) ;
#1077 = DIRECTION ( 'NONE',  ( 0.007781995580012663651, -3.146120232559066537E-19, -0.9999697198139514409 ) ) ;
#1078 = ORIENTED_EDGE ( 'NONE', *, *, #56058, .F. ) ;
#1079 = FACE_OUTER_BOUND ( 'NONE', #48733, .T. ) ;
#1080 = VERTEX_POINT ( 'NONE', #32094 ) ;
#1081 = CARTESIAN_POINT ( 'NONE',  ( -18.66354898467281132, 0.000000000000000000, 14.21960318569776582 ) ) ;
#1082 = ADVANCED_FACE ( 'NONE', ( #28673 ), #23565, .F. ) ;
#1083 = AXIS2_PLACEMENT_3D ( 'NONE', #36884, #36304, #24087 ) ;
#1084 = DIRECTION ( 'NONE',  ( -0.9999697198139514409, -0.000000000000000000, -0.007781995580013368816 ) ) ;
#1085 = EDGE_CURVE ( 'NONE', #36106, #20635, #41457, .T. ) ;
#1086 = CARTESIAN_POINT ( 'NONE',  ( -10.66613911421745264, 0.000000000000000000, 1.613418192619087588 ) ) ;
#1087 = PLANE ( 'NONE',  #45093 ) ;
#1088 = ORIENTED_EDGE ( 'NONE', *, *, #55992, .F. ) ;
#1089 = CARTESIAN_POINT ( 'NONE',  ( -14.65381140700083229, -1.975113310420658852, 2.510342657734869753 ) ) ;
#1090 = CARTESIAN_POINT ( 'NONE',  ( -19.45503627000849889, -1.000000000000000000, 7.556996783084074742 ) ) ;
#1091 = CARTESIAN_POINT ( 'NONE',  ( -27.06708303904391144, 0.000000000000000000, 7.395095371555332697 ) ) ;
#1092 = EDGE_LOOP ( 'NONE', ( #33982, #22318, #12217, #35445 ) ) ;
#1093 = LINE ( 'NONE', #23536, #39186 ) ;
#1094 = ORIENTED_EDGE ( 'NONE', *, *, #34768, .F. ) ;
#1095 = EDGE_CURVE ( 'NONE', #28751, #18842, #32389, .T. ) ;
#1096 = LINE ( 'NONE', #39754, #2894 ) ;
#1097 = CARTESIAN_POINT ( 'NONE',  ( -19.60990026154428278, 0.000000000000000000, 4.498472333781370125 ) ) ;
#1098 = PLANE ( 'NONE',  #40317 ) ;
#1099 = DIRECTION ( 'NONE',  ( 0.6427681459581294776, -0.7660444431189769032, 0.005002170337467562802 ) ) ;
#1100 = AXIS2_PLACEMENT_3D ( 'NONE', #1492, #4626, #4911 ) ;
#1101 = DIRECTION ( 'NONE',  ( -0.005002170337468016433, -0.7660444431189770143, 0.6427681459581293666 ) ) ;
#1102 = FACE_OUTER_BOUND ( 'NONE', #19728, .T. ) ;
#1103 = CARTESIAN_POINT ( 'NONE',  ( -9.847580306979804021, -0.1191753592594190225, 2.997113657646766516 ) ) ;
#1104 = EDGE_CURVE ( 'NONE', #32862, #27005, #10793, .T. ) ;
#1105 = PLANE ( 'NONE',  #11081 ) ;
#1106 = SURFACE_STYLE_FILL_AREA ( #18752 ) ;
#1107 = LINE ( 'NONE', #22455, #28687 ) ;
#1108 = ORIENTED_EDGE ( 'NONE', *, *, #24121, .F. ) ;
#1109 = VECTOR ( 'NONE', #22249, 1000.000000000000227 ) ;
#1110 = CARTESIAN_POINT ( 'NONE',  ( -17.18961764541363024, 0.000000000000000000, 3.947969406708516704 ) ) ;
#1111 = PLANE ( 'NONE',  #28547 ) ;
#1112 = CARTESIAN_POINT ( 'NONE',  ( -19.97424332634331989, -1.651309408375658760, 4.587310137610792538 ) ) ;
#1113 = CARTESIAN_POINT ( 'NONE',  ( -22.40556560354864146, -0.1191753592594197858, 5.484709000965211523 ) ) ;
#1114 = VECTOR ( 'NONE', #14489, 1000.000000000000227 ) ;
#1115 = VECTOR ( 'NONE', #5387, 999.9999999999998863 ) ;
#1116 = LINE ( 'NONE', #25872, #47246 ) ;
#1117 = PLANE ( 'NONE',  #16062 ) ;
#1118 = DIRECTION ( 'NONE',  ( 0.6427681459581294776, -0.7660444431189769032, 0.005002170337467562802 ) ) ;
#1119 = VERTEX_POINT ( 'NONE', #15325 ) ;
#1120 = VECTOR ( 'NONE', #5356, 999.9999999999998863 ) ;
#1121 = VECTOR ( 'NONE', #32886, 1000.000000000000227 ) ;
#1122 = ORIENTED_EDGE ( 'NONE', *, *, #48950, .T. ) ;
#1123 = FACE_OUTER_BOUND ( 'NONE', #15703, .T. ) ;
#1124 = PLANE ( 'NONE',  #9605 ) ;
#1125 = EDGE_LOOP ( 'NONE', ( #11524, #5118, #3400, #21702 ) ) ;
#1126 = PLANE ( 'NONE',  #50338 ) ;
#1127 = ADVANCED_FACE ( 'NONE', ( #41701 ), #45409, .F. ) ;
#1128 = VERTEX_POINT ( 'NONE', #11045 ) ;
#1129 = LINE ( 'NONE', #31252, #252 ) ;
#1130 = EDGE_LOOP ( 'NONE', ( #36116, #1815, #51661, #8244 ) ) ;
#1131 = VERTEX_POINT ( 'NONE', #28370 ) ;
#1132 = EDGE_CURVE ( 'NONE', #3861, #40733, #6809, .T. ) ;
#1133 = ORIENTED_EDGE ( 'NONE', *, *, #12182, .F. ) ;
#1134 = EDGE_CURVE ( 'NONE', #21716, #44513, #51470, .T. ) ;
#1135 = LINE ( 'NONE', #22480, #12068 ) ;
#1136 = DIRECTION ( 'NONE',  ( 0.7660212471507180654, -0.6427876096865404731, 0.005961354470445141482 ) ) ;
#1137 = PLANE ( 'NONE',  #47499 ) ;
#1138 = ADVANCED_FACE ( 'NONE', ( #33850 ), #50875, .F. ) ;
#1139 = ADVANCED_FACE ( 'NONE', ( #33566 ), #7742, .F. ) ;
#1140 = EDGE_CURVE ( 'NONE', #29285, #27679, #8026, .T. ) ;
#1141 = DIRECTION ( 'NONE',  ( -0.7660212471507179544, -0.6427876096865405842, -0.005961354470445141482 ) ) ;
#1142 = ORIENTED_EDGE ( 'NONE', *, *, #25881, .F. ) ;
#1143 = ORIENTED_EDGE ( 'NONE', *, *, #9429, .T. ) ;
#1144 = VECTOR ( 'NONE', #22161, 999.9999999999998863 ) ;
#1145 = CARTESIAN_POINT ( 'NONE',  ( -17.80222495869421451, -1.813211359398156919, 6.572709218920322449 ) ) ;
#1146 = ORIENTED_EDGE ( 'NONE', *, *, #41593, .F. ) ;
#1147 = VECTOR ( 'NONE', #55689, 1000.000000000000114 ) ;
#1148 = CARTESIAN_POINT ( 'NONE',  ( -17.74404816805336793, 0.000000000000000000, 3.574322630375089460 ) ) ;
#1149 = EDGE_LOOP ( 'NONE', ( #52643, #9477, #12356, #26488 ) ) ;
#1150 = DIRECTION ( 'NONE',  ( 0.9999697198139515519, 0.000000000000000000, 0.007781995580013368816 ) ) ;
#1151 = FACE_OUTER_BOUND ( 'NONE', #44393, .T. ) ;
#1152 = VECTOR ( 'NONE', #35541, 1000.000000000000227 ) ;
#1153 = AXIS2_PLACEMENT_3D ( 'NONE', #22380, #1035, #40542 ) ;
#1154 = VERTEX_POINT ( 'NONE', #25339 ) ;
#1155 = CARTESIAN_POINT ( 'NONE',  ( -14.93495759592298988, 0.000000000000000000, 12.77129166681078409 ) ) ;
#1156 = EDGE_CURVE ( 'NONE', #29456, #32397, #8288, .T. ) ;
#1157 = ORIENTED_EDGE ( 'NONE', *, *, #53864, .F. ) ;
#1158 = EDGE_CURVE ( 'NONE', #34260, #18621, #47181, .T. ) ;
#1159 = VECTOR ( 'NONE', #7810, 1000.000000000000114 ) ;
#1160 = DIRECTION ( 'NONE',  ( 0.5364919789714477361, 0.6444004775717706579, 0.5449076811759711036 ) ) ;
#1161 = AXIS2_PLACEMENT_3D ( 'NONE', #8248, #51124, #25562 ) ;
#1162 = ORIENTED_EDGE ( 'NONE', *, *, #48359, .F. ) ;
#1163 = PLANE ( 'NONE',  #31379 ) ;
#1164 = DIRECTION ( 'NONE',  ( 0.9999697198139515519, 0.000000000000000000, 0.007781995580013368816 ) ) ;
#1165 = EDGE_CURVE ( 'NONE', #13096, #1131, #46626, .T. ) ;
#1166 = DIRECTION ( 'NONE',  ( 0.007781995580012662783, 0.000000000000000000, -0.9999697198139514409 ) ) ;
#1167 = VERTEX_POINT ( 'NONE', #38105 ) ;
#1168 = ADVANCED_FACE ( 'NONE', ( #51169 ), #12282, .F. ) ;
#1169 = CARTESIAN_POINT ( 'NONE',  ( -14.67804947269237203, -1.975113310420657520, 5.624882046661574542 ) ) ;
#1170 = DIRECTION ( 'NONE',  ( 0.000000000000000000, -0.000000000000000000, -1.000000000000000000 ) ) ;
#1171 = AXIS2_PLACEMENT_3D ( 'NONE', #24094, #11305, #41422 ) ;
#1172 = FACE_OUTER_BOUND ( 'NONE', #56171, .T. ) ;
#1173 = VECTOR ( 'NONE', #47615, 1000.000000000000227 ) ;
#1174 = DIRECTION ( 'NONE',  ( -0.6427681459581293666, -0.7660444431189770143, -0.005002170337467561935 ) ) ;
#1175 = CARTESIAN_POINT ( 'NONE',  ( -9.394439624159845792, -0.1191753592594179401, 4.477968382445831175 ) ) ;
#1176 = ORIENTED_EDGE ( 'NONE', *, *, #5629, .F. ) ;
#1177 = DIRECTION ( 'NONE',  ( 0.007781995580012662783, 0.000000000000000000, -0.9999697198139514409 ) ) ;
#1178 = FACE_OUTER_BOUND ( 'NONE', #8509, .T. ) ;
#1179 = CARTESIAN_POINT ( 'NONE',  ( -18.67619601524082285, 0.000000000000000000, 3.936400510096834893 ) ) ;
#1180 = ORIENTED_EDGE ( 'NONE', *, *, #37039, .T. ) ;
#1181 = PLANE ( 'NONE',  #2092 ) ;
#1182 = FACE_OUTER_BOUND ( 'NONE', #21499, .T. ) ;
#1183 = ORIENTED_EDGE ( 'NONE', *, *, #22124, .F. ) ;
#1184 = AXIS2_PLACEMENT_3D ( 'NONE', #26250, #51542, #51252 ) ;
#1185 = DIRECTION ( 'NONE',  ( -0.7660212471507179544, -0.6427876096865405842, -0.005961354470445141482 ) ) ;
#1186 = CARTESIAN_POINT ( 'NONE',  ( -15.60102546347950536, 0.000000000000000000, 12.95077420755565356 ) ) ;
#1187 = AXIS2_PLACEMENT_3D ( 'NONE', #30707, #43214, #21625 ) ;
#1188 = LINE ( 'NONE', #18521, #5171 ) ;
#1189 = DIRECTION ( 'NONE',  ( 0.5364919789714477361, 0.6444004775717706579, 0.5449076811759711036 ) ) ;
#1190 = EDGE_LOOP ( 'NONE', ( #52515, #25889, #24218, #32180 ) ) ;
#1191 = EDGE_LOOP ( 'NONE', ( #4345, #38872, #49783 ) ) ;
#1192 = DIRECTION ( 'NONE',  ( -0.6427681459581293666, -0.7660444431189770143, -0.005002170337467561935 ) ) ;
#1193 = PLANE ( 'NONE',  #17787 ) ;
#1194 = VECTOR ( 'NONE', #24398, 1000.000000000000227 ) ;
#1195 = CARTESIAN_POINT ( 'NONE',  ( -13.58191980274018462, -0.1191753592594188005, 5.184044583049274735 ) ) ;
#1196 = COLOUR_RGB ( '', 0.40784314, 0.44705882, 0.49803922) ;
#1197 = FACE_OUTER_BOUND ( 'NONE', #37198, .T. ) ;
#1198 = AXIS2_PLACEMENT_3D ( 'NONE', #51681, #25861, #30690 ) ;
#1199 = CARTESIAN_POINT ( 'NONE',  ( -14.94760462649100496, 0.000000000000000000, 2.488088991209854051 ) ) ;
#1200 = CARTESIAN_POINT ( 'NONE',  ( -20.26688789326949092, -0.6003329984493698257, 5.466933331983609534 ) ) ;
#1201 = VERTEX_POINT ( 'NONE', #43241 ) ;
#1202 = CARTESIAN_POINT ( 'NONE',  ( -15.03495456790438389, -0.1191753592594197858, 12.77051346725278158 ) ) ;
#1203 = VECTOR ( 'NONE', #49764, 1000.000000000000227 ) ;
#1204 = DIRECTION ( 'NONE',  ( 0.005961354470445682716, -0.6427876096865404731, -0.7660212471507180654 ) ) ;
#1205 = AXIS2_PLACEMENT_3D ( 'NONE', #21549, #51628, #34880 ) ;
#1206 = ORIENTED_EDGE ( 'NONE', *, *, #7060, .F. ) ;
#1207 = DIRECTION ( 'NONE',  ( -0.7660212471507179544, -0.6427876096865405842, -0.005961354470445141482 ) ) ;
#1208 = FACE_OUTER_BOUND ( 'NONE', #45868, .T. ) ;
#1209 = DIRECTION ( 'NONE',  ( 0.6427681459581294776, -0.7660444431189769032, 0.005002170337467562802 ) ) ;
#1210 = EDGE_CURVE ( 'NONE', #11984, #43814, #42642, .T. ) ;
#1211 = ADVANCED_FACE ( 'NONE', ( #21362 ), #55420, .F. ) ;
#1212 = ORIENTED_EDGE ( 'NONE', *, *, #28692, .F. ) ;
#1213 = CARTESIAN_POINT ( 'NONE',  ( -10.42580624377069398, 0.000000000000000000, 4.739271090628184524 ) ) ;
#1214 = ORIENTED_EDGE ( 'NONE', *, *, #17604, .T. ) ;
#1215 = ADVANCED_FACE ( 'NONE', ( #55710 ), #42932, .F. ) ;
#1216 = ORIENTED_EDGE ( 'NONE', *, *, #54700, .F. ) ;
#1217 = ORIENTED_EDGE ( 'NONE', *, *, #5235, .F. ) ;
#1218 = ORIENTED_EDGE ( 'NONE', *, *, #16405, .T. ) ;
#1219 = DIRECTION ( 'NONE',  ( 0.000000000000000000, -1.000000000000000000, 0.000000000000000000 ) ) ;
#1220 = VERTEX_POINT ( 'NONE', #4337 ) ;
#1221 = VECTOR ( 'NONE', #37144, 1000.000000000000114 ) ;
#1222 = CARTESIAN_POINT ( 'NONE',  ( -20.26176469941677993, 0.000000000000000000, 14.76116360616437895 ) ) ;
#1223 = LINE ( 'NONE', #56140, #49492 ) ;
#1224 = VERTEX_POINT ( 'NONE', #34158 ) ;
#1225 = CARTESIAN_POINT ( 'NONE',  ( -11.15796014699535910, 0.000000000000000000, 5.102905369465933205 ) ) ;
#1226 = ORIENTED_EDGE ( 'NONE', *, *, #53223, .T. ) ;
#1227 = CARTESIAN_POINT ( 'NONE',  ( -31.72782227498118601, 0.000000000000000000, 9.205484770164058972 ) ) ;
#1228 = VECTOR ( 'NONE', #3408, 999.9999999999998863 ) ;
#1229 = ORIENTED_EDGE ( 'NONE', *, *, #9897, .F. ) ;
#1230 = EDGE_CURVE ( 'NONE', #31801, #20518, #12566, .T. ) ;
#1231 = CARTESIAN_POINT ( 'NONE',  ( -17.93139508144814442, 0.000000000000000000, 13.85596890686001537 ) ) ;
#1232 = PLANE ( 'NONE',  #41080 ) ;
#1233 = DIRECTION ( 'NONE',  ( 0.6427681459581294776, -0.7660444431189769032, 0.005002170337467562802 ) ) ;
#1234 = CYLINDRICAL_SURFACE ( 'NONE', #12104, 0.7500000000000006661 ) ;
#1235 = EDGE_CURVE ( 'NONE', #37629, #10857, #21649, .T. ) ;
#1236 = FACE_OUTER_BOUND ( 'NONE', #19862, .T. ) ;
#1237 = AXIS2_PLACEMENT_3D ( 'NONE', #54105, #41025, #45852 ) ;
#1238 = LINE ( 'NONE', #10643, #55534 ) ;
#1239 = ORIENTED_EDGE ( 'NONE', *, *, #43794, .T. ) ;
#1240 = VECTOR ( 'NONE', #9345, 1000.000000000000000 ) ;
#1242 = EDGE_LOOP ( 'NONE', ( #33007, #29909, #54777, #5167 ) ) ;
#1241 = EDGE_CURVE ( 'NONE', #8596, #49849, #12831, .T. ) ;
#1243 = CARTESIAN_POINT ( 'NONE',  ( -17.75217832828985820, -0.1191753592594190225, 3.677175353557638360 ) ) ;
#1244 = CARTESIAN_POINT ( 'NONE',  ( -13.27065584551087163, 0.000000000000000000, 12.04557950825129176 ) ) ;
#1245 = ADVANCED_FACE ( 'NONE', ( #26 ), #17357, .F. ) ;
#1246 = DIRECTION ( 'NONE',  ( 0.005002170337468016433, -0.7660444431189770143, -0.6427681459581293666 ) ) ;
#1247 = AXIS2_PLACEMENT_3D ( 'NONE', #53931, #1951, #32382 ) ;
#1248 = VECTOR ( 'NONE', #31091, 999.9999999999998863 ) ;
#1249 = CARTESIAN_POINT ( 'NONE',  ( -24.26908309836554878, 0.000000000000000000, 6.108867788427308376 ) ) ;
#1250 = EDGE_LOOP ( 'NONE', ( #46634, #5454, #20723, #15875 ) ) ;
#1251 = CARTESIAN_POINT ( 'NONE',  ( -11.20636620717317378, 0.000000000000000000, 11.32298014792380414 ) ) ;
#1252 = CARTESIAN_POINT ( 'NONE',  ( -14.49107522188537800, -0.1191753592594191197, 2.591644836708906663 ) ) ;
#1253 = ORIENTED_EDGE ( 'NONE', *, *, #34974, .T. ) ;
#1254 = DIRECTION ( 'NONE',  ( 0.9659258262890682012, -0.2588190451025213501, 0.000000000000000000 ) ) ;
#1255 = CARTESIAN_POINT ( 'NONE',  ( -8.975993561185934055, -0.1191753592594197858, 10.41700724906143982 ) ) ;
#1256 = VERTEX_POINT ( 'NONE', #4590 ) ;
#1257 = DIRECTION ( 'NONE',  ( 0.9999697198139515519, 0.000000000000000000, 0.007781995580013368816 ) ) ;
#1258 = CARTESIAN_POINT ( 'NONE',  ( -19.60990026154428278, 0.000000000000000000, 4.498472333781370125 ) ) ;
#1259 = PLANE ( 'NONE',  #49497 ) ;
#1260 = DIRECTION ( 'NONE',  ( -0.6427681459581293666, -0.7660444431189770143, -0.005002170337467561935 ) ) ;
#1261 = CARTESIAN_POINT ( 'NONE',  ( -9.867698681516781534, -0.1191753592594181482, 5.582281580451115666 ) ) ;
#1262 = EDGE_LOOP ( 'NONE', ( #22416, #28896, #47549, #43417 ) ) ;
#1263 = VECTOR ( 'NONE', #44655, 1000.000000000000227 ) ;
#1264 = ORIENTED_EDGE ( 'NONE', *, *, #30729, .T. ) ;
#1265 = CARTESIAN_POINT ( 'NONE',  ( -15.13495153988577968, 0.000000000000000000, 12.76973526769478084 ) ) ;
#1266 = FACE_OUTER_BOUND ( 'NONE', #11393, .T. ) ;
#1267 = LINE ( 'NONE', #22855, #52369 ) ;
#1268 = AXIS2_PLACEMENT_3D ( 'NONE', #28854, #37644, #54973 ) ;
#1269 = DIRECTION ( 'NONE',  ( 0.7660212471507180654, -0.6427876096865404731, 0.005961354470445141482 ) ) ;
#1270 = CARTESIAN_POINT ( 'NONE',  ( -16.79925329029790149, 0.000000000000000000, 13.49544742625427496 ) ) ;
#1271 = VECTOR ( 'NONE', #54648, 999.9999999999998863 ) ;
#1272 = ORIENTED_EDGE ( 'NONE', *, *, #50044, .F. ) ;
#1273 = FACE_OUTER_BOUND ( 'NONE', #23658, .T. ) ;
#1274 = CARTESIAN_POINT ( 'NONE',  ( -14.59739752808399693, -5.698858183938163791, 11.70485382328475765 ) ) ;
#1275 = DIRECTION ( 'NONE',  ( 0.9999697198139515519, 0.000000000000000000, 0.007781995580013368816 ) ) ;
#1276 = CARTESIAN_POINT ( 'NONE',  ( -18.48268442577178661, -3.756034771668162797, 3.940786248539256853 ) ) ;
#1277 = ORIENTED_EDGE ( 'NONE', *, *, #6006, .F. ) ;
#1278 = AXIS2_PLACEMENT_3D ( 'NONE', #55144, #50605, #11698 ) ;
#1279 = DIRECTION ( 'NONE',  ( 0.6427681459581294776, -0.7660444431189769032, 0.005002170337467562802 ) ) ;
#1280 = EDGE_LOOP ( 'NONE', ( #46976, #26824, #5714, #7174 ) ) ;
#1281 = DIRECTION ( 'NONE',  ( 0.007781995580012662783, 0.000000000000000000, -0.9999697198139514409 ) ) ;
#1282 = FACE_OUTER_BOUND ( 'NONE', #16307, .T. ) ;
#1283 = VECTOR ( 'NONE', #40595, 999.9999999999998863 ) ;
#1284 = ADVANCED_FACE ( 'NONE', ( #1151 ), #13661, .F. ) ;
#1285 = ORIENTED_EDGE ( 'NONE', *, *, #18893, .T. ) ;
#1286 = CARTESIAN_POINT ( 'NONE',  ( -10.21431608578677519, 0.000000000000000000, 3.263588676713128578 ) ) ;
#1287 = VERTEX_POINT ( 'NONE', #44333 ) ;
#1288 = EDGE_CURVE ( 'NONE', #9606, #17353, #317, .T. ) ;
#1289 = EDGE_CURVE ( 'NONE', #42137, #2279, #22746, .T. ) ;
#1290 = VECTOR ( 'NONE', #5907, 1000.000000000000114 ) ;
#1291 = EDGE_LOOP ( 'NONE', ( #10494, #29693, #27691, #54552 ) ) ;
#1292 = VERTEX_POINT ( 'NONE', #35527 ) ;
#1293 = CARTESIAN_POINT ( 'NONE',  ( -18.02080248396530848, 3.524445264749011208, 3.569375148849157853 ) ) ;
#1294 = VECTOR ( 'NONE', #21814, 1000.000000000000227 ) ;
#1295 = ORIENTED_EDGE ( 'NONE', *, *, #24887, .F. ) ;
#1296 = ORIENTED_EDGE ( 'NONE', *, *, #16534, .F. ) ;
#1297 = CARTESIAN_POINT ( 'NONE',  ( -5.829680373272994487, -7.699177326359582629, 5.482819409421843204 ) ) ;
#1298 = LINE ( 'NONE', #9849, #30364 ) ;
#1299 = ORIENTED_EDGE ( 'NONE', *, *, #8340, .T. ) ;
#1300 = VERTEX_POINT ( 'NONE', #31572 ) ;
#1301 = CARTESIAN_POINT ( 'NONE',  ( -15.36136699221811064, 0.000000000000000000, 7.855524030320988338 ) ) ;
#1302 = ORIENTED_EDGE ( 'NONE', *, *, #43624, .T. ) ;
#1303 = ORIENTED_EDGE ( 'NONE', *, *, #54137, .T. ) ;
#1304 = AXIS2_PLACEMENT_3D ( 'NONE', #45579, #12056, #50690 ) ;
#1305 = DIRECTION ( 'NONE',  ( -0.5364919789714478471, 0.6444004775717705469, -0.5449076811759709926 ) ) ;
#1306 = VECTOR ( 'NONE', #56012, 1000.000000000000227 ) ;
#1307 = LINE ( 'NONE', #53002, #19425 ) ;
#1308 = CARTESIAN_POINT ( 'NONE',  ( -16.77606153933838229, -5.051250379848164052, 3.236551803192220245 ) ) ;
#1309 = DIRECTION ( 'NONE',  ( -0.5449076811759708816, 0.6444004775717707689, 0.5364919789714475140 ) ) ;
#1310 = ORIENTED_EDGE ( 'NONE', *, *, #55422, .T. ) ;
#1311 = LINE ( 'NONE', #54384, #47388 ) ;
#1312 = AXIS2_PLACEMENT_3D ( 'NONE', #4287, #55657, #30394 ) ;
#1313 = ORIENTED_EDGE ( 'NONE', *, *, #45290, .F. ) ;
#1314 = PLANE ( 'NONE',  #36669 ) ;
#1315 = ADVANCED_FACE ( 'NONE', ( #14515 ), #5437, .F. ) ;
#1316 = DIRECTION ( 'NONE',  ( 0.9999697198139515519, 0.000000000000000000, 0.007781995580013368816 ) ) ;
#1317 = VECTOR ( 'NONE', #25702, 999.9999999999998863 ) ;
#1318 = CARTESIAN_POINT ( 'NONE',  ( -12.00514593104556305, -3.756034771668160577, 7.509431062354686937 ) ) ;
#1319 = LINE ( 'NONE', #30867, #45881 ) ;
#1320 = EDGE_CURVE ( 'NONE', #15806, #5087, #40357, .T. ) ;
#1321 = LINE ( 'NONE', #53841, #36634 ) ;
#1322 = AXIS2_PLACEMENT_3D ( 'NONE', #44807, #9906, #32032 ) ;
#1323 = CARTESIAN_POINT ( 'NONE',  ( -15.03495456790438389, -0.1191753592594197858, 12.77051346725278158 ) ) ;
#1324 = ORIENTED_EDGE ( 'NONE', *, *, #35734, .T. ) ;
#1325 = CARTESIAN_POINT ( 'NONE',  ( -13.86208312349174854, 1.905425754524006532, 2.005642517411173831 ) ) ;
#1326 = EDGE_CURVE ( 'NONE', #22884, #34361, #1455, .T. ) ;
#1327 = VERTEX_POINT ( 'NONE', #6014 ) ;
#1328 = AXIS2_PLACEMENT_3D ( 'NONE', #55885, #8446, #34562 ) ;
#1329 = FACE_OUTER_BOUND ( 'NONE', #32283, .T. ) ;
#1330 = CARTESIAN_POINT ( 'NONE',  ( -24.92324194630820244, 18.23204470015658174, -4.564397236248976419 ) ) ;
#1331 = PLANE ( 'NONE',  #55336 ) ;
#1332 = ADVANCED_FACE ( 'NONE', ( #52836 ), #48293, .F. ) ;
#1333 = PLANE ( 'NONE',  #14999 ) ;
#1334 = CARTESIAN_POINT ( 'NONE',  ( -25.20278734466900517, 0.000000000000000000, 6.670939612111840944 ) ) ;
#1335 = VECTOR ( 'NONE', #36218, 1000.000000000000114 ) ;
#1336 = CARTESIAN_POINT ( 'NONE',  ( -68.94855334729879814, -2.681968279941893282E-15, -7.664179260766972313 ) ) ;
#1337 = VECTOR ( 'NONE', #51375, 999.9999999999998863 ) ;
#1338 = ORIENTED_EDGE ( 'NONE', *, *, #28103, .T. ) ;
#1339 = CARTESIAN_POINT ( 'NONE',  ( -2.056461029976381472, 6.659969651376628441, 4.017172877417169552 ) ) ;
#1340 = LINE ( 'NONE', #54159, #41235 ) ;
#1341 = CARTESIAN_POINT ( 'NONE',  ( -18.67775241435682432, 0.000000000000000000, 4.136394454059623804 ) ) ;
#1342 = DIRECTION ( 'NONE',  ( 0.005002170337468016433, -0.7660444431189770143, -0.6427681459581293666 ) ) ;
#1343 = DIRECTION ( 'NONE',  ( 0.007781995580012663651, 0.000000000000000000, -0.9999697198139515519 ) ) ;
#1344 = CARTESIAN_POINT ( 'NONE',  ( -21.88142947281899708, -3.917936722690662066, 5.255808726792642105 ) ) ;
#1345 = EDGE_CURVE ( 'NONE', #55101, #40102, #9409, .T. ) ;
#1346 = DIRECTION ( 'NONE',  ( 0.005961354470445682716, -0.6427876096865404731, -0.7660212471507180654 ) ) ;
#1347 = VECTOR ( 'NONE', #7334, 1000.000000000000227 ) ;
#1348 = DIRECTION ( 'NONE',  ( -0.005961354470445682716, -0.6427876096865404731, 0.7660212471507180654 ) ) ;
#1349 = VECTOR ( 'NONE', #22887, 1000.000000000000227 ) ;
#1350 = CARTESIAN_POINT ( 'NONE',  ( -14.60466426183518607, 0.000000000000000000, 4.337418181458335020 ) ) ;
#1351 = ADVANCED_FACE ( 'NONE', ( #9975 ), #36114, .F. ) ;
#1352 = AXIS2_PLACEMENT_3D ( 'NONE', #55815, #35355, #22001 ) ;
#1353 = VERTEX_POINT ( 'NONE', #53417 ) ;
#1354 = ADVANCED_FACE ( 'NONE', ( #9716 ), #13947, .F. ) ;
#1355 = VECTOR ( 'NONE', #9417, 1000.000000000000114 ) ;
#1356 = EDGE_CURVE ( 'NONE', #43988, #8731, #22491, .T. ) ;
#1357 = ADVANCED_FACE ( 'NONE', ( #52312 ), #31828, .F. ) ;
#1358 = VERTEX_POINT ( 'NONE', #48600 ) ;
#1359 = EDGE_LOOP ( 'NONE', ( #10415, #15887, #48999, #40635 ) ) ;
#1360 = VECTOR ( 'NONE', #27646, 1000.000000000000000 ) ;
#1361 = VECTOR ( 'NONE', #49736, 999.9999999999998863 ) ;
#1362 = ORIENTED_EDGE ( 'NONE', *, *, #53870, .F. ) ;
#1363 = AXIS2_PLACEMENT_3D ( 'NONE', #48257, #22158, #39494 ) ;
#1364 = ORIENTED_EDGE ( 'NONE', *, *, #36334, .T. ) ;
#1365 = PLANE ( 'NONE',  #48657 ) ;
#1366 = CARTESIAN_POINT ( 'NONE',  ( -14.60622066095118576, 0.000000000000000000, 4.537412125421123932 ) ) ;
#1367 = VECTOR ( 'NONE', #37803, 1000.000000000000227 ) ;
#1368 = ORIENTED_EDGE ( 'NONE', *, *, #8155, .F. ) ;
#1369 = VERTEX_POINT ( 'NONE', #34996 ) ;
#1370 = EDGE_LOOP ( 'NONE', ( #41531, #53817 ) ) ;
#1371 = EDGE_CURVE ( 'NONE', #27421, #2828, #623, .T. ) ;
#1372 = VECTOR ( 'NONE', #49413, 1000.000000000000227 ) ;
#1373 = VECTOR ( 'NONE', #51812, 999.9999999999998863 ) ;
#1374 = CARTESIAN_POINT ( 'NONE',  ( -9.033451952363439119, 0.000000000000000000, 4.950112769895002707 ) ) ;
#1375 = CARTESIAN_POINT ( 'NONE',  ( -18.31855849401743086, 0.000000000000000000, 3.897176644277617896 ) ) ;
#1376 = DIRECTION ( 'NONE',  ( 0.005961354470445682716, -0.6427876096865404731, -0.7660212471507180654 ) ) ;
#1377 = ORIENTED_EDGE ( 'NONE', *, *, #26173, .T. ) ;
#1378 = LINE ( 'NONE', #4800, #8362 ) ;
#1379 = ORIENTED_EDGE ( 'NONE', *, *, #1008, .F. ) ;
#1380 = DIRECTION ( 'NONE',  ( 0.7660212471507180654, -0.6427876096865404731, 0.005961354470445141482 ) ) ;
#1381 = DIRECTION ( 'NONE',  ( 0.9321478471874540261, 0.000000000000000000, -0.3620778797217456546 ) ) ;
#1382 = AXIS2_PLACEMENT_3D ( 'NONE', #22527, #31018, #9452 ) ;
#1383 = CARTESIAN_POINT ( 'NONE',  ( -12.33850799832341849, 0.000000000000000000, 11.68350162852954632 ) ) ;
#1384 = LINE ( 'NONE', #9925, #1544 ) ;
#1385 = LINE ( 'NONE', #14460, #45774 ) ;
#1386 = DIRECTION ( 'NONE',  ( 0.9999697198139515519, 0.000000000000000000, 0.007781995580013368816 ) ) ;
#1388 = VECTOR ( 'NONE', #53123, 999.9999999999998863 ) ;
#1387 = CARTESIAN_POINT ( 'NONE',  ( -13.07066190154808361, 0.000000000000000000, 12.04713590736729678 ) ) ;
#1389 = ORIENTED_EDGE ( 'NONE', *, *, #17850, .T. ) ;
#1390 = DIRECTION ( 'NONE',  ( 0.9999697198139515519, 0.000000000000000000, 0.007781995580013368816 ) ) ;
#1391 = ORIENTED_EDGE ( 'NONE', *, *, #47578, .T. ) ;
#1392 = VECTOR ( 'NONE', #54145, 999.9999999999998863 ) ;
#1393 = PLANE ( 'NONE',  #27403 ) ;
#1394 = LINE ( 'NONE', #31785, #45045 ) ;
#1395 = LINE ( 'NONE', #27519, #14987 ) ;
#1396 = DIRECTION ( 'NONE',  ( -0.005002170337468016433, -0.7660444431189770143, 0.6427681459581293666 ) ) ;
#1397 = ADVANCED_FACE ( 'NONE', ( #10249 ), #27572, .F. ) ;
#1398 = VECTOR ( 'NONE', #29174, 999.9999999999998863 ) ;
#1399 = CARTESIAN_POINT ( 'NONE',  ( -17.46532115785441519, 0.000000000000000000, 13.67492996699914265 ) ) ;
#1400 = PLANE ( 'NONE',  #3189 ) ;
#1401 = FACE_OUTER_BOUND ( 'NONE', #53127, .T. ) ;
#1403 = AXIS2_PLACEMENT_3D ( 'NONE', #38051, #46555, #50813 ) ;
#1402 = CARTESIAN_POINT ( 'NONE',  ( -14.20280369269832832, 0.000000000000000000, 12.40765738797303719 ) ) ;
#1404 = AXIS2_PLACEMENT_3D ( 'NONE', #55284, #38238, #29759 ) ;
#1405 = PRESENTATION_STYLE_ASSIGNMENT (( #23550 ) ) ;
#1406 = DIRECTION ( 'NONE',  ( 0.007781995580012662783, 0.000000000000000000, -0.9999697198139514409 ) ) ;
#1407 = ORIENTED_EDGE ( 'NONE', *, *, #43869, .T. ) ;
#1408 = CARTESIAN_POINT ( 'NONE',  ( -14.46888367232926420, 0.000000000000000000, 12.59025272694991315 ) ) ;
#1409 = CARTESIAN_POINT ( 'NONE',  ( -25.83279121425626812, 17.74370688441070953, -4.657437592157546824 ) ) ;
#1410 = CARTESIAN_POINT ( 'NONE',  ( 2.072287782118878319, 0.000000000000000000, -2.950529333540147015 ) ) ;
#1412 = VECTOR ( 'NONE', #29489, 999.9999999999998863 ) ;
#1411 = DIRECTION ( 'NONE',  ( -0.9999697198139514409, -0.000000000000000000, -0.007781995580013368816 ) ) ;
#1413 = EDGE_CURVE ( 'NONE', #42953, #21409, #19076, .T. ) ;
#1414 = VECTOR ( 'NONE', #33309, 1000.000000000000227 ) ;
#1415 = CARTESIAN_POINT ( 'NONE',  ( -16.44346267919223692, 1.095915999411505526, 3.034165600300908316 ) ) ;
#1416 = AXIS2_PLACEMENT_3D ( 'NONE', #28813, #46114, #2932 ) ;
#1417 = EDGE_CURVE ( 'NONE', #18340, #51526, #19618, .T. ) ;
#1418 = PLANE ( 'NONE',  #2434 ) ;
#1419 = ADVANCED_FACE ( 'NONE', ( #45430 ), #46018, .F. ) ;
#1420 = DIRECTION ( 'NONE',  ( -0.005961354470445682716, -0.6427876096865404731, 0.7660212471507180654 ) ) ;
#1421 = VERTEX_POINT ( 'NONE', #36366 ) ;
#1422 = VECTOR ( 'NONE', #47528, 999.9999999999998863 ) ;
#1423 = AXIS2_PLACEMENT_3D ( 'NONE', #1553, #32215, #31919 ) ;
#1424 = ORIENTED_EDGE ( 'NONE', *, *, #42445, .T. ) ;
#1425 = DIRECTION ( 'NONE',  ( -0.3620778797217455991, 0.000000000000000000, -0.9321478471874540261 ) ) ;
#1426 = LINE ( 'NONE', #22468, #34979 ) ;
#1427 = EDGE_CURVE ( 'NONE', #54304, #8877, #15346, .T. ) ;
#1428 = VERTEX_POINT ( 'NONE', #53969 ) ;
#1429 = EDGE_CURVE ( 'NONE', #4025, #83, #14793, .T. ) ;
#1430 = CARTESIAN_POINT ( 'NONE',  ( -16.06709938707323460, 0.000000000000000000, 13.13181314741652628 ) ) ;
#1431 = EDGE_LOOP ( 'NONE', ( #16342, #44010, #36700, #33808 ) ) ;
#1432 = DIRECTION ( 'NONE',  ( 0.005961354470445682716, -0.6427876096865404731, -0.7660212471507180654 ) ) ;
#1433 = ADVANCED_FACE ( 'NONE', ( #11069 ), #23584, .F. ) ;
#1434 = VECTOR ( 'NONE', #38934, 1000.000000000000227 ) ;
#1435 = VERTEX_POINT ( 'NONE', #54250 ) ;
#1436 = ORIENTED_EDGE ( 'NONE', *, *, #48216, .T. ) ;
#1437 = VERTEX_POINT ( 'NONE', #50556 ) ;
#1438 = AXIS2_PLACEMENT_3D ( 'NONE', #9953, #1699, #27259 ) ;
#1439 = PLANE ( 'NONE',  #39281 ) ;
#1440 = LINE ( 'NONE', #54237, #2392 ) ;
#1441 = AXIS2_PLACEMENT_3D ( 'NONE', #56035, #34438, #47497 ) ;
#1442 = CARTESIAN_POINT ( 'NONE',  ( -15.53393805551735518, 0.000000000000000000, 4.330186357922316986 ) ) ;
#1443 = EDGE_CURVE ( 'NONE', #5744, #52834, #50257, .T. ) ;
#1444 = DIRECTION ( 'NONE',  ( 0.005002170337468016433, -0.7660444431189770143, -0.6427681459581293666 ) ) ;
#1445 = ORIENTED_EDGE ( 'NONE', *, *, #245, .T. ) ;
#1446 = VERTEX_POINT ( 'NONE', #24416 ) ;
#1447 = EDGE_CURVE ( 'NONE', #35209, #22415, #6545, .T. ) ;
#1448 = VECTOR ( 'NONE', #51351, 1000.000000000000227 ) ;
#1449 = VECTOR ( 'NONE', #30800, 999.9999999999998863 ) ;
#1450 = CARTESIAN_POINT ( 'NONE',  ( -67.59744393630020909, -9.446281902138684572, -7.461798308327055373 ) ) ;
#1451 = VERTEX_POINT ( 'NONE', #20143 ) ;
#1452 = CARTESIAN_POINT ( 'NONE',  ( -18.66354898467281132, 0.000000000000000000, 14.21960318569776582 ) ) ;
#1453 = ORIENTED_EDGE ( 'NONE', *, *, #9204, .F. ) ;
#1454 = CARTESIAN_POINT ( 'NONE',  ( -10.27421835998572064, 0.000000000000000000, 10.96090226820206048 ) ) ;
#1455 = LINE ( 'NONE', #26729, #38520 ) ;
#1456 = AXIS2_PLACEMENT_3D ( 'NONE', #26545, #39337, #35359 ) ;
#1457 = ORIENTED_EDGE ( 'NONE', *, *, #49593, .F. ) ;
#1458 = AXIS2_PLACEMENT_3D ( 'NONE', #12983, #17516, #34849 ) ;
#1459 = DIRECTION ( 'NONE',  ( -0.9335804264972041855, 0.3583679495452941621, 0.000000000000000000 ) ) ;
#1460 = EDGE_LOOP ( 'NONE', ( #55447, #31584, #11570, #21958 ) ) ;
#1461 = VECTOR ( 'NONE', #27925, 1000.000000000000227 ) ;
#1462 = CARTESIAN_POINT ( 'NONE',  ( -19.45503627000849889, 0.000000000000000000, 7.556996783084074742 ) ) ;
#1463 = VECTOR ( 'NONE', #33129, 1000.000000000000000 ) ;
#1464 = EDGE_LOOP ( 'NONE', ( #52364, #1521, #20842, #38091 ) ) ;
#1465 = LINE ( 'NONE', #326, #4980 ) ;
#1466 = DIRECTION ( 'NONE',  ( 0.5449076811759707706, 0.6444004775717708799, -0.5364919789714476250 ) ) ;
#1467 = CARTESIAN_POINT ( 'NONE',  ( -12.60458797795435615, 0.000000000000000000, 11.86609696750642229 ) ) ;
#1468 = EDGE_LOOP ( 'NONE', ( #876, #46291, #23991, #39804 ) ) ;
#1469 = CARTESIAN_POINT ( 'NONE',  ( -17.62242848232430248, -0.5179957512181546653, 3.709944023437250937 ) ) ;
#1470 = CARTESIAN_POINT ( 'NONE',  ( -17.68167742291825917, 0.000000000000000000, 7.468134768223175790 ) ) ;
#1471 = EDGE_CURVE ( 'NONE', #33376, #28974, #15086, .T. ) ;
#1472 = CARTESIAN_POINT ( 'NONE',  ( -11.40636015113596180, 0.000000000000000000, 11.32142374880780089 ) ) ;
#1473 = DIRECTION ( 'NONE',  ( -0.7660212471507179544, -0.6427876096865405842, -0.005961354470445141482 ) ) ;
#1474 = DIRECTION ( 'NONE',  ( 0.7660212471507180654, -0.6427876096865404731, 0.005961354470445141482 ) ) ;
#1475 = VECTOR ( 'NONE', #48134, 1000.000000000000227 ) ;
#1476 = DIRECTION ( 'NONE',  ( 0.005002170337468016433, -0.7660444431189770143, -0.6427681459581293666 ) ) ;
#1477 = VERTEX_POINT ( 'NONE', #37476 ) ;
#1478 = DIRECTION ( 'NONE',  ( 0.7660212471507180654, -0.6427876096865404731, 0.005961354470445141482 ) ) ;
#1479 = DIRECTION ( 'NONE',  ( 0.005002170337468016433, -0.7660444431189770143, -0.6427681459581293666 ) ) ;
#1480 = CARTESIAN_POINT ( 'NONE',  ( -67.47740846882294363, -0.6008377845323265021, 3.370402386375713100 ) ) ;
#1481 = ORIENTED_EDGE ( 'NONE', *, *, #25153, .F. ) ;
#1482 = CARTESIAN_POINT ( 'NONE',  ( -13.53673582514181106, 0.000000000000000000, 12.22817484722816772 ) ) ;
#1483 = DIRECTION ( 'NONE',  ( 0.9999697198139515519, 0.000000000000000000, 0.007781995580013368816 ) ) ;
#1484 = VECTOR ( 'NONE', #18223, 999.9999999999998863 ) ;
#1485 = ORIENTED_EDGE ( 'NONE', *, *, #19321, .F. ) ;
#1486 = EDGE_CURVE ( 'NONE', #3168, #13096, #49718, .T. ) ;
#1487 = EDGE_CURVE ( 'NONE', #51971, #54306, #32119, .T. ) ;
#1488 = VECTOR ( 'NONE', #8921, 1000.000000000000227 ) ;
#1489 = LINE ( 'NONE', #5748, #12278 ) ;
#1490 = CARTESIAN_POINT ( 'NONE',  ( -12.28303617674575676, 0.000000000000000000, 4.555491684261172125 ) ) ;
#1491 = EDGE_CURVE ( 'NONE', #22884, #49289, #1983, .T. ) ;
#1492 = CARTESIAN_POINT ( 'NONE',  ( 2.072287782118878319, 0.000000000000000000, -2.950529333540147015 ) ) ;
#1493 = ORIENTED_EDGE ( 'NONE', *, *, #46265, .F. ) ;
#1494 = VECTOR ( 'NONE', #9598, 1000.000000000000227 ) ;
#1495 = VERTEX_POINT ( 'NONE', #32662 ) ;
#1496 = FACE_OUTER_BOUND ( 'NONE', #15908, .T. ) ;
#1497 = DIRECTION ( 'NONE',  ( 0.6427681459581294776, -0.7660444431189769032, 0.005002170337467562802 ) ) ;
#1498 = AXIS2_PLACEMENT_3D ( 'NONE', #24554, #42170, #41870 ) ;
#1499 = DIRECTION ( 'NONE',  ( 0.007781995580012663651, 0.000000000000000000, -0.9999697198139515519 ) ) ;
#1501 = DIRECTION ( 'NONE',  ( 0.007781995580012663651, -3.146120232559066537E-19, -0.9999697198139514409 ) ) ;
#1500 = AXIS2_PLACEMENT_3D ( 'NONE', #43014, #38774, #50692 ) ;
#1502 = ORIENTED_EDGE ( 'NONE', *, *, #53584, .F. ) ;
#1503 = EDGE_CURVE ( 'NONE', #30960, #29943, #6837, .T. ) ;
#1504 = LINE ( 'NONE', #1200, #53029 ) ;
#1505 = ORIENTED_EDGE ( 'NONE', *, *, #3606, .T. ) ;
#1506 = DIRECTION ( 'NONE',  ( 0.000000000000000000, 1.000000000000000000, 0.000000000000000000 ) ) ;
#1507 = AXIS2_PLACEMENT_3D ( 'NONE', #20130, #46845, #16175 ) ;
#1508 = ADVANCED_FACE ( 'NONE', ( #2560 ), #19881, .F. ) ;
#1509 = CIRCLE ( 'NONE', #36867, 0.5000000000000004441 ) ;
#1510 = CARTESIAN_POINT ( 'NONE',  ( -20.03477888584858846, 2.553033558614007603, 8.853472636018112851 ) ) ;
#1511 = ORIENTED_EDGE ( 'NONE', *, *, #27999, .T. ) ;
#1512 = EDGE_CURVE ( 'NONE', #29979, #50929, #15906, .T. ) ;
#1513 = FACE_OUTER_BOUND ( 'NONE', #55549, .T. ) ;
#1514 = DIRECTION ( 'NONE',  ( 0.6427681459581294776, -0.7660444431189769032, 0.005002170337467562802 ) ) ;
#1515 = LINE ( 'NONE', #26231, #7564 ) ;
#1516 = EDGE_LOOP ( 'NONE', ( #28306, #44050, #3769, #25827 ) ) ;
#1517 = EDGE_CURVE ( 'NONE', #28225, #21479, #11655, .T. ) ;
#1518 = DIRECTION ( 'NONE',  ( -0.6427681459581293666, -0.7660444431189770143, -0.005002170337467561935 ) ) ;
#1519 = ORIENTED_EDGE ( 'NONE', *, *, #39376, .F. ) ;
#1520 = VECTOR ( 'NONE', #41202, 1000.000000000000227 ) ;
#1521 = ORIENTED_EDGE ( 'NONE', *, *, #45656, .F. ) ;
#1522 = ORIENTED_EDGE ( 'NONE', *, *, #10895, .F. ) ;
#1523 = CARTESIAN_POINT ( 'NONE',  ( -13.43725194175183901, 0.2864062442990034651, 2.570847542666338192 ) ) ;
#1524 = EDGE_LOOP ( 'NONE', ( #27416, #46123, #51377, #53382 ) ) ;
#1525 = CARTESIAN_POINT ( 'NONE',  ( -19.84496024468298003, -5.375054281893166142, 4.418285240812005910 ) ) ;
#1526 = ORIENTED_EDGE ( 'NONE', *, *, #11212, .T. ) ;
#1527 = DIRECTION ( 'NONE',  ( 0.007781995580012663651, -3.146120232559066537E-19, -0.9999697198139514409 ) ) ;
#1528 = CARTESIAN_POINT ( 'NONE',  ( -21.47341775636118655, -0.1191753592594197858, 5.122631121243466090 ) ) ;
#1529 = VERTEX_POINT ( 'NONE', #23332 ) ;
#1530 = AXIS2_PLACEMENT_3D ( 'NONE', #51224, #50923, #33906 ) ;
#1531 = CARTESIAN_POINT ( 'NONE',  ( -9.777102069609235002, 0.000000000000000000, 6.790985861763807030 ) ) ;
#1532 = ORIENTED_EDGE ( 'NONE', *, *, #1719, .F. ) ;
#1533 = VECTOR ( 'NONE', #44302, 1000.000000000000114 ) ;
#1534 = LINE ( 'NONE', #39869, #13793 ) ;
#1535 = FACE_OUTER_BOUND ( 'NONE', #7711, .T. ) ;
#1536 = CARTESIAN_POINT ( 'NONE',  ( -22.40634380310664397, 0.000000000000000000, 5.584705972946605534 ) ) ;
#1537 = FACE_OUTER_BOUND ( 'NONE', #25561, .T. ) ;
#1538 = CARTESIAN_POINT ( 'NONE',  ( -17.74560456716937296, 0.000000000000000000, 3.774316574337878372 ) ) ;
#1539 = PLANE ( 'NONE',  #18308 ) ;
#1540 = FILL_AREA_STYLE ('',( #36740 ) ) ;
#1541 = ORIENTED_EDGE ( 'NONE', *, *, #2850, .F. ) ;
#1542 = ADVANCED_FACE ( 'NONE', ( #25538 ), #55356, .F. ) ;
#1543 = ORIENTED_EDGE ( 'NONE', *, *, #7873, .F. ) ;
#1544 = VECTOR ( 'NONE', #27226, 1000.000000000000114 ) ;
#1545 = LINE ( 'NONE', #15176, #16486 ) ;
#1546 = CARTESIAN_POINT ( 'NONE',  ( -6.389729114256917697, 6.241674792422348794, 5.700361359755299340 ) ) ;
#1547 = EDGE_CURVE ( 'NONE', #35486, #53425, #42856, .T. ) ;
#1548 = CARTESIAN_POINT ( 'NONE',  ( -20.31146284415708791, 2.876837460659007473, 9.492363449552833288 ) ) ;
#1549 = VECTOR ( 'NONE', #27844, 999.9999999999998863 ) ;
#1550 = CARTESIAN_POINT ( 'NONE',  ( -19.85946097050258174, -2.622721114510660367, 4.511731653252694763 ) ) ;
#1551 = ORIENTED_EDGE ( 'NONE', *, *, #30791, .T. ) ;
#1552 = EDGE_CURVE ( 'NONE', #19985, #6581, #39063, .T. ) ;
#1553 = CARTESIAN_POINT ( 'NONE',  ( -15.88130887279446490, 0.000000000000000000, 3.050160814894388839 ) ) ;
#1554 = CARTESIAN_POINT ( 'NONE',  ( -70.00279782826048347, 0.1332992376639058896, -7.501782499249456393 ) ) ;
#1555 = ORIENTED_EDGE ( 'NONE', *, *, #5021, .T. ) ;
#1556 = LINE ( 'NONE', #14052, #54697 ) ;
#1557 = DIRECTION ( 'NONE',  ( -0.5364919789714478471, 0.6444004775717705469, -0.5449076811759709926 ) ) ;
#1558 = VERTEX_POINT ( 'NONE', #16745 ) ;
#1559 = EDGE_CURVE ( 'NONE', #32592, #16959, #50811, .T. ) ;
#1560 = ADVANCED_FACE ( 'NONE', ( #7372 ), #3960, .F. ) ;
#1561 = EDGE_CURVE ( 'NONE', #35486, #15388, #38900, .T. ) ;
#1562 = CARTESIAN_POINT ( 'NONE',  ( -67.43178107170270152, -8.821979906182226827, -4.591303796237533597 ) ) ;
#1563 = CARTESIAN_POINT ( 'NONE',  ( -12.15271748404464880, 0.000000000000000000, 1.601849296007406664 ) ) ;
#1564 = CARTESIAN_POINT ( 'NONE',  ( -26.13337879274045505, 0.000000000000000000, 6.833023547870798353 ) ) ;
#1565 = ADVANCED_FACE ( 'NONE', ( #21285 ), #16449, .F. ) ;
#1566 = PLANE ( 'NONE',  #2395 ) ;
#1567 = DIRECTION ( 'NONE',  ( -0.9999697198139514409, -0.000000000000000000, -0.007781995580013368816 ) ) ;
#1568 = EDGE_LOOP ( 'NONE', ( #10952, #49342, #29271, #51314 ) ) ;
#1569 = ORIENTED_EDGE ( 'NONE', *, *, #18264, .F. ) ;
#1570 = DIRECTION ( 'NONE',  ( 0.6427681459581294776, -0.7660444431189769032, 0.005002170337467562802 ) ) ;
#1571 = DIRECTION ( 'NONE',  ( 0.000000000000000000, -0.000000000000000000, -1.000000000000000000 ) ) ;
#1572 = DIRECTION ( 'NONE',  ( 0.6427681459581294776, -0.7660444431189769032, 0.005002170337467562802 ) ) ;
#1573 = CARTESIAN_POINT ( 'NONE',  ( -26.13493519185646008, 0.000000000000000000, 7.033017491833586377 ) ) ;
#1574 = PLANE ( 'NONE',  #11300 ) ;
#1575 = VERTEX_POINT ( 'NONE', #34083 ) ;
#1576 = CARTESIAN_POINT ( 'NONE',  ( -15.70074161002902180, -1.003701604285657911, 2.947999021814709852 ) ) ;
#1577 = CARTESIAN_POINT ( 'NONE',  ( -29.86197018149027116, 0.000000000000000000, 8.281335066757780083 ) ) ;
#1578 = EDGE_CURVE ( 'NONE', #13246, #30223, #12504, .T. ) ;
#1580 = VECTOR ( 'NONE', #33352, 1000.000000000000000 ) ;
#1579 = DIRECTION ( 'NONE',  ( 0.5364919789714477361, 0.6444004775717706579, 0.5449076811759711036 ) ) ;
#1581 = DIRECTION ( 'NONE',  ( -0.9999697198139514409, -0.000000000000000000, -0.007781995580013368816 ) ) ;
#1582 = ORIENTED_EDGE ( 'NONE', *, *, #44254, .F. ) ;
#1583 = EDGE_CURVE ( 'NONE', #28250, #41541, #34356, .T. ) ;
#1584 = CARTESIAN_POINT ( 'NONE',  ( -24.26908309836554878, 0.000000000000000000, 6.108867788427308376 ) ) ;
#1585 = EDGE_LOOP ( 'NONE', ( #23253, #50007, #8190, #13525 ) ) ;
#1586 = LINE ( 'NONE', #52975, #43142 ) ;
#1587 = LINE ( 'NONE', #18914, #3012 ) ;
#1588 = VERTEX_POINT ( 'NONE', #29546 ) ;
#1589 = ADVANCED_FACE ( 'NONE', ( #55100 ), #12204, .F. ) ;
#1590 = VECTOR ( 'NONE', #12067, 1000.000000000000227 ) ;
#1591 = CARTESIAN_POINT ( 'NONE',  ( -21.64383464956858560, 4.981562823951511731, 13.46411479766764785 ) ) ;
#1592 = ORIENTED_EDGE ( 'NONE', *, *, #6327, .F. ) ;
#1593 = EDGE_CURVE ( 'NONE', #30130, #34473, #3113, .T. ) ;
#1594 = ORIENTED_EDGE ( 'NONE', *, *, #32462, .T. ) ;
#1595 = ORIENTED_EDGE ( 'NONE', *, *, #40065, .F. ) ;
#1596 = DIRECTION ( 'NONE',  ( 0.005002170337468016433, -0.7660444431189770143, -0.6427681459581293666 ) ) ;
#1597 = ORIENTED_EDGE ( 'NONE', *, *, #51155, .F. ) ;
#1598 = EDGE_LOOP ( 'NONE', ( #12539, #23880, #1828, #12173 ) ) ;
#1599 = CARTESIAN_POINT ( 'NONE',  ( -27.56484202182514665, 16.74370688441070953, -4.657437592157546824 ) ) ;
#1600 = FACE_OUTER_BOUND ( 'NONE', #30295, .T. ) ;
#1601 = ORIENTED_EDGE ( 'NONE', *, *, #54889, .T. ) ;
#1602 = EDGE_LOOP ( 'NONE', ( #43725, #53528, #14096, #9125 ) ) ;
#1603 = LINE ( 'NONE', #18643, #29493 ) ;
#1604 = VERTEX_POINT ( 'NONE', #46550 ) ;
#1605 = ORIENTED_EDGE ( 'NONE', *, *, #16748, .T. ) ;
#1606 = CARTESIAN_POINT ( 'NONE',  ( 2.072287782118878319, 0.000000000000000000, -2.950529333540147015 ) ) ;
#1607 = CARTESIAN_POINT ( 'NONE',  ( -17.65868499487599763, 0.000000000000000000, 4.513657142161060065 ) ) ;
#1608 = CARTESIAN_POINT ( 'NONE',  ( 2.072287782118878319, 0.000000000000000000, -2.950529333540147015 ) ) ;
#1609 = DIRECTION ( 'NONE',  ( 0.005961354470445682716, -0.6427876096865404731, -0.7660212471507180654 ) ) ;
#1610 = EDGE_LOOP ( 'NONE', ( #22629, #50899, #33846, #1644 ) ) ;
#1611 = CARTESIAN_POINT ( 'NONE',  ( -20.04277098628171672, 4.819660872929012463, 4.313452222389104307 ) ) ;
#1612 = ORIENTED_EDGE ( 'NONE', *, *, #40578, .F. ) ;
#1613 = DIRECTION ( 'NONE',  ( 0.5364919789714477361, 0.6444004775717706579, 0.5449076811759711036 ) ) ;
#1614 = FACE_OUTER_BOUND ( 'NONE', #10339, .T. ) ;
#1615 = VECTOR ( 'NONE', #55757, 999.9999999999998863 ) ;
#1616 = CARTESIAN_POINT ( 'NONE',  ( -19.60912206198628027, -0.1191753592594197858, 4.398475361799976113 ) ) ;
#1617 = DIRECTION ( 'NONE',  ( -0.005961354470445682716, -0.6427876096865404731, 0.7660212471507180654 ) ) ;
#1618 = CARTESIAN_POINT ( 'NONE',  ( -13.09143909235258363, -0.1191753592594181482, 1.866785954948907866 ) ) ;
#1619 = LINE ( 'NONE', #17833, #9611 ) ;
#1620 = EDGE_LOOP ( 'NONE', ( #6107, #50680, #51894, #38119 ) ) ;
#1621 = CARTESIAN_POINT ( 'NONE',  ( -10.47421230394850866, 0.000000000000000000, 10.95934586908605723 ) ) ;
#1622 = EDGE_LOOP ( 'NONE', ( #44451, #53456, #18787, #13593 ) ) ;
#1623 = EDGE_CURVE ( 'NONE', #29206, #2049, #17289, .T. ) ;
#1624 = EDGE_CURVE ( 'NONE', #10121, #53596, #17042, .T. ) ;
#1625 = VECTOR ( 'NONE', #36384, 1000.000000000000227 ) ;
#1626 = DIRECTION ( 'NONE',  ( -0.5449076811759708816, 0.6444004775717707689, 0.5364919789714475140 ) ) ;
#1627 = CARTESIAN_POINT ( 'NONE',  ( -12.19950532623806083, -0.1191753592594194527, 6.672131131384362313 ) ) ;
#1628 = DIRECTION ( 'NONE',  ( 0.007781995580012663651, -3.146120232559066537E-19, -0.9999697198139514409 ) ) ;
#1629 = DIRECTION ( 'NONE',  ( 0.5364919789714477361, 0.6444004775717706579, 0.5449076811759711036 ) ) ;
#1630 = EDGE_CURVE ( 'NONE', #15384, #51326, #24995, .T. ) ;
#1631 = FACE_OUTER_BOUND ( 'NONE', #54256, .T. ) ;
#1632 = CARTESIAN_POINT ( 'NONE',  ( -67.21206727041581530, 2.489116509966271308E-16, 4.722169080041621392 ) ) ;
#1633 = EDGE_LOOP ( 'NONE', ( #50284, #3568, #21928 ) ) ;
#1634 = CARTESIAN_POINT ( 'NONE',  ( -28.32679246876683266, 14.57174378119085389, 4.727889153708476400 ) ) ;
#1635 = CARTESIAN_POINT ( 'NONE',  ( -9.601946002769009780, -9.248839861434568377, 0.5113483352705097129 ) ) ;
#1636 = LINE ( 'NONE', #18963, #55409 ) ;
#1637 = LINE ( 'NONE', #36281, #49116 ) ;
#1638 = DIRECTION ( 'NONE',  ( 0.9999697198139515519, 0.000000000000000000, 0.007781995580013368816 ) ) ;
#1639 = FACE_OUTER_BOUND ( 'NONE', #12689, .T. ) ;
#1640 = LINE ( 'NONE', #18969, #39650 ) ;
#1641 = CARTESIAN_POINT ( 'NONE',  ( -20.54204810873173415, 0.000000000000000000, 4.860550213503115558 ) ) ;
#1642 = ORIENTED_EDGE ( 'NONE', *, *, #33678, .F. ) ;
#1643 = EDGE_CURVE ( 'NONE', #21963, #1847, #29822, .T. ) ;
#1644 = ORIENTED_EDGE ( 'NONE', *, *, #32334, .T. ) ;
#1645 = VERTEX_POINT ( 'NONE', #42583 ) ;
#1646 = ORIENTED_EDGE ( 'NONE', *, *, #2853, .T. ) ;
#1647 = EDGE_CURVE ( 'NONE', #9132, #31598, #12762, .T. ) ;
#1648 = ORIENTED_EDGE ( 'NONE', *, *, #21805, .T. ) ;
#1649 = CARTESIAN_POINT ( 'NONE',  ( -16.53317331066696383, 0.000000000000000000, 13.31285208727739899 ) ) ;
#1650 = FACE_OUTER_BOUND ( 'NONE', #10084, .T. ) ;
#1651 = VECTOR ( 'NONE', #21471, 999.9999999999998863 ) ;
#1652 = ORIENTED_EDGE ( 'NONE', *, *, #31807, .T. ) ;
#1653 = ORIENTED_EDGE ( 'NONE', *, *, #47917, .F. ) ;
#1654 = EDGE_CURVE ( 'NONE', #18340, #41698, #56203, .T. ) ;
#1655 = ORIENTED_EDGE ( 'NONE', *, *, #42198, .T. ) ;
#1656 = DIRECTION ( 'NONE',  ( -0.1139275668495183524, 0.9934890585767659488, 4.694855797473114533E-16 ) ) ;
#1657 = LINE ( 'NONE', #15534, #41867 ) ;
#1658 = CARTESIAN_POINT ( 'NONE',  ( -19.60990026154428278, 0.000000000000000000, 4.498472333781370125 ) ) ;
#1659 = ORIENTED_EDGE ( 'NONE', *, *, #8572, .F. ) ;
#1660 = CARTESIAN_POINT ( 'NONE',  ( -14.01701317841955508, 0.000000000000000000, 2.326005055450897085 ) ) ;
#1661 = VERTEX_POINT ( 'NONE', #52502 ) ;
#1662 = CARTESIAN_POINT ( 'NONE',  ( -16.81190032086591302, 0.000000000000000000, 3.212244750653343583 ) ) ;
#1663 = FACE_OUTER_BOUND ( 'NONE', #52430, .T. ) ;
#1664 = LINE ( 'NONE', #819, #18243 ) ;
#1665 = CARTESIAN_POINT ( 'NONE',  ( -21.47263955680318404, 0.000000000000000000, 5.022634149262071190 ) ) ;
#1666 = CARTESIAN_POINT ( 'NONE',  ( -18.15206242676991266, 0.000000000000000000, 8.203138262970696815 ) ) ;
#1667 = CARTESIAN_POINT ( 'NONE',  ( -12.15193928448664629, -0.1191753592594197858, 1.501852324026012209 ) ) ;
#1669 = FACE_OUTER_BOUND ( 'NONE', #21654, .T. ) ;
#1668 = B_SPLINE_CURVE_WITH_KNOTS ( 'NONE', 3,
 ( #32011, #15259, #45343, #19212, #36548, #45094, #32574, #44247, #36029, #5608, #5905, #22931, #27771, #6196, #23231, #5351 ),
 .UNSPECIFIED., .F., .F.,
 ( 4, 2, 2, 2, 2, 2, 2, 4 ),
 ( 2.629190268277348252E-18, 0.0004228030555968962517, 0.0008456061111937897929, 0.001268409166790682900, 0.001691212222387575900, 0.002114015277984469116, 0.002536818333581361898, 0.003382424444775107997 ),
 .UNSPECIFIED. ) ;
#1670 = ORIENTED_EDGE ( 'NONE', *, *, #52960, .T. ) ;
#1671 = CARTESIAN_POINT ( 'NONE',  ( -13.11440885239381693, -0.1191753592594183703, 4.818350791559519841 ) ) ;
#1672 = ADVANCED_FACE ( 'NONE', ( #1079 ), #17888, .F. ) ;
#1673 = ORIENTED_EDGE ( 'NONE', *, *, #54482, .F. ) ;
#1674 = EDGE_CURVE ( 'NONE', #6876, #28453, #39741, .T. ) ;
#1675 = CARTESIAN_POINT ( 'NONE',  ( -13.31607370880347929, -3.108426967578159061, 6.955805194728735152 ) ) ;
#1676 = DIRECTION ( 'NONE',  ( -0.5364919789714478471, 0.6444004775717705469, -0.5449076811759709926 ) ) ;
#1677 = FACE_OUTER_BOUND ( 'NONE', #42898, .T. ) ;
#1678 = DIRECTION ( 'NONE',  ( 0.007781995580012663651, 0.000000000000000000, -0.9999697198139515519 ) ) ;
#1679 = CARTESIAN_POINT ( 'NONE',  ( -13.48270103031678957, 0.000000000000000000, 5.284819754588673923 ) ) ;
#1680 = CARTESIAN_POINT ( 'NONE',  ( -23.33693525117809386, 0.000000000000000000, 5.746789908705562944 ) ) ;
#1681 = ADVANCED_FACE ( 'NONE', ( #18414 ), #9333, .F. ) ;
#1682 = EDGE_CURVE ( 'NONE', #1080, #35417, #22122, .T. ) ;
#1683 = DIRECTION ( 'NONE',  ( 0.7660212471507180654, -0.6427876096865404731, 0.005961354470445141482 ) ) ;
#1684 = DIRECTION ( 'NONE',  ( 0.7660212471507180654, -0.6427876096865404731, 0.005961354470445141482 ) ) ;
#1685 = FACE_OUTER_BOUND ( 'NONE', #47461, .T. ) ;
#1686 = ORIENTED_EDGE ( 'NONE', *, *, #18158, .F. ) ;
#1687 = LINE ( 'NONE', #31535, #13941 ) ;
#1688 = DIRECTION ( 'NONE',  ( -0.005002170337468016433, -0.7660444431189770143, 0.6427681459581293666 ) ) ;
#1689 = CARTESIAN_POINT ( 'NONE',  ( -68.44026216309750055, -1.000000000000000444, 5.059064008999124340 ) ) ;
#1690 = FACE_OUTER_BOUND ( 'NONE', #55480, .T. ) ;
#1691 = AXIS2_PLACEMENT_3D ( 'NONE', #351, #44090, #52871 ) ;
#1692 = DIRECTION ( 'NONE',  ( 0.007781995580012662783, 0.000000000000000000, -0.9999697198139514409 ) ) ;
#1693 = LINE ( 'NONE', #31541, #10608 ) ;
#1694 = CARTESIAN_POINT ( 'NONE',  ( -28.93137873341882127, 0.000000000000000000, 8.119251130998824451 ) ) ;
#1695 = ADVANCED_FACE ( 'NONE', ( #9918 ), #31506, .F. ) ;
#1696 = ORIENTED_EDGE ( 'NONE', *, *, #17502, .T. ) ;
#1697 = ORIENTED_EDGE ( 'NONE', *, *, #15275, .T. ) ;
#1698 = FACE_OUTER_BOUND ( 'NONE', #9318, .T. ) ;
#1699 = DIRECTION ( 'NONE',  ( -0.005961354470445682716, -0.6427876096865404731, 0.7660212471507180654 ) ) ;
#1700 = ORIENTED_EDGE ( 'NONE', *, *, #48020, .F. ) ;
#1701 = CARTESIAN_POINT ( 'NONE',  ( -19.60990026154428278, 0.000000000000000000, 4.498472333781370125 ) ) ;
#1702 = VERTEX_POINT ( 'NONE', #44276 ) ;
#1703 = CARTESIAN_POINT ( 'NONE',  ( -6.110905869600904872, 1.712176620043476140E-14, -3.600000000000000089 ) ) ;
#1704 = ORIENTED_EDGE ( 'NONE', *, *, #38915, .T. ) ;
#1705 = ORIENTED_EDGE ( 'NONE', *, *, #38327, .F. ) ;
#1706 = ORIENTED_EDGE ( 'NONE', *, *, #33420, .F. ) ;
#1707 = DIRECTION ( 'NONE',  ( 0.9999697198139515519, 0.000000000000000000, 0.007781995580013368816 ) ) ;
#1708 = LINE ( 'NONE', #19605, #26848 ) ;
#1709 = DIRECTION ( 'NONE',  ( 0.6427681459581294776, -0.7660444431189769032, 0.005002170337467562802 ) ) ;
#1710 = EDGE_LOOP ( 'NONE', ( #9317, #630, #4247, #49002 ) ) ;
#1711 = EDGE_CURVE ( 'NONE', #14416, #38344, #35207, .T. ) ;
#1712 = ORIENTED_EDGE ( 'NONE', *, *, #14966, .F. ) ;
#1713 = DIRECTION ( 'NONE',  ( -0.5364919789714478471, 0.6444004775717705469, -0.5449076811759709926 ) ) ;
#1714 = EDGE_LOOP ( 'NONE', ( #14645, #47327, #53878, #47076 ) ) ;
#1715 = FACE_OUTER_BOUND ( 'NONE', #7240, .T. ) ;
#1716 = VERTEX_POINT ( 'NONE', #35753 ) ;
#1717 = PLANE ( 'NONE',  #40309 ) ;
#1718 = DIRECTION ( 'NONE',  ( 0.7660212471507180654, -0.6427876096865404731, 0.005961354470445141482 ) ) ;
#1719 = EDGE_CURVE ( 'NONE', #2367, #13439, #22962, .T. ) ;
#1720 = EDGE_LOOP ( 'NONE', ( #41677, #45771, #5248, #31726 ) ) ;
#1721 = DIRECTION ( 'NONE',  ( 0.5449076811759707706, 0.6444004775717708799, -0.5364919789714476250 ) ) ;
#1722 = ORIENTED_EDGE ( 'NONE', *, *, #3150, .T. ) ;
#1723 = EDGE_CURVE ( 'NONE', #25204, #23927, #44525, .T. ) ;
#1724 = ADVANCED_FACE ( 'NONE', ( #4528 ), #39456, .F. ) ;
#1725 = CARTESIAN_POINT ( 'NONE',  ( -26.13415699229845757, -0.1191753592594197858, 6.933020519852192365 ) ) ;
#1726 = ORIENTED_EDGE ( 'NONE', *, *, #18025, .T. ) ;
#1727 = FACE_OUTER_BOUND ( 'NONE', #754, .T. ) ;
#1728 = DIRECTION ( 'NONE',  ( -0.2426528472758542054, 0.7422098413412800966, -0.6246952433987894571 ) ) ;
#1729 = DIRECTION ( 'NONE',  ( 0.7660212471507180654, -0.6427876096865404731, 0.005961354470445141482 ) ) ;
#1730 = ADVANCED_FACE ( 'NONE', ( #34922 ), #22430, .F. ) ;
#1731 = ORIENTED_EDGE ( 'NONE', *, *, #49822, .F. ) ;
#1732 = EDGE_CURVE ( 'NONE', #55625, #45339, #1378, .T. ) ;
#1733 = DIRECTION ( 'NONE',  ( -0.8531650599175529814, -0.4028455766673920135, 0.3313982828793697877 ) ) ;
#1734 = LINE ( 'NONE', #6296, #1520 ) ;
#1735 = CARTESIAN_POINT ( 'NONE',  ( -14.55352977697969585, -0.1941918491731554897, 2.528210585817464384 ) ) ;
#1736 = CARTESIAN_POINT ( 'NONE',  ( -56.02165185617580079, 5.343604887189308705, 2.999999999999993339 ) ) ;
#1737 = PLANE ( 'NONE',  #40329 ) ;
#1738 = ADVANCED_FACE ( 'NONE', ( #13345 ), #813, .F. ) ;
#1739 = CARTESIAN_POINT ( 'NONE',  ( -12.09166439329881726, 0.000000000000000000, 5.664977193150467549 ) ) ;
#1740 = CARTESIAN_POINT ( 'NONE',  ( 3.004435629306332345, 0.000000000000000000, -3.312607213261892003 ) ) ;
#1741 = B_SPLINE_CURVE_WITH_KNOTS ( 'NONE', 3,
 ( #23369, #39838, #22787, #52607 ),
 .UNSPECIFIED., .F., .F.,
 ( 4, 4 ),
 ( 0.0001251225081293656771, 0.0003537265380804738486 ),
 .UNSPECIFIED. ) ;
#1742 = ORIENTED_EDGE ( 'NONE', *, *, #52628, .F. ) ;
#1743 = PLANE ( 'NONE',  #41578 ) ;
#1744 = PLANE ( 'NONE',  #25922 ) ;
#1745 = CARTESIAN_POINT ( 'NONE',  ( -67.30971128957258998, -0.6012107392119571125, -2.713115426956270060 ) ) ;
#1746 = EDGE_LOOP ( 'NONE', ( #15239, #15077, #53540, #43309 ) ) ;
#1747 = DIRECTION ( 'NONE',  ( -0.5364919789714478471, 0.6444004775717705469, -0.5449076811759709926 ) ) ;
#1748 = CARTESIAN_POINT ( 'NONE',  ( -14.03218643205485883, -0.1191753592594197164, 3.333880154992445277 ) ) ;
#1749 = APPLICATION_CONTEXT ( 'automotive_design' ) ;
#1750 = ADVANCED_FACE ( 'NONE', ( #47698 ), #36054, .F. ) ;
#1751 = DIRECTION ( 'NONE',  ( -0.2426528472758542054, 0.7422098413412800966, -0.6246952433987894571 ) ) ;
#1752 = CARTESIAN_POINT ( 'NONE',  ( -15.86710544311044302, 0.000000000000000000, 13.13336954653252953 ) ) ;
#1753 = CARTESIAN_POINT ( 'NONE',  ( -27.99923088623136636, 0.000000000000000000, 7.757173251277078130 ) ) ;
#1754 = ADVANCED_FACE ( 'NONE', ( #239 ), #30667, .F. ) ;
#1755 = ORIENTED_EDGE ( 'NONE', *, *, #44018, .T. ) ;
#1756 = ORIENTED_EDGE ( 'NONE', *, *, #38402, .T. ) ;
#1757 = CARTESIAN_POINT ( 'NONE',  ( -17.69161723782338669, 0.000000000000000000, 8.745379637291446073 ) ) ;
#1758 = CARTESIAN_POINT ( 'NONE',  ( -28.93060053386082231, -0.1191753592594197858, 8.019254159017428663 ) ) ;
#1759 = DIRECTION ( 'NONE',  ( 0.007781995580012663651, -3.146120232559066537E-19, -0.9999697198139514409 ) ) ;
#1760 =( GEOMETRIC_REPRESENTATION_CONTEXT ( 3 ) GLOBAL_UNCERTAINTY_ASSIGNED_CONTEXT ( ( #42179 ) ) GLOBAL_UNIT_ASSIGNED_CONTEXT ( ( #39762, #23813, #2772 ) ) REPRESENTATION_CONTEXT ( 'NONE', 'WORKASPACE' ) );
#1761 = ORIENTED_EDGE ( 'NONE', *, *, #21176, .F. ) ;
#1762 = CARTESIAN_POINT ( 'NONE',  ( -19.60834386242827776, 0.000000000000000000, 4.298478389818581213 ) ) ;
#1763 = EDGE_LOOP ( 'NONE', ( #33530, #9431, #3298, #1481 ) ) ;
#1764 = CARTESIAN_POINT ( 'NONE',  ( -18.68917496928920485, -0.1134144341941974582, 4.041136669461655728 ) ) ;
#1765 = DIRECTION ( 'NONE',  ( -1.007958083594381669E-15, 3.869188571150967118E-16, -1.000000000000000000 ) ) ;
#1766 = ORIENTED_EDGE ( 'NONE', *, *, #22536, .T. ) ;
#1767 = CARTESIAN_POINT ( 'NONE',  ( -7.241878385602738888, 3.035725714417215393, 8.349636240898133721 ) ) ;
#1768 = CARTESIAN_POINT ( 'NONE',  ( -12.13851405436063047, 0.000000000000000000, 11.68505802764555135 ) ) ;
#1769 = FACE_OUTER_BOUND ( 'NONE', #8875, .T. ) ;
#1770 = ORIENTED_EDGE ( 'NONE', *, *, #31393, .T. ) ;
#1771 = FACE_OUTER_BOUND ( 'NONE', #10275, .T. ) ;
#1772 = EDGE_CURVE ( 'NONE', #19751, #25320, #26659, .T. ) ;
#1773 = ORIENTED_EDGE ( 'NONE', *, *, #35731, .T. ) ;
#1774 = ORIENTED_EDGE ( 'NONE', *, *, #48004, .F. ) ;
#1775 = ORIENTED_EDGE ( 'NONE', *, *, #40793, .T. ) ;
#1776 = CARTESIAN_POINT ( 'NONE',  ( -16.81345671998191449, 0.000000000000000000, 3.412238694616132495 ) ) ;
#1777 = ORIENTED_EDGE ( 'NONE', *, *, #37045, .T. ) ;
#1778 = LINE ( 'NONE', #1525, #29366 ) ;
#1779 = ORIENTED_EDGE ( 'NONE', *, *, #52572, .F. ) ;
#1780 = DIRECTION ( 'NONE',  ( -0.9999697198139514409, -0.000000000000000000, -0.007781995580013368816 ) ) ;
#1781 = LINE ( 'NONE', #1528, #50375 ) ;
#1782 = EDGE_LOOP ( 'NONE', ( #5617, #52032, #32023, #12756 ) ) ;
#1783 = PLANE ( 'NONE',  #41250 ) ;
#1784 = ORIENTED_EDGE ( 'NONE', *, *, #40845, .F. ) ;
#1785 = EDGE_CURVE ( 'NONE', #28760, #24516, #10176, .T. ) ;
#1786 = LINE ( 'NONE', #35607, #52772 ) ;
#1787 = DIRECTION ( 'NONE',  ( 0.000000000000000000, -1.000000000000000000, 0.000000000000000000 ) ) ;
#1788 = CARTESIAN_POINT ( 'NONE',  ( -9.110551994824897193, 0.000000000000000000, 3.538847790438064411 ) ) ;
#1789 = LINE ( 'NONE', #5797, #9397 ) ;
#1790 = PLANE ( 'NONE',  #53200 ) ;
#1791 = LINE ( 'NONE', #32730, #8345 ) ;
#1792 = DIRECTION ( 'NONE',  ( -0.7660212471507179544, -0.6427876096865405842, -0.005961354470445141482 ) ) ;
#1793 = ORIENTED_EDGE ( 'NONE', *, *, #49135, .F. ) ;
#1794 = EDGE_LOOP ( 'NONE', ( #7989, #15707, #6396, #6214 ) ) ;
#1795 = ADVANCED_FACE ( 'NONE', ( #54188 ), #44821, .T. ) ;
#1796 = CARTESIAN_POINT ( 'NONE',  ( -19.06409189942038651, 0.000000000000000000, 5.980048219888089989 ) ) ;
#1797 = CARTESIAN_POINT ( 'NONE',  ( 2.072287782118878319, 0.000000000000000000, -2.950529333540147015 ) ) ;
#1798 = EDGE_CURVE ( 'NONE', #10838, #20767, #53890, .T. ) ;
#1799 = PLANE ( 'NONE',  #29697 ) ;
#1800 = FACE_OUTER_BOUND ( 'NONE', #16212, .T. ) ;
#1801 = ORIENTED_EDGE ( 'NONE', *, *, #21933, .F. ) ;
#1802 = DIRECTION ( 'NONE',  ( 0.005961354470445682716, -0.6427876096865404731, -0.7660212471507180654 ) ) ;
#1803 = DIRECTION ( 'NONE',  ( 0.9999697198139515519, 0.000000000000000000, 0.007781995580013368816 ) ) ;
#1804 = EDGE_LOOP ( 'NONE', ( #46986, #41214, #8796, #21069 ) ) ;
#1805 = CARTESIAN_POINT ( 'NONE',  ( -17.36532418587302473, -0.1191753592594177458, 13.67570816655714516 ) ) ;
#1806 = FACE_OUTER_BOUND ( 'NONE', #12422, .T. ) ;
#1807 = ORIENTED_EDGE ( 'NONE', *, *, #39907, .F. ) ;
#1808 = EDGE_CURVE ( 'NONE', #9203, #5331, #5940, .T. ) ;
#1809 = CARTESIAN_POINT ( 'NONE',  ( -66.55839402557589324, -8.722187935008872017, -0.3300946888591901884 ) ) ;
#1810 = DIRECTION ( 'NONE',  ( -0.5364919789714478471, 0.6444004775717705469, -0.5449076811759709926 ) ) ;
#1811 = CARTESIAN_POINT ( 'NONE',  ( -15.57130075108602618, 0.000000000000000000, 9.131212500273253596 ) ) ;
#1812 = LINE ( 'NONE', #22848, #12386 ) ;
#1813 = CARTESIAN_POINT ( 'NONE',  ( -15.87975247367846166, 0.000000000000000000, 2.850166870931599927 ) ) ;
#1814 = EDGE_CURVE ( 'NONE', #40640, #13341, #41412, .T. ) ;
#1815 = ORIENTED_EDGE ( 'NONE', *, *, #7028, .T. ) ;
#1816 = ORIENTED_EDGE ( 'NONE', *, *, #27941, .F. ) ;
#1817 = LINE ( 'NONE', #45282, #36653 ) ;
#1818 = FACE_OUTER_BOUND ( 'NONE', #11541, .T. ) ;
#1819 = CARTESIAN_POINT ( 'NONE',  ( -13.93672754567525018, -2.784623065533161856, 2.205975334288626133 ) ) ;
#1820 = DIRECTION ( 'NONE',  ( 0.000000000000000000, -0.000000000000000000, -1.000000000000000000 ) ) ;
#1821 = DIRECTION ( 'NONE',  ( 0.6246952433987893460, 0.7422098413412802076, -0.2426528472758539279 ) ) ;
#1822 = ORIENTED_EDGE ( 'NONE', *, *, #18531, .F. ) ;
#1823 = CARTESIAN_POINT ( 'NONE',  ( -19.22961988024793101, -0.1191753592594177458, 14.39986392600063603 ) ) ;
#1824 = CARTESIAN_POINT ( 'NONE',  ( -11.20636620717317378, 0.000000000000000000, 11.32298014792380414 ) ) ;
#1825 = AXIS2_PLACEMENT_3D ( 'NONE', #11547, #16336, #50711 ) ;
#1826 = CARTESIAN_POINT ( 'NONE',  ( -14.59316804781405352, 0.000000000000000000, 2.860179368427277602 ) ) ;
#1827 = CARTESIAN_POINT ( 'NONE',  ( -20.11552963796318494, 21.04456939451101150, -4.294601649057681492 ) ) ;
#1828 = ORIENTED_EDGE ( 'NONE', *, *, #26813, .T. ) ;
#1829 = FACE_OUTER_BOUND ( 'NONE', #1763, .T. ) ;
#1830 = ORIENTED_EDGE ( 'NONE', *, *, #42815, .T. ) ;
#1831 = PLANE ( 'NONE',  #19535 ) ;
#1832 = ADVANCED_FACE ( 'NONE', ( #49075 ), #7056, .F. ) ;
#1833 = DIRECTION ( 'NONE',  ( -0.3620778797217457101, 0.000000000000000000, -0.9321478471874540261 ) ) ;
#1834 = ORIENTED_EDGE ( 'NONE', *, *, #7038, .F. ) ;
#1835 = CARTESIAN_POINT ( 'NONE',  ( -11.87243407472968926, 0.000000000000000000, 11.50246268866867361 ) ) ;
#1836 = ADVANCED_FACE ( 'NONE', ( #32600 ), #19820, .F. ) ;
#1837 = EDGE_LOOP ( 'NONE', ( #12268, #29340, #18634, #34154 ) ) ;
#1838 = EDGE_LOOP ( 'NONE', ( #6597, #46127, #54432, #23639 ) ) ;
#1839 = ORIENTED_EDGE ( 'NONE', *, *, #23407, .T. ) ;
#1840 = CARTESIAN_POINT ( 'NONE',  ( -29.14071270714143935, 15.83387752003526394, 4.730034822273776030 ) ) ;
#1841 = EDGE_CURVE ( 'NONE', #39352, #17429, #23262, .T. ) ;
#1842 = ORIENTED_EDGE ( 'NONE', *, *, #12734, .T. ) ;
#1843 = EDGE_CURVE ( 'NONE', #48446, #42740, #49362, .T. ) ;
#1844 = ORIENTED_EDGE ( 'NONE', *, *, #33961, .T. ) ;
#1845 = PLANE ( 'NONE',  #52857 ) ;
#1846 = CARTESIAN_POINT ( 'NONE',  ( -7.296103114018933411, -3.208161209119383628, 8.210037920513791221 ) ) ;
#1848 = ADVANCED_FACE ( 'NONE', ( #23525 ), #54723, .F. ) ;
#1847 = VERTEX_POINT ( 'NONE', #6765 ) ;
#1849 = EDGE_CURVE ( 'NONE', #50804, #17276, #37402, .T. ) ;
#1850 = EDGE_CURVE ( 'NONE', #29513, #38157, #10481, .T. ) ;
#1851 = ORIENTED_EDGE ( 'NONE', *, *, #8213, .F. ) ;
#1852 = FACE_OUTER_BOUND ( 'NONE', #55211, .T. ) ;
#1853 = VERTEX_POINT ( 'NONE', #6223 ) ;
#1854 = VERTEX_POINT ( 'NONE', #49659 ) ;
#1855 = DIRECTION ( 'NONE',  ( 0.5364919789714477361, 0.6444004775717706579, 0.5449076811759711036 ) ) ;
#1856 = LINE ( 'NONE', #14400, #15807 ) ;
#1857 = CARTESIAN_POINT ( 'NONE',  ( 5.221828392167458865, 0.000000000000000000, 2.393421119419573806 ) ) ;
#1858 = CARTESIAN_POINT ( 'NONE',  ( -16.76102578975193680, 0.000000000000000000, 8.583295701532488664 ) ) ;
#1859 = ORIENTED_EDGE ( 'NONE', *, *, #27376, .T. ) ;
#1860 = DIRECTION ( 'NONE',  ( 0.9999697198139515519, 0.000000000000000000, 0.007781995580013368816 ) ) ;
#1861 = ORIENTED_EDGE ( 'NONE', *, *, #23294, .F. ) ;
#1862 = AXIS2_PLACEMENT_3D ( 'NONE', #32665, #37204, #36662 ) ;
#1863 = EDGE_CURVE ( 'NONE', #7513, #21986, #2499, .T. ) ;
#1864 = LINE ( 'NONE', #31143, #6672 ) ;
#1865 = AXIS2_PLACEMENT_3D ( 'NONE', #9153, #13691, #35858 ) ;
#1866 = EDGE_CURVE ( 'NONE', #42382, #46574, #32870, .T. ) ;
#1867 = DIRECTION ( 'NONE',  ( 0.000000000000000000, -0.000000000000000000, -1.000000000000000000 ) ) ;
#1868 = CARTESIAN_POINT ( 'NONE',  ( -14.95858617223174569, -0.1191753592594189115, 2.957338628198661556 ) ) ;
#1869 = PLANE ( 'NONE',  #6895 ) ;
#1870 = EDGE_CURVE ( 'NONE', #47896, #25894, #45645, .T. ) ;
#1871 = LINE ( 'NONE', #18668, #29375 ) ;
#1872 = FACE_OUTER_BOUND ( 'NONE', #39528, .T. ) ;
#1873 = ORIENTED_EDGE ( 'NONE', *, *, #3756, .F. ) ;
#1874 = CARTESIAN_POINT ( 'NONE',  ( -11.34645787693701635, 0.000000000000000000, 3.624110157318871206 ) ) ;
#1875 = VERTEX_POINT ( 'NONE', #20074 ) ;
#1876 = EDGE_CURVE ( 'NONE', #26373, #28453, #50184, .T. ) ;
#1877 = CARTESIAN_POINT ( 'NONE',  ( -19.15468851132792949, -0.1191753592594168992, 4.771343938575395072 ) ) ;
#1878 = LINE ( 'NONE', #28028, #3322 ) ;
#1879 = DIRECTION ( 'NONE',  ( 0.9999697198139515519, 0.000000000000000000, 0.007781995580013368816 ) ) ;
#1880 = CARTESIAN_POINT ( 'NONE',  ( -11.21901323774118708, 0.000000000000000000, 1.039777472322872098 ) ) ;
#1881 = DIRECTION ( 'NONE',  ( 0.5364919789714477361, 0.6444004775717706579, 0.5449076811759711036 ) ) ;
#1882 = LINE ( 'NONE', #53030, #51097 ) ;
#1883 = ORIENTED_EDGE ( 'NONE', *, *, #48403, .T. ) ;
#1884 = CARTESIAN_POINT ( 'NONE',  ( -10.37421533196711465, -0.1191753592594197858, 10.96012406864405975 ) ) ;
#1885 = CARTESIAN_POINT ( 'NONE',  ( -21.10695443357304768, -5.213152330870665097, 4.913652161167348709 ) ) ;
#1886 = LINE ( 'NONE', #45092, #74 ) ;
#1887 = VECTOR ( 'NONE', #32657, 999.9999999999998863 ) ;
#1888 = DIRECTION ( 'NONE',  ( -0.5449076811759708816, 0.6444004775717707689, 0.5364919789714475140 ) ) ;
#1889 = DIRECTION ( 'NONE',  ( -0.5449076811759708816, 0.6444004775717707689, 0.5364919789714475140 ) ) ;
#1890 = CARTESIAN_POINT ( 'NONE',  ( -18.86354292863559579, 0.000000000000000000, 14.21804678658176080 ) ) ;
#1891 = PLANE ( 'NONE',  #16563 ) ;
#1892 = DIRECTION ( 'NONE',  ( -0.005961354470445682716, -0.6427876096865404731, 0.7660212471507180654 ) ) ;
#1893 = DIRECTION ( 'NONE',  ( -0.5364919789714478471, 0.6444004775717705469, -0.5449076811759709926 ) ) ;
#1894 = EDGE_LOOP ( 'NONE', ( #21734, #23060 ) ) ;
#1895 = EDGE_LOOP ( 'NONE', ( #2877, #24204, #52473, #51482 ) ) ;
#1896 = VECTOR ( 'NONE', #13418, 1000.000000000000227 ) ;
#1897 = VECTOR ( 'NONE', #27769, 1000.000000000000000 ) ;
#1898 = ORIENTED_EDGE ( 'NONE', *, *, #3465, .T. ) ;
#1899 = EDGE_LOOP ( 'NONE', ( #54836, #24136, #39930, #22886 ) ) ;
#1900 = EDGE_LOOP ( 'NONE', ( #22867, #22739, #46322, #54821 ) ) ;
#1901 = VERTEX_POINT ( 'NONE', #2205 ) ;
#1902 = FACE_OUTER_BOUND ( 'NONE', #4725, .T. ) ;
#1903 = LINE ( 'NONE', #36571, #15791 ) ;
#1904 = EDGE_CURVE ( 'NONE', #27821, #18640, #31635, .T. ) ;
#1905 = EDGE_CURVE ( 'NONE', #33489, #34665, #55035, .T. ) ;
#1906 = B_SPLINE_CURVE_WITH_KNOTS ( 'NONE', 3,
 ( #20919, #47057, #9009, #51600 ),
 .UNSPECIFIED., .F., .F.,
 ( 4, 4 ),
 ( 0.000000000000000000, 1.000000000000000000 ),
 .UNSPECIFIED. ) ;
#1907 = EDGE_LOOP ( 'NONE', ( #23537, #20296, #38827, #53020 ) ) ;
#1908 = ORIENTED_EDGE ( 'NONE', *, *, #1427, .F. ) ;
#1909 = VERTEX_POINT ( 'NONE', #51604 ) ;
#1910 = ADVANCED_FACE ( 'NONE', ( #42247 ), #16380, .F. ) ;
#1911 = LINE ( 'NONE', #18409, #14781 ) ;
#1912 = CARTESIAN_POINT ( 'NONE',  ( -10.67607892912258194, 0.000000000000000000, 2.890663061687355651 ) ) ;
#1913 = LINE ( 'NONE', #19247, #34098 ) ;
#1914 = VERTEX_POINT ( 'NONE', #28905 ) ;
#1915 = DIRECTION ( 'NONE',  ( -0.6427681459581293666, -0.7660444431189770143, -0.005002170337467561935 ) ) ;
#1916 = ORIENTED_EDGE ( 'NONE', *, *, #43531, .T. ) ;
#1917 = VECTOR ( 'NONE', #13379, 1000.000000000000000 ) ;
#1918 = VECTOR ( 'NONE', #52240, 1000.000000000000227 ) ;
#1919 = DIRECTION ( 'NONE',  ( -0.6427681459581293666, -0.7660444431189770143, -0.005002170337467561935 ) ) ;
#1920 = LINE ( 'NONE', #14725, #40237 ) ;
#1921 = DIRECTION ( 'NONE',  ( 0.9999697198139515519, 0.000000000000000000, 0.007781995580013368816 ) ) ;
#1922 = DIRECTION ( 'NONE',  ( 0.005002170337468016433, -0.7660444431189770143, -0.6427681459581293666 ) ) ;
#1923 = B_SPLINE_CURVE_WITH_KNOTS ( 'NONE', 3,
 ( #45758, #18536, #18837, #36407, #54017, #2023, #19362 ),
 .UNSPECIFIED., .F., .F.,
 ( 4, 3, 4 ),
 ( 0.000000000000000000, 0.0007529153636991639358, 0.001137651663043191038 ),
 .UNSPECIFIED. ) ;
#1924 = CARTESIAN_POINT ( 'NONE',  ( -18.34343421021684861, 0.000000000000000000, 7.093652754081396949 ) ) ;
#1925 = FACE_OUTER_BOUND ( 'NONE', #48388, .T. ) ;
#1926 = LINE ( 'NONE', #7067, #350 ) ;
#1927 = EDGE_CURVE ( 'NONE', #43311, #9641, #11589, .T. ) ;
#1928 = CARTESIAN_POINT ( 'NONE',  ( -9.470713295052064495, 9.226104519242889879, 6.897120246239332175 ) ) ;
#1929 = ORIENTED_EDGE ( 'NONE', *, *, #37571, .T. ) ;
#1930 = CARTESIAN_POINT ( 'NONE',  ( 2.072287782118878319, 0.000000000000000000, -2.950529333540147015 ) ) ;
#1931 = ORIENTED_EDGE ( 'NONE', *, *, #36461, .F. ) ;
#1932 = EDGE_CURVE ( 'NONE', #7363, #44540, #47328, .T. ) ;
#1933 = CARTESIAN_POINT ( 'NONE',  ( -20.48605083020362017, 4.172053068839010059, 11.68584882396997493 ) ) ;
#1934 = DIRECTION ( 'NONE',  ( 0.5449076811759707706, 0.6444004775717708799, -0.5364919789714476250 ) ) ;
#1935 = LINE ( 'NONE', #12075, #34937 ) ;
#1936 = CARTESIAN_POINT ( 'NONE',  ( -9.319383251525813705, -0.1191753592594193140, 3.001224209265955345 ) ) ;
#1937 = FACE_OUTER_BOUND ( 'NONE', #6335, .T. ) ;
#1938 = DIRECTION ( 'NONE',  ( -0.6427681459581293666, -0.7660444431189770143, -0.005002170337467561935 ) ) ;
#1939 = CARTESIAN_POINT ( 'NONE',  ( -17.93139508144814442, 0.000000000000000000, 13.85596890686001537 ) ) ;
#1940 = VECTOR ( 'NONE', #11066, 1000.000000000000227 ) ;
#1941 = CARTESIAN_POINT ( 'NONE',  ( -16.79925329029790149, 0.000000000000000000, 13.49544742625427496 ) ) ;
#1942 = DIRECTION ( 'NONE',  ( -0.07978464360815165635, -0.004239666569833556650, 0.9968031078762230601 ) ) ;
#1943 = CARTESIAN_POINT ( 'NONE',  ( -11.88054826722768276, 25.79903810567671130, 3.000000000000000888 ) ) ;
#1944 = ORIENTED_EDGE ( 'NONE', *, *, #33891, .T. ) ;
#1945 = CARTESIAN_POINT ( 'NONE',  ( -13.63673279712320507, -0.1191753592594197858, 12.22739664767016521 ) ) ;
#1946 = LINE ( 'NONE', #36615, #45762 ) ;
#1948 = EDGE_CURVE ( 'NONE', #13435, #15529, #41937, .T. ) ;
#1947 = DIRECTION ( 'NONE',  ( 0.005002170337468016433, -0.7660444431189770143, -0.6427681459581293666 ) ) ;
#1949 = DIRECTION ( 'NONE',  ( 0.007781995580012663651, -3.146120232559066537E-19, -0.9999697198139514409 ) ) ;
#1950 = LINE ( 'NONE', #10784, #4659 ) ;
#1951 = DIRECTION ( 'NONE',  ( -0.7660212471507179544, -0.6427876096865405842, -0.005961354470445141482 ) ) ;
#1952 = CARTESIAN_POINT ( 'NONE',  ( -12.45966937092331861, -2.137015261443157677, 1.652897857657781522 ) ) ;
#1953 = DIRECTION ( 'NONE',  ( 0.005961354470445682716, -0.6427876096865404731, -0.7660212471507180654 ) ) ;
#1954 = EDGE_LOOP ( 'NONE', ( #7900, #50069, #40658, #38237 ) ) ;
#1955 = ORIENTED_EDGE ( 'NONE', *, *, #2128, .F. ) ;
#1956 = LINE ( 'NONE', #27849, #51338 ) ;
#1957 = CARTESIAN_POINT ( 'NONE',  ( -19.79569077582305070, 0.000000000000000000, 14.58012466630350445 ) ) ;
#1958 = AXIS2_PLACEMENT_3D ( 'NONE', #2173, #18379, #49628 ) ;
#1959 = VECTOR ( 'NONE', #888, 1000.000000000000227 ) ;
#1960 = ORIENTED_EDGE ( 'NONE', *, *, #23851, .F. ) ;
#1961 = CARTESIAN_POINT ( 'NONE',  ( -25.20278734466900517, 0.000000000000000000, 6.670939612111840944 ) ) ;
#1962 = ORIENTED_EDGE ( 'NONE', *, *, #49369, .T. ) ;
#1963 = LINE ( 'NONE', #10230, #31121 ) ;
#1964 = EDGE_LOOP ( 'NONE', ( #32203, #28848, #1655, #21035 ) ) ;
#1965 = ORIENTED_EDGE ( 'NONE', *, *, #43779, .F. ) ;
#1966 = VECTOR ( 'NONE', #50986, 1000.000000000000114 ) ;
#1967 = ORIENTED_EDGE ( 'NONE', *, *, #41514, .F. ) ;
#1968 = CARTESIAN_POINT ( 'NONE',  ( -15.93812677074078721, -0.1191753592594209099, 9.409283274482961090 ) ) ;
#1969 = LINE ( 'NONE', #2268, #2342 ) ;
#1970 = FACE_OUTER_BOUND ( 'NONE', #7950, .T. ) ;
#1971 = ADVANCED_FACE ( 'NONE', ( #24924 ), #8438, .F. ) ;
#1972 = EDGE_LOOP ( 'NONE', ( #41603, #54047, #31424, #43067 ) ) ;
#1973 = AXIS2_PLACEMENT_3D ( 'NONE', #13811, #48164, #17233 ) ;
#1974 = ORIENTED_EDGE ( 'NONE', *, *, #10264, .T. ) ;
#1975 = ADVANCED_FACE ( 'NONE', ( #34010 ), #25763, .F. ) ;
#1976 = ADVANCED_FACE ( 'NONE', ( #3348 ), #37712, .F. ) ;
#1977 = VECTOR ( 'NONE', #25078, 1000.000000000000227 ) ;
#1978 = LINE ( 'NONE', #14787, #34533 ) ;
#1979 = ORIENTED_EDGE ( 'NONE', *, *, #37264, .T. ) ;
#1980 = CARTESIAN_POINT ( 'NONE',  ( -27.06708303904391144, 0.000000000000000000, 7.395095371555332697 ) ) ;
#1981 = ORIENTED_EDGE ( 'NONE', *, *, #46750, .F. ) ;
#1982 = DIRECTION ( 'NONE',  ( -0.5449076811759708816, 0.6444004775717707689, 0.5364919789714475140 ) ) ;
#1983 = LINE ( 'NONE', #54796, #14941 ) ;
#1984 = ORIENTED_EDGE ( 'NONE', *, *, #34145, .F. ) ;
#1985 = LINE ( 'NONE', #22493, #38584 ) ;
#1986 = DIRECTION ( 'NONE',  ( 0.7660212471507180654, -0.6427876096865404731, 0.005961354470445141482 ) ) ;
#1987 = VERTEX_POINT ( 'NONE', #46789 ) ;
#1988 = CARTESIAN_POINT ( 'NONE',  ( -11.88054826722768276, 25.79903810567671130, 5.000000000000000000 ) ) ;
#1989 = LINE ( 'NONE', #6291, #26660 ) ;
#1990 = VECTOR ( 'NONE', #53920, 999.9999999999998863 ) ;
#1991 = CARTESIAN_POINT ( 'NONE',  ( -13.63673279712320507, -0.1191753592594197858, 12.22739664767016521 ) ) ;
#1992 = ORIENTED_EDGE ( 'NONE', *, *, #45850, .T. ) ;
#1993 = AXIS2_PLACEMENT_3D ( 'NONE', #42978, #47518, #29671 ) ;
#1994 = VECTOR ( 'NONE', #1166, 1000.000000000000227 ) ;
#1995 = DIRECTION ( 'NONE',  ( 0.000000000000000000, -1.000000000000000000, 0.000000000000000000 ) ) ;
#1996 = PLANE ( 'NONE',  #5144 ) ;
#1997 = CARTESIAN_POINT ( 'NONE',  ( -17.64587796725810165, 3.409179049219567048, 12.21456663636006468 ) ) ;
#1998 = LINE ( 'NONE', #38063, #24999 ) ;
#1999 = ADVANCED_FACE ( 'NONE', ( #38837 ), #42782, .F. ) ;
#2000 = LINE ( 'NONE', #22509, #23109 ) ;
#2001 = DIRECTION ( 'NONE',  ( -0.5364919789714478471, 0.6444004775717705469, -0.5449076811759709926 ) ) ;
#2002 = AXIS2_PLACEMENT_3D ( 'NONE', #16355, #46758, #25447 ) ;
#2003 = CARTESIAN_POINT ( 'NONE',  ( -66.84648059262940478, -9.494061817138627291, 1.387855868230217560 ) ) ;
#2004 = VECTOR ( 'NONE', #49455, 1000.000000000000227 ) ;
#2005 = ORIENTED_EDGE ( 'NONE', *, *, #22159, .T. ) ;
#2007 = EDGE_CURVE ( 'NONE', #47104, #36655, #15828, .T. ) ;
#2006 = CARTESIAN_POINT ( 'NONE',  ( -16.17100751540999681, 0.7721120973665049902, 2.938665801846358505 ) ) ;
#2008 = FACE_OUTER_BOUND ( 'NONE', #4329, .T. ) ;
#2009 = CARTESIAN_POINT ( 'NONE',  ( -68.06922484120158856, 4.336808689942017736E-15, -7.865887534729849584 ) ) ;
#2010 = VERTEX_POINT ( 'NONE', #20372 ) ;
#2011 = LINE ( 'NONE', #19346, #23865 ) ;
#2012 = CARTESIAN_POINT ( 'NONE',  ( 2.072287782118878319, 0.000000000000000000, -2.950529333540147015 ) ) ;
#2013 = EDGE_CURVE ( 'NONE', #9641, #50706, #51334, .T. ) ;
#2014 = DIRECTION ( 'NONE',  ( -0.9999697198139514409, -0.000000000000000000, -0.007781995580013368816 ) ) ;
#2015 = VECTOR ( 'NONE', #2440, 999.9999999999998863 ) ;
#2016 = LINE ( 'NONE', #49175, #30593 ) ;
#2017 = CARTESIAN_POINT ( 'NONE',  ( 2.072287782118878319, 0.000000000000000000, -2.950529333540147015 ) ) ;
#2018 = EDGE_LOOP ( 'NONE', ( #20058, #6656 ) ) ;
#2019 = ORIENTED_EDGE ( 'NONE', *, *, #43484, .F. ) ;
#2020 = CARTESIAN_POINT ( 'NONE',  ( -11.72912032238640556, -0.1191753592594190225, 5.937127636636843953 ) ) ;
#2021 = CARTESIAN_POINT ( 'NONE',  ( -14.93495759592298988, 0.000000000000000000, 12.77129166681078409 ) ) ;
#2022 = ORIENTED_EDGE ( 'NONE', *, *, #51670, .F. ) ;
#2023 = CARTESIAN_POINT ( 'NONE',  ( -69.46128946698341622, -9.665596887234965351, -7.502022462329921204 ) ) ;
#2024 = AXIS2_PLACEMENT_3D ( 'NONE', #25241, #11614, #24379 ) ;
#2025 = ORIENTED_EDGE ( 'NONE', *, *, #30562, .T. ) ;
#2026 = DIRECTION ( 'NONE',  ( 0.000000000000000000, 1.000000000000000000, 0.000000000000000000 ) ) ;
#2027 = EDGE_CURVE ( 'NONE', #28956, #29054, #50749, .T. ) ;
#2028 = VERTEX_POINT ( 'NONE', #46476 ) ;
#2029 = EDGE_LOOP ( 'NONE', ( #22916, #37565, #35525, #17878 ) ) ;
#2030 = CARTESIAN_POINT ( 'NONE',  ( -20.54049170961573267, 0.000000000000000000, 4.660556269540326646 ) ) ;
#2031 = CIRCLE ( 'NONE', #34679, 6.999999999999988454 ) ;
#2032 = EDGE_CURVE ( 'NONE', #36770, #46531, #37987, .T. ) ;
#2033 = CARTESIAN_POINT ( 'NONE',  ( -20.19095613468760320, 0.000000000000000000, 5.662415103335279198 ) ) ;
#2034 = CARTESIAN_POINT ( 'NONE',  ( -25.20123094555300369, 0.000000000000000000, 6.470945668149052032 ) ) ;
#2035 = ORIENTED_EDGE ( 'NONE', *, *, #5359, .T. ) ;
#2036 = VECTOR ( 'NONE', #18693, 1000.000000000000227 ) ;
#2037 = VECTOR ( 'NONE', #47569, 1000.000000000000227 ) ;
#2038 = LINE ( 'NONE', #2872, #4928 ) ;
#2039 = EDGE_CURVE ( 'NONE', #37913, #17469, #33705, .T. ) ;
#2040 = ORIENTED_EDGE ( 'NONE', *, *, #5282, .T. ) ;
#2041 = ADVANCED_FACE ( 'NONE', ( #7905 ), #29765, .F. ) ;
#2042 = VERTEX_POINT ( 'NONE', #25476 ) ;
#2043 = AXIS2_PLACEMENT_3D ( 'NONE', #54026, #36162, #6074 ) ;
#2044 = ORIENTED_EDGE ( 'NONE', *, *, #13964, .F. ) ;
#2045 = LINE ( 'NONE', #45489, #38592 ) ;
#2046 = VECTOR ( 'NONE', #9933, 1000.000000000000227 ) ;
#2047 = ORIENTED_EDGE ( 'NONE', *, *, #7137, .F. ) ;
#2048 = CARTESIAN_POINT ( 'NONE',  ( -24.27063949748155380, 0.000000000000000000, 6.308861732390097288 ) ) ;
#2049 = VERTEX_POINT ( 'NONE', #47061 ) ;
#2050 = LINE ( 'NONE', #10328, #54862 ) ;
#2051 = DIRECTION ( 'NONE',  ( -0.005961354470445682716, -0.6427876096865404731, 0.7660212471507180654 ) ) ;
#2052 = EDGE_CURVE ( 'NONE', #44744, #47896, #52708, .T. ) ;
#2053 = ORIENTED_EDGE ( 'NONE', *, *, #52670, .F. ) ;
#2055 = VECTOR ( 'NONE', #51107, 1000.000000000000227 ) ;
#2054 = DIRECTION ( 'NONE',  ( -0.7660212471507179544, -0.6427876096865405842, -0.005961354470445141482 ) ) ;
#2056 = ORIENTED_EDGE ( 'NONE', *, *, #49126, .T. ) ;
#2057 = VECTOR ( 'NONE', #31968, 1000.000000000000227 ) ;
#2058 = ADVANCED_FACE ( 'NONE', ( #763 ), #22630, .F. ) ;
#2059 = DIRECTION ( 'NONE',  ( -0.7660212471507179544, -0.6427876096865405842, -0.005961354470445141482 ) ) ;
#2060 = LINE ( 'NONE', #19393, #53805 ) ;
#2061 = DIRECTION ( 'NONE',  ( 0.005961354470445682716, -0.6427876096865404731, -0.7660212471507180654 ) ) ;
#2062 = PLANE ( 'NONE',  #51096 ) ;
#2063 = DIRECTION ( 'NONE',  ( 0.007781995580012662783, 0.000000000000000000, -0.9999697198139514409 ) ) ;
#2064 = LINE ( 'NONE', #40722, #15582 ) ;
#2065 = EDGE_LOOP ( 'NONE', ( #43818, #17178, #9439, #28162 ) ) ;
#2066 = AXIS2_PLACEMENT_3D ( 'NONE', #5631, #49655, #13868 ) ;
#2067 = EDGE_LOOP ( 'NONE', ( #37855, #52540, #10327, #27541 ) ) ;
#2068 = DIRECTION ( 'NONE',  ( -1.000000000000000000, 0.000000000000000000, 0.000000000000000000 ) ) ;
#2069 = LINE ( 'NONE', #29330, #9466 ) ;
#2070 = VECTOR ( 'NONE', #39496, 1000.000000000000227 ) ;
#2071 = CARTESIAN_POINT ( 'NONE',  ( -13.17065887352947762, -0.1191753592594197858, 12.04635770780929427 ) ) ;
#2072 = LINE ( 'NONE', #33035, #26965 ) ;
#2073 = DIRECTION ( 'NONE',  ( -0.005961354470445682716, -0.6427876096865404731, 0.7660212471507180654 ) ) ;
#2074 = ORIENTED_EDGE ( 'NONE', *, *, #27339, .T. ) ;
#2075 = FACE_OUTER_BOUND ( 'NONE', #2430, .T. ) ;
#2076 = PLANE ( 'NONE',  #26868 ) ;
#2077 = ORIENTED_EDGE ( 'NONE', *, *, #16674, .T. ) ;
#2079 = DIRECTION ( 'NONE',  ( 0.007781995580012663651, -3.146120232559066537E-19, -0.9999697198139514409 ) ) ;
#2078 = AXIS2_PLACEMENT_3D ( 'NONE', #1703, #6268, #15329 ) ;
#2080 = DIRECTION ( 'NONE',  ( 0.000000000000000000, -0.000000000000000000, -1.000000000000000000 ) ) ;
#2081 = EDGE_LOOP ( 'NONE', ( #41452, #25307, #16223, #11978 ) ) ;
#2082 = AXIS2_PLACEMENT_3D ( 'NONE', #20184, #45027, #27133 ) ;
#2083 = VECTOR ( 'NONE', #15039, 1000.000000000000227 ) ;
#2084 = CARTESIAN_POINT ( 'NONE',  ( -13.52026565332740482, -1.165603555308156736, 3.846616072963900290 ) ) ;
#2085 = LINE ( 'NONE', #48971, #39656 ) ;
#2086 = EDGE_CURVE ( 'NONE', #51694, #9097, #27167, .T. ) ;
#2087 = CARTESIAN_POINT ( 'NONE',  ( -18.67775241435682432, 0.000000000000000000, 4.136394454059623804 ) ) ;
#2088 = FACE_OUTER_BOUND ( 'NONE', #24345, .T. ) ;
#2089 = DIRECTION ( 'NONE',  ( 0.007781995580012662783, 0.000000000000000000, -0.9999697198139514409 ) ) ;
#2090 = ORIENTED_EDGE ( 'NONE', *, *, #30344, .F. ) ;
#2091 = VECTOR ( 'NONE', #34344, 1000.000000000000000 ) ;
#2092 = AXIS2_PLACEMENT_3D ( 'NONE', #14288, #27307, #5459 ) ;
#2093 = ORIENTED_EDGE ( 'NONE', *, *, #49879, .T. ) ;
#2094 = FACE_OUTER_BOUND ( 'NONE', #7215, .T. ) ;
#2095 = PLANE ( 'NONE',  #55793 ) ;
#2096 = LINE ( 'NONE', #1819, #46032 ) ;
#2097 = ADVANCED_FACE ( 'NONE', ( #39937 ), #56149, .F. ) ;
#2098 = LINE ( 'NONE', #5833, #41850 ) ;
#2099 = DIRECTION ( 'NONE',  ( -0.005961354470445682716, -0.6427876096865404731, 0.7660212471507180654 ) ) ;
#2101 = EDGE_CURVE ( 'NONE', #3819, #47757, #26066, .T. ) ;
#2100 = EDGE_LOOP ( 'NONE', ( #22012, #1505, #24804, #48534 ) ) ;
#2103 = AXIS2_PLACEMENT_3D ( 'NONE', #41336, #54640, #24002 ) ;
#2102 = DIRECTION ( 'NONE',  ( 0.000000000000000000, -0.000000000000000000, -1.000000000000000000 ) ) ;
#2104 = EDGE_CURVE ( 'NONE', #31339, #2694, #170, .T. ) ;
#2105 = DIRECTION ( 'NONE',  ( -0.005002170337468016433, -0.7660444431189770143, 0.6427681459581293666 ) ) ;
#2106 = DIRECTION ( 'NONE',  ( 0.9999697198139515519, 0.000000000000000000, 0.007781995580013368816 ) ) ;
#2107 = EDGE_LOOP ( 'NONE', ( #47687, #15501, #17139, #35280 ) ) ;
#2108 = DIRECTION ( 'NONE',  ( 0.7660212471507180654, -0.6427876096865404731, 0.005961354470445141482 ) ) ;
#2109 = EDGE_LOOP ( 'NONE', ( #6, #16158, #21082, #50793 ) ) ;
#2110 = DIRECTION ( 'NONE',  ( 0.7660212471507180654, -0.6427876096865404731, 0.005961354470445141482 ) ) ;
#2111 = VECTOR ( 'NONE', #48952, 1000.000000000000000 ) ;
#2112 = DIRECTION ( 'NONE',  ( -0.6427681459581293666, -0.7660444431189770143, -0.005002170337467561935 ) ) ;
#2113 = ORIENTED_EDGE ( 'NONE', *, *, #38991, .T. ) ;
#2114 = PLANE ( 'NONE',  #54024 ) ;
#2115 = EDGE_CURVE ( 'NONE', #42375, #18224, #18351, .T. ) ;
#2116 = VECTOR ( 'NONE', #43468, 999.9999999999998863 ) ;
#2117 = EDGE_LOOP ( 'NONE', ( #22976, #10330, #5618, #19865 ) ) ;
#2118 = ADVANCED_FACE ( 'NONE', ( #9273 ), #43914, .F. ) ;
#2119 = ORIENTED_EDGE ( 'NONE', *, *, #8292, .T. ) ;
#2120 = EDGE_LOOP ( 'NONE', ( #29756, #40103, #54588, #22343 ) ) ;
#2121 = CARTESIAN_POINT ( 'NONE',  ( -29.26563357085082728, 15.76175442574525043, 4.734210823084358921 ) ) ;
#2122 = ORIENTED_EDGE ( 'NONE', *, *, #28360, .F. ) ;
#2123 = ORIENTED_EDGE ( 'NONE', *, *, #25714, .T. ) ;
#2124 = VECTOR ( 'NONE', #55210, 999.9999999999998863 ) ;
#2125 = LINE ( 'NONE', #18923, #2057 ) ;
#2126 = VERTEX_POINT ( 'NONE', #53007 ) ;
#2127 = VECTOR ( 'NONE', #54884, 1000.000000000000114 ) ;
#2128 = EDGE_CURVE ( 'NONE', #29102, #17107, #31140, .T. ) ;
#2129 = VECTOR ( 'NONE', #43312, 1000.000000000000227 ) ;
#2130 = ORIENTED_EDGE ( 'NONE', *, *, #10800, .T. ) ;
#2131 = LINE ( 'NONE', #19175, #54850 ) ;
#2132 = VERTEX_POINT ( 'NONE', #9013 ) ;
#2133 = ORIENTED_EDGE ( 'NONE', *, *, #18160, .T. ) ;
#2134 = ORIENTED_EDGE ( 'NONE', *, *, #35473, .T. ) ;
#2135 = EDGE_CURVE ( 'NONE', #54647, #50938, #44472, .T. ) ;
#2136 = AXIS2_PLACEMENT_3D ( 'NONE', #23823, #10785, #54760 ) ;
#2137 = VECTOR ( 'NONE', #13624, 1000.000000000000227 ) ;
#2138 = DIRECTION ( 'NONE',  ( 0.5449076811759707706, 0.6444004775717708799, -0.5364919789714476250 ) ) ;
#2139 = PLANE ( 'NONE',  #29403 ) ;
#2140 = LINE ( 'NONE', #53003, #45922 ) ;
#2141 = CARTESIAN_POINT ( 'NONE',  ( -24.26908309836554878, 0.000000000000000000, 6.108867788427308376 ) ) ;
#2142 = VERTEX_POINT ( 'NONE', #17518 ) ;
#2143 = DIRECTION ( 'NONE',  ( 0.007781995580012663651, 0.000000000000000000, -0.9999697198139515519 ) ) ;
#2144 = ORIENTED_EDGE ( 'NONE', *, *, #3036, .F. ) ;
#2145 = EDGE_LOOP ( 'NONE', ( #7055, #3714, #30518, #47275 ) ) ;
#2146 = DIRECTION ( 'NONE',  ( 0.6427681459581294776, -0.7660444431189769032, 0.005002170337467562802 ) ) ;
#2147 = PLANE ( 'NONE',  #40587 ) ;
#2148 = LINE ( 'NONE', #19485, #38495 ) ;
#2149 = VECTOR ( 'NONE', #50327, 999.9999999999998863 ) ;
#2150 = LINE ( 'NONE', #6437, #21219 ) ;
#2151 = DIRECTION ( 'NONE',  ( -0.3620778797217455991, 0.000000000000000000, -0.9321478471874540261 ) ) ;
#2152 = ORIENTED_EDGE ( 'NONE', *, *, #43562, .F. ) ;
#2153 = DIRECTION ( 'NONE',  ( -0.005961354470445682716, -0.6427876096865404731, 0.7660212471507180654 ) ) ;
#2154 = AXIS2_PLACEMENT_3D ( 'NONE', #49605, #44224, #2146 ) ;
#2155 = EDGE_LOOP ( 'NONE', ( #4127, #53544, #41314, #16182 ) ) ;
#2156 = DIRECTION ( 'NONE',  ( 0.9999697198139515519, 0.000000000000000000, 0.007781995580013368816 ) ) ;
#2157 = LINE ( 'NONE', #10435, #45918 ) ;
#2158 = DIRECTION ( 'NONE',  ( 0.7660212471507180654, -0.6427876096865404731, 0.005961354470445141482 ) ) ;
#2159 = ADVANCED_FACE ( 'NONE', ( #4738 ), #47629, .F. ) ;
#2160 = VECTOR ( 'NONE', #24632, 999.9999999999998863 ) ;
#2161 = CARTESIAN_POINT ( 'NONE',  ( -16.99924723426068951, 0.000000000000000000, 13.49389102713827171 ) ) ;
#2162 = CARTESIAN_POINT ( 'NONE',  ( -12.27285761711391032, 0.000000000000000000, 3.247568630525088818 ) ) ;
#2163 = EDGE_CURVE ( 'NONE', #40212, #12044, #48461, .T. ) ;
#2164 = ORIENTED_EDGE ( 'NONE', *, *, #19730, .T. ) ;
#2165 = AXIS2_PLACEMENT_3D ( 'NONE', #34407, #30138, #47456 ) ;
#2166 = CARTESIAN_POINT ( 'NONE',  ( -19.16420072258311436, -0.6798977022406551551, 5.241786070853162727 ) ) ;
#2167 = CARTESIAN_POINT ( 'NONE',  ( -13.73672976910459909, 0.000000000000000000, 12.22661844811216270 ) ) ;
#2168 = DIRECTION ( 'NONE',  ( -0.5449076811759708816, 0.6444004775717707689, 0.5364919789714475140 ) ) ;
#2169 = EDGE_CURVE ( 'NONE', #13325, #33916, #33726, .T. ) ;
#2170 = ADVANCED_FACE ( 'NONE', ( #13282 ), #9863, .F. ) ;
#2171 = EDGE_CURVE ( 'NONE', #33602, #55501, #5321, .T. ) ;
#2172 = VECTOR ( 'NONE', #7976, 1000.000000000000114 ) ;
#2173 = CARTESIAN_POINT ( 'NONE',  ( -22.40478740399063895, 0.000000000000000000, 5.384712028983816623 ) ) ;
#2174 = PLANE ( 'NONE',  #43896 ) ;
#2175 = CARTESIAN_POINT ( 'NONE',  ( -18.67697421479882181, -0.1191753592594197858, 4.036397482078229793 ) ) ;
#2176 = LINE ( 'NONE', #15263, #34685 ) ;
#2177 = ADVANCED_FACE ( 'NONE', ( #47913 ), #22059, .F. ) ;
#2178 = VECTOR ( 'NONE', #1638, 999.9999999999998863 ) ;
#2179 = VECTOR ( 'NONE', #10973, 999.9999999999998863 ) ;
#2180 = DIRECTION ( 'NONE',  ( -0.9321478471874540261, 0.000000000000000000, 0.3620778797217457656 ) ) ;
#2181 = DIRECTION ( 'NONE',  ( 0.5449076811759707706, 0.6444004775717708799, -0.5364919789714476250 ) ) ;
#2182 = EDGE_LOOP ( 'NONE', ( #18550, #14027, #27487, #4916, #1801 ) ) ;
#2183 = EDGE_CURVE ( 'NONE', #11699, #42663, #13547, .T. ) ;
#2184 = EDGE_CURVE ( 'NONE', #38162, #8156, #45882, .T. ) ;
#2185 = AXIS2_PLACEMENT_3D ( 'NONE', #45061, #6168, #53305 ) ;
#2186 = ORIENTED_EDGE ( 'NONE', *, *, #25414, .T. ) ;
#2187 = VERTEX_POINT ( 'NONE', #15481 ) ;
#2188 = ORIENTED_EDGE ( 'NONE', *, *, #4643, .F. ) ;
#2189 = EDGE_CURVE ( 'NONE', #44901, #31339, #6173, .T. ) ;
#2190 = ORIENTED_EDGE ( 'NONE', *, *, #32674, .T. ) ;
#2191 = LINE ( 'NONE', #31758, #34148 ) ;
#2192 = DIRECTION ( 'NONE',  ( -0.6427681459581293666, -0.7660444431189770143, -0.005002170337467561935 ) ) ;
#2193 = VECTOR ( 'NONE', #958, 999.9999999999998863 ) ;
#2194 = EDGE_CURVE ( 'NONE', #33225, #40269, #49301, .T. ) ;
#2195 = ORIENTED_EDGE ( 'NONE', *, *, #43381, .T. ) ;
#2196 = DIRECTION ( 'NONE',  ( 0.5364919789714477361, 0.6444004775717706579, 0.5449076811759711036 ) ) ;
#2197 = ORIENTED_EDGE ( 'NONE', *, *, #42916, .F. ) ;
#2198 = ORIENTED_EDGE ( 'NONE', *, *, #35348, .F. ) ;
#2199 = AXIS2_PLACEMENT_3D ( 'NONE', #5585, #30619, #14130 ) ;
#2200 = CARTESIAN_POINT ( 'NONE',  ( -68.38969147407715354, -8.931796914766161777, -6.479403174773509910 ) ) ;
#2201 = VECTOR ( 'NONE', #17876, 1000.000000000000227 ) ;
#2202 = DIRECTION ( 'NONE',  ( 0.9999697198139515519, 0.000000000000000000, 0.007781995580013368816 ) ) ;
#2203 = CARTESIAN_POINT ( 'NONE',  ( -19.25103323024604052, 0.000000000000000000, 4.301259063778239522 ) ) ;
#2204 = ORIENTED_EDGE ( 'NONE', *, *, #17300, .T. ) ;
#2205 = CARTESIAN_POINT ( 'NONE',  ( -13.00213746683328964, 0.000000000000000000, 3.241893206105073144 ) ) ;
#2206 = VECTOR ( 'NONE', #38846, 999.9999999999998863 ) ;
#2207 = DIRECTION ( 'NONE',  ( 0.5449076811759707706, 0.6444004775717708799, -0.5364919789714476250 ) ) ;
#2208 = FACE_OUTER_BOUND ( 'NONE', #20967, .T. ) ;
#2209 = VECTOR ( 'NONE', #45024, 1000.000000000000114 ) ;
#2210 = DIRECTION ( 'NONE',  ( -0.5449076811759708816, 0.6444004775717707689, 0.5364919789714475140 ) ) ;
#2211 = PLANE ( 'NONE',  #3368 ) ;
#2212 = AXIS2_PLACEMENT_3D ( 'NONE', #3387, #41454, #36924 ) ;
#2213 = CARTESIAN_POINT ( 'NONE',  ( -46.28406441860501985, 5.387676038879166462, 5.000000000000000000 ) ) ;
#2214 = DIRECTION ( 'NONE',  ( -0.7660212471507179544, -0.6427876096865405842, -0.005961354470445141482 ) ) ;
#2215 = CARTESIAN_POINT ( 'NONE',  ( -0.9971735401232131313, -6.078073896745635807, 3.605709642803621939 ) ) ;
#2216 = CARTESIAN_POINT ( 'NONE',  ( -16.32763152475235913, 5.305366725996512045, 11.93053833287189747 ) ) ;
#2217 = ORIENTED_EDGE ( 'NONE', *, *, #55126, .F. ) ;
#2218 = CARTESIAN_POINT ( 'NONE',  ( -10.37421533196711465, -0.1191753592594197858, 10.96012406864405975 ) ) ;
#2219 = ORIENTED_EDGE ( 'NONE', *, *, #45835, .F. ) ;
#2220 = ADVANCED_FACE ( 'NONE', ( #14946 ), #5877, .F. ) ;
#2221 = LINE ( 'NONE', #19563, #29258 ) ;
#2222 = FACE_OUTER_BOUND ( 'NONE', #39220, .T. ) ;
#2223 = FACE_OUTER_BOUND ( 'NONE', #4457, .T. ) ;
#2224 = DIRECTION ( 'NONE',  ( -0.5449076811759708816, 0.6444004775717707689, 0.5364919789714475140 ) ) ;
#2225 = ADVANCED_FACE ( 'NONE', ( #41351 ), #11231, .F. ) ;
#2226 = CARTESIAN_POINT ( 'NONE',  ( -8.061453912371437269, -7.756624998024296502, -0.08703110797150630240 ) ) ;
#2227 = CARTESIAN_POINT ( 'NONE',  ( -19.60990026154428278, 0.000000000000000000, 4.498472333781370125 ) ) ;
#2228 = VECTOR ( 'NONE', #20101, 999.9999999999998863 ) ;
#2229 = DIRECTION ( 'NONE',  ( 0.9999697198139515519, 0.000000000000000000, 0.007781995580013368816 ) ) ;
#2230 = DIRECTION ( 'NONE',  ( 0.9998863659938501680, -0.01507498257419588941, 1.340073885192090777E-15 ) ) ;
#2231 = VECTOR ( 'NONE', #47775, 1000.000000000000114 ) ;
#2232 = DIRECTION ( 'NONE',  ( 0.005961354470445682716, -0.6427876096865404731, -0.7660212471507180654 ) ) ;
#2233 = DIRECTION ( 'NONE',  ( 0.000000000000000000, -1.000000000000000000, 0.000000000000000000 ) ) ;
#2234 = DIRECTION ( 'NONE',  ( -0.5449076811759708816, 0.6444004775717707689, 0.5364919789714475140 ) ) ;
#2235 = CARTESIAN_POINT ( 'NONE',  ( -69.83802984922479595, -1.000000000000000666, -7.175319846998989171 ) ) ;
#2236 = VECTOR ( 'NONE', #48621, 999.9999999999998863 ) ;
#2237 = EDGE_CURVE ( 'NONE', #29513, #1224, #14661, .T. ) ;
#2238 = DIRECTION ( 'NONE',  ( 0.9999697198139515519, 0.000000000000000000, 0.007781995580013368816 ) ) ;
#2239 = EDGE_CURVE ( 'NONE', #19378, #19054, #36516, .T. ) ;
#2240 = EDGE_CURVE ( 'NONE', #3565, #2953, #31981, .T. ) ;
#2241 = DIRECTION ( 'NONE',  ( 0.9999697198139515519, 0.000000000000000000, 0.007781995580013368816 ) ) ;
#2242 = AXIS2_PLACEMENT_3D ( 'NONE', #38054, #38321, #55953 ) ;
#2243 = DIRECTION ( 'NONE',  ( 0.007781995580012663651, 0.000000000000000000, -0.9999697198139515519 ) ) ;
#2244 = EDGE_CURVE ( 'NONE', #32088, #34543, #40225, .T. ) ;
#2245 = FACE_OUTER_BOUND ( 'NONE', #33427, .T. ) ;
#2246 = DIRECTION ( 'NONE',  ( 0.005002170337468016433, -0.7660444431189770143, -0.6427681459581293666 ) ) ;
#2247 = ORIENTED_EDGE ( 'NONE', *, *, #39992, .T. ) ;
#2248 = FACE_OUTER_BOUND ( 'NONE', #43148, .T. ) ;
#2249 = VECTOR ( 'NONE', #33727, 1000.000000000000227 ) ;
#2250 = VECTOR ( 'NONE', #24711, 999.9999999999998863 ) ;
#2251 = ORIENTED_EDGE ( 'NONE', *, *, #8873, .T. ) ;
#2252 = PLANE ( 'NONE',  #47739 ) ;
#2253 = VECTOR ( 'NONE', #43903, 1000.000000000000000 ) ;
#2254 = DIRECTION ( 'NONE',  ( 0.6427681459581294776, -0.7660444431189769032, 0.005002170337467562802 ) ) ;
#2255 = AXIS2_PLACEMENT_3D ( 'NONE', #15107, #33523, #11926 ) ;
#2256 = ORIENTED_EDGE ( 'NONE', *, *, #53680, .F. ) ;
#2257 = CARTESIAN_POINT ( 'NONE',  ( -12.92993527630429185, 1.905425754524006532, 1.643564637689428620 ) ) ;
#2258 = ORIENTED_EDGE ( 'NONE', *, *, #4489, .T. ) ;
#2259 = CARTESIAN_POINT ( 'NONE',  ( 5.541166327321979779, -1.059169997729283441, -2.374049323224325825 ) ) ;
#2260 = EDGE_CURVE ( 'NONE', #16010, #10235, #23730, .T. ) ;
#2261 = VECTOR ( 'NONE', #14306, 1000.000000000000114 ) ;
#2262 = VERTEX_POINT ( 'NONE', #19763 ) ;
#2263 = VECTOR ( 'NONE', #21465, 1000.000000000000227 ) ;
#2264 = ORIENTED_EDGE ( 'NONE', *, *, #8457, .F. ) ;
#2265 = ORIENTED_EDGE ( 'NONE', *, *, #22264, .T. ) ;
#2266 = EDGE_CURVE ( 'NONE', #42909, #30703, #14404, .T. ) ;
#2267 = DIRECTION ( 'NONE',  ( -0.005002170337468016433, -0.7660444431189770143, 0.6427681459581293666 ) ) ;
#2268 = CARTESIAN_POINT ( 'NONE',  ( -10.15248364251277913, -0.02656858173836865178, 0.8564570764427139604 ) ) ;
#2269 = FACE_OUTER_BOUND ( 'NONE', #13609, .T. ) ;
#2270 = EDGE_CURVE ( 'NONE', #25263, #29020, #1311, .T. ) ;
#2271 = ORIENTED_EDGE ( 'NONE', *, *, #27435, .T. ) ;
#2272 = ORIENTED_EDGE ( 'NONE', *, *, #5337, .F. ) ;
#2273 = ADVANCED_FACE ( 'NONE', ( #19186 ), #53834, .F. ) ;
#2274 = VECTOR ( 'NONE', #50073, 1000.000000000000227 ) ;
#2275 = LINE ( 'NONE', #45710, #1887 ) ;
#2276 = VECTOR ( 'NONE', #2196, 999.9999999999998863 ) ;
#2277 = ORIENTED_EDGE ( 'NONE', *, *, #28600, .T. ) ;
#2278 = FACE_OUTER_BOUND ( 'NONE', #17971, .T. ) ;
#2279 = VERTEX_POINT ( 'NONE', #45320 ) ;
#2280 = AXIS2_PLACEMENT_3D ( 'NONE', #43032, #43862, #39635 ) ;
#2281 = CARTESIAN_POINT ( 'NONE',  ( 5.561339567967533704, -1.056856647418703776, 2.400892578144001366 ) ) ;
#2282 = DIRECTION ( 'NONE',  ( -0.5449076811759708816, 0.6444004775717707689, 0.5364919789714475140 ) ) ;
#2283 = ORIENTED_EDGE ( 'NONE', *, *, #11508, .F. ) ;
#2284 = DIRECTION ( 'NONE',  ( -0.5449076811759708816, 0.6444004775717707689, 0.5364919789714475140 ) ) ;
#2285 = VECTOR ( 'NONE', #16986, 1000.000000000000227 ) ;
#2286 = PLANE ( 'NONE',  #5528 ) ;
#2287 = VECTOR ( 'NONE', #6286, 1000.000000000000227 ) ;
#2288 = VECTOR ( 'NONE', #24226, 999.9999999999998863 ) ;
#2289 = VERTEX_POINT ( 'NONE', #41052 ) ;
#2290 = FACE_OUTER_BOUND ( 'NONE', #31705, .T. ) ;
#2291 = DIRECTION ( 'NONE',  ( -0.8531650599175529814, -0.4028455766673920135, 0.3313982828793697877 ) ) ;
#2292 = CARTESIAN_POINT ( 'NONE',  ( -29.86197018149027116, 0.000000000000000000, 8.281335066757780083 ) ) ;
#2293 = EDGE_LOOP ( 'NONE', ( #35221, #36493, #16059, #46308 ) ) ;
#2294 = VECTOR ( 'NONE', #54153, 999.9999999999998863 ) ;
#2295 = VECTOR ( 'NONE', #34920, 999.9999999999998863 ) ;
#2296 = PLANE ( 'NONE',  #21068 ) ;
#2297 = CARTESIAN_POINT ( 'NONE',  ( -12.60458797795435615, 0.000000000000000000, 11.86609696750642229 ) ) ;
#2298 = CARTESIAN_POINT ( 'NONE',  ( -21.04994044461160740, -3.432230869623158487, 10.49131904603741816 ) ) ;
#2299 = CARTESIAN_POINT ( 'NONE',  ( 2.072287782118878319, 0.000000000000000000, -2.950529333540147015 ) ) ;
#2300 = CARTESIAN_POINT ( 'NONE',  ( -12.71165780605550211, -2.946525016555658905, 6.455320848100502218 ) ) ;
#2301 = DIRECTION ( 'NONE',  ( 0.9999697198139515519, 0.000000000000000000, 0.007781995580013368816 ) ) ;
#2302 = VECTOR ( 'NONE', #13178, 999.9999999999998863 ) ;
#2303 = VECTOR ( 'NONE', #26760, 1000.000000000000114 ) ;
#2304 = CARTESIAN_POINT ( 'NONE',  ( -67.75769695306428275, -11.47776601246343375, 8.850418579662749252 ) ) ;
#2305 = VERTEX_POINT ( 'NONE', #18936 ) ;
#2306 = DIRECTION ( 'NONE',  ( 0.007781995580012663651, -3.146120232559066537E-19, -0.9999697198139514409 ) ) ;
#2307 = DIRECTION ( 'NONE',  ( 0.000000000000000000, -0.000000000000000000, -1.000000000000000000 ) ) ;
#2308 = CARTESIAN_POINT ( 'NONE',  ( -66.48098233065147156, 7.155734338404329264E-14, -4.848827299331423646 ) ) ;
#2309 = VERTEX_POINT ( 'NONE', #40531 ) ;
#2310 = CARTESIAN_POINT ( 'NONE',  ( 2.072287782118878319, 0.000000000000000000, -2.950529333540147015 ) ) ;
#2311 = PLANE ( 'NONE',  #19096 ) ;
#2312 = EDGE_CURVE ( 'NONE', #32666, #3230, #31717, .T. ) ;
#2313 = DIRECTION ( 'NONE',  ( 0.007781995580012663651, -3.146120232559066537E-19, -0.9999697198139514409 ) ) ;
#2314 = EDGE_CURVE ( 'NONE', #9006, #32397, #19475, .T. ) ;
#2315 = EDGE_CURVE ( 'NONE', #54422, #24558, #36818, .T. ) ;
#2316 = CARTESIAN_POINT ( 'NONE',  ( -14.01623497886155256, -0.1191753592594197858, 2.226008083469502630 ) ) ;
#2317 = LINE ( 'NONE', #27614, #44686 ) ;
#2318 = VECTOR ( 'NONE', #9380, 999.9999999999998863 ) ;
#2319 = ORIENTED_EDGE ( 'NONE', *, *, #30602, .T. ) ;
#2320 = VERTEX_POINT ( 'NONE', #32550 ) ;
#2321 = VECTOR ( 'NONE', #48092, 1000.000000000000114 ) ;
#2322 = CARTESIAN_POINT ( 'NONE',  ( -24.26908309836554878, 0.000000000000000000, 6.108867788427308376 ) ) ;
#2323 = VECTOR ( 'NONE', #41289, 999.9999999999998863 ) ;
#2324 = CARTESIAN_POINT ( 'NONE',  ( -18.24265903867745919, -0.1191753592594168992, 6.994433981658000121 ) ) ;
#2325 = ORIENTED_EDGE ( 'NONE', *, *, #1723, .T. ) ;
#2326 = CARTESIAN_POINT ( 'NONE',  ( -28.93060053386082231, -0.1191753592594197858, 8.019254159017428663 ) ) ;
#2327 = VECTOR ( 'NONE', #19336, 1000.000000000000114 ) ;
#2328 = VERTEX_POINT ( 'NONE', #10951 ) ;
#2329 = DIRECTION ( 'NONE',  ( 0.007781995580012663651, -3.146120232559066537E-19, -0.9999697198139514409 ) ) ;
#2330 = VECTOR ( 'NONE', #30164, 999.9999999999998863 ) ;
#2331 = ORIENTED_EDGE ( 'NONE', *, *, #41111, .F. ) ;
#2332 = ORIENTED_EDGE ( 'NONE', *, *, #33090, .F. ) ;
#2333 = CARTESIAN_POINT ( 'NONE',  ( -10.77972815416725894, -0.1191753592594185784, 3.359191537368509728 ) ) ;
#2334 = LINE ( 'NONE', #44955, #15973 ) ;
#2335 = CARTESIAN_POINT ( 'NONE',  ( -14.94838282604900748, -0.1191753592594197858, 2.588085963191248506 ) ) ;
#2336 = VECTOR ( 'NONE', #43038, 999.9999999999998863 ) ;
#2337 = EDGE_LOOP ( 'NONE', ( #55218, #651, #33952, #27378 ) ) ;
#2338 = VECTOR ( 'NONE', #44819, 999.9999999999998863 ) ;
#2339 = DIRECTION ( 'NONE',  ( 0.007781995580012663651, -3.146120232559066537E-19, -0.9999697198139514409 ) ) ;
#2340 = ORIENTED_EDGE ( 'NONE', *, *, #7096, .F. ) ;
#2341 = ADVANCED_FACE ( 'NONE', ( #41611 ), #7836, .F. ) ;
#2342 = VECTOR ( 'NONE', #53666, 1000.000000000000114 ) ;
#2343 = EDGE_LOOP ( 'NONE', ( #38952, #30792, #45064, #46395 ) ) ;
#2344 = VECTOR ( 'NONE', #45609, 1000.000000000000000 ) ;
#2345 = VERTEX_POINT ( 'NONE', #12060 ) ;
#2346 = DIRECTION ( 'NONE',  ( 0.5449076811759707706, 0.6444004775717708799, -0.5364919789714476250 ) ) ;
#2347 = ADVANCED_FACE ( 'NONE', ( #50693 ), #2693, .F. ) ;
#2348 = ORIENTED_EDGE ( 'NONE', *, *, #44025, .T. ) ;
#2349 = PLANE ( 'NONE',  #13952 ) ;
#2350 = ORIENTED_EDGE ( 'NONE', *, *, #40253, .F. ) ;
#2351 = LINE ( 'NONE', #45241, #7733 ) ;
#2352 = DIRECTION ( 'NONE',  ( -0.5364919789714478471, 0.6444004775717705469, -0.5449076811759709926 ) ) ;
#2353 = ORIENTED_EDGE ( 'NONE', *, *, #52080, .T. ) ;
#2354 = ADVANCED_FACE ( 'NONE', ( #33638 ), #11782, .F. ) ;
#2355 = CARTESIAN_POINT ( 'NONE',  ( -15.60102546347950536, 0.000000000000000000, 12.95077420755565356 ) ) ;
#2356 = EDGE_LOOP ( 'NONE', ( #53429, #41604, #29760, #51916 ) ) ;
#2357 = VECTOR ( 'NONE', #19289, 1000.000000000000227 ) ;
#2358 = LINE ( 'NONE', #15412, #4721 ) ;
#2359 = CARTESIAN_POINT ( 'NONE',  ( -20.54049170961573267, 0.000000000000000000, 4.660556269540326646 ) ) ;
#2360 = DIRECTION ( 'NONE',  ( -0.6427681459581293666, -0.7660444431189770143, -0.005002170337467561935 ) ) ;
#2361 = FACE_OUTER_BOUND ( 'NONE', #24008, .T. ) ;
#2362 = DIRECTION ( 'NONE',  ( -0.7660212471507179544, -0.6427876096865405842, -0.005961354470445141482 ) ) ;
#2363 = LINE ( 'NONE', #17826, #17373 ) ;
#2364 = CARTESIAN_POINT ( 'NONE',  ( -19.25546368286732601, 0.000000000000000000, 4.870562710998793676 ) ) ;
#2365 = AXIS2_PLACEMENT_3D ( 'NONE', #3828, #16925, #51554 ) ;
#2366 = ORIENTED_EDGE ( 'NONE', *, *, #16292, .T. ) ;
#2367 = VERTEX_POINT ( 'NONE', #47001 ) ;
#2368 = DIRECTION ( 'NONE',  ( 0.6427681459581294776, -0.7660444431189769032, 0.005002170337467562802 ) ) ;
#2369 = CARTESIAN_POINT ( 'NONE',  ( -68.38638472608106156, -9.332867493602380549, 7.478321023991166605 ) ) ;
#2370 = VECTOR ( 'NONE', #45386, 999.9999999999998863 ) ;
#2371 = DIRECTION ( 'NONE',  ( -0.5364919789714478471, 0.6444004775717705469, -0.5449076811759709926 ) ) ;
#2372 = CARTESIAN_POINT ( 'NONE',  ( -17.93139508144814442, 0.000000000000000000, 13.85596890686001537 ) ) ;
#2373 = VECTOR ( 'NONE', #13068, 999.9999999999998863 ) ;
#2374 = VECTOR ( 'NONE', #13671, 1000.000000000000000 ) ;
#2375 = DIRECTION ( 'NONE',  ( 0.005002170337468016433, -0.7660444431189770143, -0.6427681459581293666 ) ) ;
#2376 = VERTEX_POINT ( 'NONE', #16604 ) ;
#2377 = CARTESIAN_POINT ( 'NONE',  ( -19.06773268699349799, 2.553033558614008047, 4.007031512929001948 ) ) ;
#2378 = DIRECTION ( 'NONE',  ( -0.7660212471507179544, -0.6427876096865405842, -0.005961354470445141482 ) ) ;
#2379 = ORIENTED_EDGE ( 'NONE', *, *, #46707, .F. ) ;
#2380 = DIRECTION ( 'NONE',  ( -0.9999697198139514409, -0.000000000000000000, -0.007781995580013368816 ) ) ;
#2381 = EDGE_CURVE ( 'NONE', #33688, #5490, #37341, .T. ) ;
#2382 = CARTESIAN_POINT ( 'NONE',  ( -13.27065584551087163, 0.000000000000000000, 12.04557950825129176 ) ) ;
#2383 = EDGE_LOOP ( 'NONE', ( #27741, #52301, #35795, #41586, #3485 ) ) ;
#2384 = VECTOR ( 'NONE', #45879, 999.9999999999998863 ) ;
#2385 = EDGE_CURVE ( 'NONE', #30192, #45499, #7253, .T. ) ;
#2386 = CARTESIAN_POINT ( 'NONE',  ( -70.71258200891328727, -0.9999999999999995559, 8.208045577613541255 ) ) ;
#2387 = DIRECTION ( 'NONE',  ( 0.7660212471507180654, -0.6427876096865404731, 0.005961354470445141482 ) ) ;
#2388 = AXIS2_PLACEMENT_3D ( 'NONE', #29323, #46637, #20534 ) ;
#2389 = LINE ( 'NONE', #19717, #5975 ) ;
#2390 = ADVANCED_FACE ( 'NONE', ( #16910 ), #55498, .F. ) ;
#2391 = CARTESIAN_POINT ( 'NONE',  ( -24.27063949748155380, 0.000000000000000000, 6.308861732390097288 ) ) ;
#2392 = VECTOR ( 'NONE', #40341, 1000.000000000000227 ) ;
#2393 = CARTESIAN_POINT ( 'NONE',  ( -68.52794903032595641, 2.000000000000048850, 8.850418579662809648 ) ) ;
#2394 = VERTEX_POINT ( 'NONE', #24854 ) ;
#2395 = AXIS2_PLACEMENT_3D ( 'NONE', #36209, #18892, #27385 ) ;
#2396 = EDGE_LOOP ( 'NONE', ( #12277, #6153, #16177, #40514 ) ) ;
#2397 = CARTESIAN_POINT ( 'NONE',  ( -69.59783862807636012, -0.6008070088998225255, -7.493102809087827332 ) ) ;
#2398 = LINE ( 'NONE', #36215, #42166 ) ;
#2399 = DIRECTION ( 'NONE',  ( -0.5364919789714478471, 0.6444004775717705469, -0.5449076811759709926 ) ) ;
#2400 = DIRECTION ( 'NONE',  ( -0.5449076811759708816, 0.6444004775717707689, 0.5364919789714475140 ) ) ;
#2401 = CARTESIAN_POINT ( 'NONE',  ( -6.110905869600904872, 1.712176620043476140E-14, 2.600000000000000089 ) ) ;
#2402 = LINE ( 'NONE', #48983, #20377 ) ;
#2403 = VERTEX_POINT ( 'NONE', #20304 ) ;
#2404 = CARTESIAN_POINT ( 'NONE',  ( -13.27065584551087163, 0.000000000000000000, 12.04557950825129176 ) ) ;
#2405 = VECTOR ( 'NONE', #46121, 999.9999999999998863 ) ;
#2406 = EDGE_CURVE ( 'NONE', #54118, #12005, #54654, .T. ) ;
#2407 = CARTESIAN_POINT ( 'NONE',  ( -20.54126990917373519, -0.1191753592594197858, 4.760553241521720658 ) ) ;
#2408 = LINE ( 'NONE', #14914, #53228 ) ;
#2409 = ORIENTED_EDGE ( 'NONE', *, *, #10214, .T. ) ;
#2410 = DIRECTION ( 'NONE',  ( 0.3583679495452941066, 0.9335804264972041855, -0.000000000000000000 ) ) ;
#2411 = MANIFOLD_SOLID_BREP ( 'Fillet2', #42168 ) ;
#2412 = CARTESIAN_POINT ( 'NONE',  ( -22.03063064900203827, 19.66612883677992585, 4.421226519471689542 ) ) ;
#2413 = AXIS2_PLACEMENT_3D ( 'NONE', #3140, #55121, #12229 ) ;
#2414 = FACE_OUTER_BOUND ( 'NONE', #44645, .T. ) ;
#2415 = ORIENTED_EDGE ( 'NONE', *, *, #54672, .T. ) ;
#2416 = FACE_OUTER_BOUND ( 'NONE', #22042, .T. ) ;
#2417 = VECTOR ( 'NONE', #51836, 999.9999999999998863 ) ;
#2418 = ORIENTED_EDGE ( 'NONE', *, *, #48924, .F. ) ;
#2419 = ORIENTED_EDGE ( 'NONE', *, *, #18520, .F. ) ;
#2420 = AXIS2_PLACEMENT_3D ( 'NONE', #19201, #40546, #40240 ) ;
#2421 = ORIENTED_EDGE ( 'NONE', *, *, #14087, .F. ) ;
#2422 = ORIENTED_EDGE ( 'NONE', *, *, #14638, .T. ) ;
#2423 = EDGE_LOOP ( 'NONE', ( #14543, #51405, #35060, #33867 ) ) ;
#2424 = DIRECTION ( 'NONE',  ( 0.7660212471507180654, -0.6427876096865404731, 0.005961354470445141482 ) ) ;
#2425 = ORIENTED_EDGE ( 'NONE', *, *, #48924, .T. ) ;
#2426 = VECTOR ( 'NONE', #40847, 999.9999999999998863 ) ;
#2427 = ORIENTED_EDGE ( 'NONE', *, *, #28275, .F. ) ;
#2428 = PLANE ( 'NONE',  #14148 ) ;
#2429 = EDGE_CURVE ( 'NONE', #40913, #40301, #8105, .T. ) ;
#2430 = EDGE_LOOP ( 'NONE', ( #10941, #48817, #52631, #54645 ) ) ;
#2431 = ORIENTED_EDGE ( 'NONE', *, *, #15801, .T. ) ;
#2432 = AXIS2_PLACEMENT_3D ( 'NONE', #47385, #8496, #54174 ) ;
#2433 = ORIENTED_EDGE ( 'NONE', *, *, #21854, .F. ) ;
#2434 = AXIS2_PLACEMENT_3D ( 'NONE', #10521, #45154, #6256 ) ;
#2435 = LINE ( 'NONE', #11227, #7557 ) ;
#2436 = DIRECTION ( 'NONE',  ( -0.005961354470445682716, -0.6427876096865404731, 0.7660212471507180654 ) ) ;
#2437 = DIRECTION ( 'NONE',  ( -0.7660212471507179544, -0.6427876096865405842, -0.005961354470445141482 ) ) ;
#2438 = LINE ( 'NONE', #2141, #14166 ) ;
#2439 = ORIENTED_EDGE ( 'NONE', *, *, #30729, .F. ) ;
#2440 = DIRECTION ( 'NONE',  ( 0.5364919789714477361, 0.6444004775717706579, 0.5449076811759711036 ) ) ;
#2441 = ORIENTED_EDGE ( 'NONE', *, *, #25891, .F. ) ;
#2442 = EDGE_CURVE ( 'NONE', #8484, #36489, #3818, .T. ) ;
#2443 = ORIENTED_EDGE ( 'NONE', *, *, #20343, .T. ) ;
#2444 = DIRECTION ( 'NONE',  ( -0.5364919789714478471, 0.6444004775717705469, -0.5449076811759709926 ) ) ;
#2445 = DIRECTION ( 'NONE',  ( 0.000000000000000000, -0.000000000000000000, -1.000000000000000000 ) ) ;
#2446 = UNCERTAINTY_MEASURE_WITH_UNIT (LENGTH_MEASURE( 1.000000000000000082E-05 ), #16772, 'distance_accuracy_value', 'NONE');
#2447 = EDGE_CURVE ( 'NONE', #83, #1327, #16319, .T. ) ;
#2448 = EDGE_CURVE ( 'NONE', #52648, #17442, #47259, .T. ) ;
#2449 = VECTOR ( 'NONE', #17949, 1000.000000000000000 ) ;
#2450 = CARTESIAN_POINT ( 'NONE',  ( -27.13299098042555002, 16.99303619941258603, -4.657414165320978405 ) ) ;
#2451 = DIRECTION ( 'NONE',  ( -0.5449076811759708816, 0.6444004775717707689, 0.5364919789714475140 ) ) ;
#2452 = CARTESIAN_POINT ( 'NONE',  ( 4.848100717410756211, 0.000000000000000000, -2.029539223447461183 ) ) ;
#2453 = DIRECTION ( 'NONE',  ( -0.9999697198139514409, -0.000000000000000000, -0.007781995580013368816 ) ) ;
#2454 = ORIENTED_EDGE ( 'NONE', *, *, #7570, .T. ) ;
#2455 = PLANE ( 'NONE',  #34686 ) ;
#2456 = EDGE_CURVE ( 'NONE', #13435, #22728, #39034, .T. ) ;
#2457 = EDGE_LOOP ( 'NONE', ( #12102, #15454, #25794, #32455 ) ) ;
#2458 = FACE_OUTER_BOUND ( 'NONE', #1370, .T. ) ;
#2459 = DIRECTION ( 'NONE',  ( 0.9999697198139515519, 0.000000000000000000, 0.007781995580013368816 ) ) ;
#2460 = ADVANCED_FACE ( 'NONE', ( #12911 ), #31064, .F. ) ;
#2462 = CARTESIAN_POINT ( 'NONE',  ( -23.66772770479517618, 18.99370688441070953, -4.503111145262439052 ) ) ;
#2461 = VECTOR ( 'NONE', #30511, 1000.000000000000000 ) ;
#2463 = LINE ( 'NONE', #24321, #2294 ) ;
#2464 = EDGE_CURVE ( 'NONE', #22669, #33221, #48103, .T. ) ;
#2465 = FACE_OUTER_BOUND ( 'NONE', #50742, .T. ) ;
#2466 = VECTOR ( 'NONE', #3509, 999.9999999999998863 ) ;
#2467 = ORIENTED_EDGE ( 'NONE', *, *, #54466, .T. ) ;
#2468 = DIRECTION ( 'NONE',  ( 0.007781995580012663651, 0.000000000000000000, -0.9999697198139515519 ) ) ;
#2469 = DIRECTION ( 'NONE',  ( -0.7660212471507179544, -0.6427876096865405842, -0.005961354470445141482 ) ) ;
#2470 = LINE ( 'NONE', #15794, #3398 ) ;
#2471 = ADVANCED_FACE ( 'NONE', ( #21724 ), #8671, .F. ) ;
#2472 = AXIS2_PLACEMENT_3D ( 'NONE', #20023, #24025, #10712 ) ;
#2473 = DIRECTION ( 'NONE',  ( -0.005002170337468016433, -0.7660444431189770143, 0.6427681459581293666 ) ) ;
#2474 = PLANE ( 'NONE',  #3105 ) ;
#2475 = DIRECTION ( 'NONE',  ( 0.000000000000000000, 1.000000000000000000, 0.000000000000000000 ) ) ;
#2476 = PLANE ( 'NONE',  #53730 ) ;
#2477 = EDGE_CURVE ( 'NONE', #27257, #5134, #34774, .T. ) ;
#2478 = DIRECTION ( 'NONE',  ( -0.3620778797217457656, 0.000000000000000000, -0.9321478471874540261 ) ) ;
#2479 = CARTESIAN_POINT ( 'NONE',  ( -25.20278734466900517, 0.000000000000000000, 6.670939612111840944 ) ) ;
#2480 = ORIENTED_EDGE ( 'NONE', *, *, #19962, .F. ) ;
#2481 = ORIENTED_EDGE ( 'NONE', *, *, #31753, .F. ) ;
#2482 = ORIENTED_EDGE ( 'NONE', *, *, #34192, .T. ) ;
#2483 = ORIENTED_EDGE ( 'NONE', *, *, #36120, .T. ) ;
#2484 = ORIENTED_EDGE ( 'NONE', *, *, #53692, .T. ) ;
#2485 = ORIENTED_EDGE ( 'NONE', *, *, #28912, .F. ) ;
#2486 = DIRECTION ( 'NONE',  ( 0.005002170337468016433, -0.7660444431189770143, -0.6427681459581293666 ) ) ;
#2487 = LINE ( 'NONE', #19805, #38349 ) ;
#2488 = CARTESIAN_POINT ( 'NONE',  ( -15.43759333659924415, -0.1191753592594194527, 4.800271232719476089 ) ) ;
#2489 = ORIENTED_EDGE ( 'NONE', *, *, #45101, .T. ) ;
#2490 = DIRECTION ( 'NONE',  ( -0.5364919789714478471, 0.6444004775717705469, -0.5449076811759709926 ) ) ;
#2491 = EDGE_CURVE ( 'NONE', #9864, #44261, #18280, .T. ) ;
#2492 = ORIENTED_EDGE ( 'NONE', *, *, #46593, .F. ) ;
#2493 = VERTEX_POINT ( 'NONE', #21985 ) ;
#2494 = VECTOR ( 'NONE', #36470, 999.9999999999998863 ) ;
#2495 = CARTESIAN_POINT ( 'NONE',  ( -66.57230477427758331, -8.723772755596309381, -0.6815216469038195557 ) ) ;
#2496 = DIRECTION ( 'NONE',  ( 0.6246952433987893460, 0.7422098413412802076, -0.2426528472758539279 ) ) ;
#2497 = FACE_OUTER_BOUND ( 'NONE', #3491, .T. ) ;
#2498 = ORIENTED_EDGE ( 'NONE', *, *, #32208, .T. ) ;
#2499 = LINE ( 'NONE', #49903, #12904 ) ;
#2500 = EDGE_CURVE ( 'NONE', #23765, #44810, #25999, .T. ) ;
#2501 = VECTOR ( 'NONE', #29255, 1000.000000000000227 ) ;
#2502 = DIRECTION ( 'NONE',  ( 0.9999697198139515519, 0.000000000000000000, 0.007781995580013368816 ) ) ;
#2503 = PLANE ( 'NONE',  #16677 ) ;
#2504 = EDGE_CURVE ( 'NONE', #18224, #23248, #5257, .T. ) ;
#2505 = LINE ( 'NONE', #40846, #24484 ) ;
#2506 = DIRECTION ( 'NONE',  ( -0.5449076811759708816, 0.6444004775717707689, 0.5364919789714475140 ) ) ;
#2507 = LINE ( 'NONE', #10185, #14989 ) ;
#2508 = DIRECTION ( 'NONE',  ( -0.5449076811759708816, 0.6444004775717707689, 0.5364919789714475140 ) ) ;
#2509 = CARTESIAN_POINT ( 'NONE',  ( -9.110551994824897193, -1.000000000000000000, 3.538847790438064411 ) ) ;
#2510 = CARTESIAN_POINT ( 'NONE',  ( -13.73537992771392702, 3.362543313726507499, 7.735115571941824086 ) ) ;
#2511 = ORIENTED_EDGE ( 'NONE', *, *, #44312, .T. ) ;
#2512 = CYLINDRICAL_SURFACE ( 'NONE', #26543, 2.125000000000000000 ) ;
#2513 = ORIENTED_EDGE ( 'NONE', *, *, #16957, .T. ) ;
#2514 = DIRECTION ( 'NONE',  ( 0.9999697198139515519, 0.000000000000000000, 0.007781995580013368816 ) ) ;
#2515 = CARTESIAN_POINT ( 'NONE',  ( -11.69321732157139948, -0.1191753592594181482, 1.323669135366288829 ) ) ;
#2516 = EDGE_CURVE ( 'NONE', #55726, #52569, #22564, .T. ) ;
#2517 = LINE ( 'NONE', #37157, #45875 ) ;
#2518 = PLANE ( 'NONE',  #19609 ) ;
#2519 = CARTESIAN_POINT ( 'NONE',  ( -11.40636015113596180, 0.000000000000000000, 11.32142374880780089 ) ) ;
#2520 = EDGE_CURVE ( 'NONE', #35585, #1901, #9497, .T. ) ;
#2521 = LINE ( 'NONE', #41960, #31031 ) ;
#2522 = ORIENTED_EDGE ( 'NONE', *, *, #37873, .F. ) ;
#2523 = CARTESIAN_POINT ( 'NONE',  ( -20.54204810873173415, 0.000000000000000000, 4.860550213503115558 ) ) ;
#2524 = FACE_OUTER_BOUND ( 'NONE', #13127, .T. ) ;
#2525 = DIRECTION ( 'NONE',  ( 0.9999697198139515519, 0.000000000000000000, 0.007781995580013368816 ) ) ;
#2526 = DIRECTION ( 'NONE',  ( 0.000000000000000000, -0.000000000000000000, -1.000000000000000000 ) ) ;
#2527 = CARTESIAN_POINT ( 'NONE',  ( -24.26986129792355129, -0.1191753592594197858, 6.208864760408702388 ) ) ;
#2528 = ADVANCED_FACE ( 'NONE', ( #25691 ), #26821, .F. ) ;
#2529 = LINE ( 'NONE', #44857, #52683 ) ;
#2530 = LINE ( 'NONE', #36622, #11225 ) ;
#2531 = DIRECTION ( 'NONE',  ( 0.005002170337468016433, -0.7660444431189770143, -0.6427681459581293666 ) ) ;
#2532 = LINE ( 'NONE', #45682, #29280 ) ;
#2533 = ORIENTED_EDGE ( 'NONE', *, *, #522, .F. ) ;
#2534 = EDGE_CURVE ( 'NONE', #41874, #50265, #39621, .T. ) ;
#2535 = CARTESIAN_POINT ( 'NONE',  ( -10.28764359011176488, -0.1191753592594198830, 0.7776965645825208995 ) ) ;
#2536 = EDGE_LOOP ( 'NONE', ( #8985, #21040, #11183, #53662 ) ) ;
#2537 = CARTESIAN_POINT ( 'NONE',  ( -17.83139810946674686, -0.1191753592594197858, 13.85674710641801788 ) ) ;
#2538 = DIRECTION ( 'NONE',  ( 0.9999697198139515519, 0.000000000000000000, 0.007781995580013368816 ) ) ;
#2539 = VECTOR ( 'NONE', #9517, 1000.000000000000114 ) ;
#2540 = ORIENTED_EDGE ( 'NONE', *, *, #55280, .F. ) ;
#2541 = EDGE_LOOP ( 'NONE', ( #8129, #19924, #8338, #17598 ) ) ;
#2542 = CARTESIAN_POINT ( 'NONE',  ( -12.73617685956571322, 0.000000000000000000, 3.074636959462103469 ) ) ;
#2543 = ORIENTED_EDGE ( 'NONE', *, *, #53364, .T. ) ;
#2544 = ORIENTED_EDGE ( 'NONE', *, *, #39856, .T. ) ;
#2545 = VERTEX_POINT ( 'NONE', #34489 ) ;
#2546 = DIRECTION ( 'NONE',  ( -0.9999697198139514409, -0.000000000000000000, -0.007781995580013368816 ) ) ;
#2547 = LINE ( 'NONE', #32402, #38641 ) ;
#2548 = DIRECTION ( 'NONE',  ( 0.000000000000000000, -1.000000000000000000, 0.000000000000000000 ) ) ;
#2549 = ADVANCED_FACE ( 'NONE', ( #700 ), #35613, .F. ) ;
#2550 = ORIENTED_EDGE ( 'NONE', *, *, #45445, .F. ) ;
#2552 = VERTEX_POINT ( 'NONE', #30242 ) ;
#2551 = EDGE_CURVE ( 'NONE', #49537, #2028, #30541, .T. ) ;
#2553 = CARTESIAN_POINT ( 'NONE',  ( -65.97443392703776510, -1.387778780781445676E-14, 3.266248677641426568 ) ) ;
#2554 = LINE ( 'NONE', #19876, #6454 ) ;
#2556 = EDGE_CURVE ( 'NONE', #8862, #55978, #35341, .T. ) ;
#2555 = ORIENTED_EDGE ( 'NONE', *, *, #37718, .T. ) ;
#2557 = PLANE ( 'NONE',  #26432 ) ;
#2558 = ORIENTED_EDGE ( 'NONE', *, *, #16904, .T. ) ;
#2559 = LINE ( 'NONE', #49717, #10363 ) ;
#2560 = FACE_OUTER_BOUND ( 'NONE', #8428, .T. ) ;
#2561 = EDGE_CURVE ( 'NONE', #37629, #44931, #8954, .T. ) ;
#2562 = ADVANCED_FACE ( 'NONE', ( #13485 ), #21454, .F. ) ;
#2563 = EDGE_CURVE ( 'NONE', #52991, #17775, #32202, .T. ) ;
#2564 = ORIENTED_EDGE ( 'NONE', *, *, #36836, .F. ) ;
#2565 = CARTESIAN_POINT ( 'NONE',  ( -11.40636015113596180, 0.000000000000000000, 11.32142374880780089 ) ) ;
#2566 = PLANE ( 'NONE',  #24559 ) ;
#2567 = ORIENTED_EDGE ( 'NONE', *, *, #25164, .T. ) ;
#2568 = FACE_OUTER_BOUND ( 'NONE', #32711, .T. ) ;
#2569 = LINE ( 'NONE', #23593, #40251 ) ;
#2570 = CARTESIAN_POINT ( 'NONE',  ( -13.96236475351288497, 3.686347215771509589, 1.987774589328580532 ) ) ;
#2571 = ORIENTED_EDGE ( 'NONE', *, *, #2504, .T. ) ;
#2572 = VECTOR ( 'NONE', #43518, 1000.000000000000000 ) ;
#2573 = CARTESIAN_POINT ( 'NONE',  ( -58.57533928340691887, 0.08623575067603483912, 2.999999999999993339 ) ) ;
#2574 = CARTESIAN_POINT ( 'NONE',  ( -19.88163492745564298, 4.010151117816508126, 11.18536447734173933 ) ) ;
#2575 = CARTESIAN_POINT ( 'NONE',  ( 0.000000000000000000, 0.000000000000000000, -2.125000000000000000 ) ) ;
#2576 = ADVANCED_FACE ( 'NONE', ( #10049 ), #49526, .F. ) ;
#2577 = DIRECTION ( 'NONE',  ( -0.9999697198139514409, -0.000000000000000000, -0.007781995580013368816 ) ) ;
#2578 = CARTESIAN_POINT ( 'NONE',  ( -17.83139810946674686, -0.1191753592594197858, 13.85674710641801788 ) ) ;
#2579 = DIRECTION ( 'NONE',  ( 0.6427681459581294776, -0.7660444431189769032, 0.005002170337467562802 ) ) ;
#2580 = EDGE_CURVE ( 'NONE', #35585, #12064, #10884, .T. ) ;
#2581 = FACE_OUTER_BOUND ( 'NONE', #35716, .T. ) ;
#2582 = ORIENTED_EDGE ( 'NONE', *, *, #6427, .T. ) ;
#2583 = CARTESIAN_POINT ( 'NONE',  ( -17.74560456716937296, 0.000000000000000000, 3.774316574337878372 ) ) ;
#2584 = LINE ( 'NONE', #37810, #48571 ) ;
#2585 = ADVANCED_FACE ( 'NONE', ( #49792 ), #23123, .F. ) ;
#2586 = CARTESIAN_POINT ( 'NONE',  ( -66.45030873714300412, -4.509921584324644611E-12, 0.7134948435194322647 ) ) ;
#2587 = ORIENTED_EDGE ( 'NONE', *, *, #30039, .T. ) ;
#2588 = CARTESIAN_POINT ( 'NONE',  ( -16.53317331066696383, 0.000000000000000000, 13.31285208727739899 ) ) ;
#2589 = MANIFOLD_SOLID_BREP ( 'Fillet2', #27672 ) ;
#2590 = CARTESIAN_POINT ( 'NONE',  ( -12.67969208061091813, 1.581621852479006440, 4.402255037361733514 ) ) ;
#2591 = EDGE_CURVE ( 'NONE', #7363, #17655, #15417, .T. ) ;
#2592 = CARTESIAN_POINT ( 'NONE',  ( 2.072287782118878319, 0.000000000000000000, -2.950529333540147015 ) ) ;
#2593 = CARTESIAN_POINT ( 'NONE',  ( -23.33693525117809386, 0.000000000000000000, 5.746789908705562944 ) ) ;
#2594 = EDGE_CURVE ( 'NONE', #20663, #18937, #19696, .T. ) ;
#2595 = LINE ( 'NONE', #1753, #23849 ) ;
#2596 = ORIENTED_EDGE ( 'NONE', *, *, #22720, .T. ) ;
#2597 = ORIENTED_EDGE ( 'NONE', *, *, #9887, .T. ) ;
#2598 = DIRECTION ( 'NONE',  ( 0.007781995580012663651, -3.146120232559066537E-19, -0.9999697198139514409 ) ) ;
#2599 = CARTESIAN_POINT ( 'NONE',  ( -16.75240362923608473, 0.000000000000000000, 7.475366591759194712 ) ) ;
#2600 = VERTEX_POINT ( 'NONE', #2364 ) ;
#2601 = CARTESIAN_POINT ( 'NONE',  ( -15.53262040112807441, 0.000000000000000000, 4.160870598627338879 ) ) ;
#2602 = ORIENTED_EDGE ( 'NONE', *, *, #25224, .F. ) ;
#2603 = DIRECTION ( 'NONE',  ( 0.005002170337468016433, -0.7660444431189770143, -0.6427681459581293666 ) ) ;
#2604 = ORIENTED_EDGE ( 'NONE', *, *, #55126, .T. ) ;
#2605 = ORIENTED_EDGE ( 'NONE', *, *, #26683, .T. ) ;
#2606 = CARTESIAN_POINT ( 'NONE',  ( -11.65596995895249854, -1.165603555308155626, 3.122460313520408093 ) ) ;
#2607 = PLANE ( 'NONE',  #50430 ) ;
#2608 = DIRECTION ( 'NONE',  ( 0.5364919789714477361, 0.6444004775717706579, 0.5449076811759711036 ) ) ;
#2609 = ORIENTED_EDGE ( 'NONE', *, *, #31310, .F. ) ;
#2610 = AXIS2_PLACEMENT_3D ( 'NONE', #34638, #13373, #3697 ) ;
#2611 = DIRECTION ( 'NONE',  ( 0.007781995580012662783, 0.000000000000000000, -0.9999697198139514409 ) ) ;
#2612 = ORIENTED_EDGE ( 'NONE', *, *, #21713, .T. ) ;
#2613 = ORIENTED_EDGE ( 'NONE', *, *, #24050, .F. ) ;
#2614 = ORIENTED_EDGE ( 'NONE', *, *, #25582, .F. ) ;
#2615 = DIRECTION ( 'NONE',  ( 0.005002170337468016433, -0.7660444431189770143, -0.6427681459581293666 ) ) ;
#2616 = EDGE_LOOP ( 'NONE', ( #31636, #8403, #13235, #6325 ) ) ;
#2617 = DIRECTION ( 'NONE',  ( 0.6427681459581294776, -0.7660444431189769032, 0.005002170337467562802 ) ) ;
#2618 = VERTEX_POINT ( 'NONE', #14875 ) ;
#2619 = DIRECTION ( 'NONE',  ( -0.7660212471507179544, -0.6427876096865405842, -0.005961354470445141482 ) ) ;
#2620 = CARTESIAN_POINT ( 'NONE',  ( -14.01701317841955508, 0.000000000000000000, 2.326005055450897085 ) ) ;
#2621 = EDGE_CURVE ( 'NONE', #25423, #34828, #1238, .T. ) ;
#2622 = EDGE_CURVE ( 'NONE', #10480, #16665, #45252, .T. ) ;
#2623 = ORIENTED_EDGE ( 'NONE', *, *, #45, .F. ) ;
#2624 = DIRECTION ( 'NONE',  ( -0.005002170337468016433, -0.7660444431189770143, 0.6427681459581293666 ) ) ;
#2625 = ORIENTED_EDGE ( 'NONE', *, *, #41798, .T. ) ;
#2626 = EDGE_CURVE ( 'NONE', #4790, #18918, #44406, .T. ) ;
#2627 = LINE ( 'NONE', #24485, #51846 ) ;
#2628 = DIRECTION ( 'NONE',  ( -0.000000000000000000, -0.000000000000000000, 1.000000000000000000 ) ) ;
#2629 = CARTESIAN_POINT ( 'NONE',  ( -27.06630483948590893, -0.1191753592594197858, 7.295098399573937797 ) ) ;
#2630 = DIRECTION ( 'NONE',  ( 0.005961354470445682716, -0.6427876096865404731, -0.7660212471507180654 ) ) ;
#2631 = CARTESIAN_POINT ( 'NONE',  ( -11.87243407472968926, 0.000000000000000000, 11.50246268866867361 ) ) ;
#2632 = VERTEX_POINT ( 'NONE', #31908 ) ;
#2633 = VERTEX_POINT ( 'NONE', #40723 ) ;
#2634 = DIRECTION ( 'NONE',  ( -0.9999697198139514409, -0.000000000000000000, -0.007781995580013368816 ) ) ;
#2635 = DIRECTION ( 'NONE',  ( 0.007781995580012663651, -3.146120232559066537E-19, -0.9999697198139514409 ) ) ;
#2636 = CARTESIAN_POINT ( 'NONE',  ( -15.50102849149811135, -0.1191753592594197858, 12.95155240711365430 ) ) ;
#2638 = EDGE_CURVE ( 'NONE', #33054, #36712, #49224, .T. ) ;
#2637 = CARTESIAN_POINT ( 'NONE',  ( -22.02230666951336246, 19.67040017278726438, 4.420763615217817133 ) ) ;
#2639 = PLANE ( 'NONE',  #52159 ) ;
#2640 = ORIENTED_EDGE ( 'NONE', *, *, #14569, .F. ) ;
#2641 = CARTESIAN_POINT ( 'NONE',  ( -9.075990533167328067, 0.000000000000000000, 10.41622904950343909 ) ) ;
#2642 = DIRECTION ( 'NONE',  ( 0.000000000000000000, -1.000000000000000000, 0.000000000000000000 ) ) ;
#2643 = ORIENTED_EDGE ( 'NONE', *, *, #5906, .T. ) ;
#2644 = CARTESIAN_POINT ( 'NONE',  ( -16.95084117408287483, 0.000000000000000000, 7.273816248680401664 ) ) ;
#2645 = DIRECTION ( 'NONE',  ( 0.7660212471507180654, -0.6427876096865404731, 0.005961354470445141482 ) ) ;
#2646 = ORIENTED_EDGE ( 'NONE', *, *, #34681, .T. ) ;
#2647 = CARTESIAN_POINT ( 'NONE',  ( -11.80690306588353877, 0.000000000000000000, 3.081868782998124168 ) ) ;
#2648 = CARTESIAN_POINT ( 'NONE',  ( -8.409922665610809034, 0.000000000000000000, 10.23674650875856962 ) ) ;
#2649 = ADVANCED_FACE ( 'NONE', ( #44679 ), #10338, .F. ) ;
#2650 = CARTESIAN_POINT ( 'NONE',  ( -15.87975247367846166, 0.000000000000000000, 2.850166870931599927 ) ) ;
#2651 = EDGE_CURVE ( 'NONE', #48176, #17974, #6105, .T. ) ;
#2652 = LINE ( 'NONE', #50370, #9671 ) ;
#2653 = LINE ( 'NONE', #41571, #207 ) ;
#2654 = VERTEX_POINT ( 'NONE', #56210 ) ;
#2655 = ADVANCED_FACE ( 'NONE', ( #28480 ), #25286, .F. ) ;
#2656 = EDGE_LOOP ( 'NONE', ( #28530, #2219, #10536, #11574 ) ) ;
#2657 = FACE_OUTER_BOUND ( 'NONE', #21406, .T. ) ;
#2658 = LINE ( 'NONE', #8068, #39459 ) ;
#2659 = LINE ( 'NONE', #7218, #55894 ) ;
#2660 = ADVANCED_FACE ( 'NONE', ( #8824 ), #55954, .F. ) ;
#2661 = FACE_OUTER_BOUND ( 'NONE', #13265, .T. ) ;
#2662 = LINE ( 'NONE', #37053, #38291 ) ;
#2663 = ADVANCED_FACE ( 'NONE', ( #11154 ), #16458, .F. ) ;
#2664 = PLANE ( 'NONE',  #47596 ) ;
#2665 = ORIENTED_EDGE ( 'NONE', *, *, #16428, .T. ) ;
#2666 = DIRECTION ( 'NONE',  ( -0.7660212471507179544, -0.6427876096865405842, -0.005961354470445141482 ) ) ;
#2667 = LINE ( 'NONE', #33066, #23300 ) ;
#2668 = LINE ( 'NONE', #46682, #49617 ) ;
#2669 = ORIENTED_EDGE ( 'NONE', *, *, #33178, .T. ) ;
#2670 = CARTESIAN_POINT ( 'NONE',  ( 2.072287782118878319, 0.000000000000000000, -2.950529333540147015 ) ) ;
#2671 = DIRECTION ( 'NONE',  ( 0.005002170337468016433, -0.7660444431189770143, -0.6427681459581293666 ) ) ;
#2672 = FACE_OUTER_BOUND ( 'NONE', #36158, .T. ) ;
#2673 = VERTEX_POINT ( 'NONE', #17048 ) ;
#2674 = LINE ( 'NONE', #28246, #4137 ) ;
#2675 = EDGE_LOOP ( 'NONE', ( #22676, #55865, #37196, #47851 ) ) ;
#2676 = ORIENTED_EDGE ( 'NONE', *, *, #13463, .F. ) ;
#2677 = VERTEX_POINT ( 'NONE', #38055 ) ;
#2678 = ORIENTED_EDGE ( 'NONE', *, *, #50651, .T. ) ;
#2679 = VERTEX_POINT ( 'NONE', #34363 ) ;
#2680 = CARTESIAN_POINT ( 'NONE',  ( -12.66989033008971077, -0.1191753592594181482, 7.407134626131880673 ) ) ;
#2681 = ORIENTED_EDGE ( 'NONE', *, *, #18929, .T. ) ;
#2682 = EDGE_CURVE ( 'NONE', #19674, #30623, #30386, .T. ) ;
#2683 = EDGE_LOOP ( 'NONE', ( #55117, #19603, #53392, #16395 ) ) ;
#2684 = LINE ( 'NONE', #10404, #50307 ) ;
#2685 = ORIENTED_EDGE ( 'NONE', *, *, #33239, .F. ) ;
#2686 = ORIENTED_EDGE ( 'NONE', *, *, #5710, .F. ) ;
#2687 = EDGE_CURVE ( 'NONE', #41949, #53748, #25005, .T. ) ;
#2688 = ADVANCED_FACE ( 'NONE', ( #29555 ), #33786, .F. ) ;
#2689 = LINE ( 'NONE', #24012, #47534 ) ;
#2690 = DIRECTION ( 'NONE',  ( -0.5449076811759708816, 0.6444004775717707689, 0.5364919789714475140 ) ) ;
#2691 = PLANE ( 'NONE',  #38679 ) ;
#2692 = DIRECTION ( 'NONE',  ( 0.5449076811759707706, 0.6444004775717708799, -0.5364919789714476250 ) ) ;
#2693 = PLANE ( 'NONE',  #22921 ) ;
#2694 = VERTEX_POINT ( 'NONE', #3683 ) ;
#2695 = VERTEX_POINT ( 'NONE', #25547 ) ;
#2696 = DIRECTION ( 'NONE',  ( 0.9999697198139515519, 0.000000000000000000, 0.007781995580013368816 ) ) ;
#2697 = CARTESIAN_POINT ( 'NONE',  ( -16.33317936670417225, 0.000000000000000000, 13.31440848639340224 ) ) ;
#2698 = EDGE_CURVE ( 'NONE', #38787, #27265, #51667, .T. ) ;
#2699 = FACE_OUTER_BOUND ( 'NONE', #6781, .T. ) ;
#2700 = DIRECTION ( 'NONE',  ( -0.005961354470445682716, -0.6427876096865404731, 0.7660212471507180654 ) ) ;
#2701 = DIRECTION ( 'NONE',  ( 0.9321478471874541372, 0.000000000000000000, -0.3620778797217453771 ) ) ;
#2702 = DIRECTION ( 'NONE',  ( 0.7660212471507180654, -0.6427876096865404731, 0.005961354470445141482 ) ) ;
#2703 = ORIENTED_EDGE ( 'NONE', *, *, #46106, .T. ) ;
#2704 = LINE ( 'NONE', #54669, #7488 ) ;
#2705 = ORIENTED_EDGE ( 'NONE', *, *, #17146, .F. ) ;
#2706 = DIRECTION ( 'NONE',  ( 0.005961354470445682716, -0.6427876096865404731, -0.7660212471507180654 ) ) ;
#2707 = DIRECTION ( 'NONE',  ( 0.7660212471507180654, -0.6427876096865404731, 0.005961354470445141482 ) ) ;
#2708 = CARTESIAN_POINT ( 'NONE',  ( -12.09672020551653127, 4.172053068839010059, 8.427147906474264261 ) ) ;
#2709 = CARTESIAN_POINT ( 'NONE',  ( -21.47419595591918906, 0.000000000000000000, 5.222628093224860102 ) ) ;
#2710 = EDGE_CURVE ( 'NONE', #34537, #54647, #20738, .T. ) ;
#2711 = LINE ( 'NONE', #55250, #33218 ) ;
#2712 = VECTOR ( 'NONE', #41371, 999.9999999999998863 ) ;
#2713 = ORIENTED_EDGE ( 'NONE', *, *, #38351, .F. ) ;
#2714 = CARTESIAN_POINT ( 'NONE',  ( -21.43680077527565686, -5.051250379848164052, 5.046941201800946963 ) ) ;
#2715 = DIRECTION ( 'NONE',  ( 0.7660212471507180654, -0.6427876096865404731, 0.005961354470445141482 ) ) ;
#2716 = DIRECTION ( 'NONE',  ( -0.9321478471874540261, 0.000000000000000000, 0.3620778797217457656 ) ) ;
#2717 = CARTESIAN_POINT ( 'NONE',  ( -13.27065584551087163, 0.000000000000000000, 12.04557950825129176 ) ) ;
#2718 = EDGE_CURVE ( 'NONE', #16343, #8547, #13061, .T. ) ;
#2719 = DIRECTION ( 'NONE',  ( -0.9999697198139514409, -0.000000000000000000, -0.007781995580013368816 ) ) ;
#2720 = PLANE ( 'NONE',  #51756 ) ;
#2721 = LINE ( 'NONE', #21181, #31080 ) ;
#2722 = CARTESIAN_POINT ( 'NONE',  ( -68.01236371044051054, -8.487308885305189676, 5.059064008999122564 ) ) ;
#2723 = CARTESIAN_POINT ( 'NONE',  ( -11.39548592363199120, 1.743523803501506375, 1.052697918879536676 ) ) ;
#2724 = ORIENTED_EDGE ( 'NONE', *, *, #36479, .F. ) ;
#2725 = ADVANCED_FACE ( 'NONE', ( #46869 ), #3423, .F. ) ;
#2726 = VERTEX_POINT ( 'NONE', #250 ) ;
#2727 = EDGE_CURVE ( 'NONE', #44057, #38668, #38322, .T. ) ;
#2728 = EDGE_CURVE ( 'NONE', #10018, #30955, #55651, .T. ) ;
#2729 = ORIENTED_EDGE ( 'NONE', *, *, #52591, .F. ) ;
#2730 = EDGE_LOOP ( 'NONE', ( #27336, #48814, #5995 ) ) ;
#2731 = EDGE_LOOP ( 'NONE', ( #39469, #448, #52549, #15398 ) ) ;
#2732 = ORIENTED_EDGE ( 'NONE', *, *, #27498, .T. ) ;
#2733 = DIRECTION ( 'NONE',  ( 0.007781995580012663651, 0.000000000000000000, -0.9999697198139515519 ) ) ;
#2734 = LINE ( 'NONE', #15525, #45608 ) ;
#2735 = EDGE_CURVE ( 'NONE', #52431, #43283, #16754, .T. ) ;
#2736 = PLANE ( 'NONE',  #48471 ) ;
#2738 = EDGE_CURVE ( 'NONE', #55501, #41332, #51938, .T. ) ;
#2737 = ORIENTED_EDGE ( 'NONE', *, *, #55575, .T. ) ;
#2739 = CARTESIAN_POINT ( 'NONE',  ( -15.96710241509184058, -0.1191753592594218814, 13.13259134697452879 ) ) ;
#2740 = ORIENTED_EDGE ( 'NONE', *, *, #5946, .F. ) ;
#2741 = LINE ( 'NONE', #54716, #19523 ) ;
#2742 = ORIENTED_EDGE ( 'NONE', *, *, #8559, .T. ) ;
#2743 = EDGE_CURVE ( 'NONE', #11370, #17587, #12511, .T. ) ;
#2744 = VECTOR ( 'NONE', #28996, 999.9999999999998863 ) ;
#2745 = CARTESIAN_POINT ( 'NONE',  ( -67.34291720966972150, -8.812237417047750654, 4.328853820092634308 ) ) ;
#2746 = CARTESIAN_POINT ( 'NONE',  ( -10.71015603238914515, -1.165603555308157846, 1.004320582572386655 ) ) ;
#2747 = DIRECTION ( 'NONE',  ( 0.9999697198139515519, 0.000000000000000000, 0.007781995580013368816 ) ) ;
#2748 = ORIENTED_EDGE ( 'NONE', *, *, #41111, .T. ) ;
#2749 = DIRECTION ( 'NONE',  ( -0.5449076811759708816, 0.6444004775717707689, 0.5364919789714475140 ) ) ;
#2750 = ORIENTED_EDGE ( 'NONE', *, *, #1486, .F. ) ;
#2751 = EDGE_CURVE ( 'NONE', #25140, #49888, #47129, .T. ) ;
#2752 = LINE ( 'NONE', #54726, #20044 ) ;
#2753 = LINE ( 'NONE', #3620, #4887 ) ;
#2754 = EDGE_CURVE ( 'NONE', #38944, #15364, #30676, .T. ) ;
#2755 = LINE ( 'NONE', #32875, #40834 ) ;
#2756 = DIRECTION ( 'NONE',  ( -0.7660212471507179544, -0.6427876096865405842, -0.005961354470445141482 ) ) ;
#2757 = DIRECTION ( 'NONE',  ( 0.7660212471507180654, -0.6427876096865404731, 0.005961354470445141482 ) ) ;
#2758 = DIRECTION ( 'NONE',  ( -0.5449076811759708816, 0.6444004775717707689, 0.5364919789714475140 ) ) ;
#2759 = DIRECTION ( 'NONE',  ( 0.9999697198139515519, 0.000000000000000000, 0.007781995580013368816 ) ) ;
#2760 = CARTESIAN_POINT ( 'NONE',  ( -10.74029228357944987, 0.000000000000000000, 11.14194120806293320 ) ) ;
#2761 = CARTESIAN_POINT ( 'NONE',  ( -17.68012102380225414, 0.000000000000000000, 7.268140824260386879 ) ) ;
#2762 = EDGE_LOOP ( 'NONE', ( #56046, #24354, #14204, #40634 ) ) ;
#2763 = CARTESIAN_POINT ( 'NONE',  ( -19.33760068587298164, 21.49370688441072019, 4.239878526350478793 ) ) ;
#2764 = ORIENTED_EDGE ( 'NONE', *, *, #14508, .F. ) ;
#2765 = VECTOR ( 'NONE', #55631, 1000.000000000000227 ) ;
#2766 = DIRECTION ( 'NONE',  ( 0.3535533905932738974, -0.6123724356957929160, -0.7071067811865487940 ) ) ;
#2767 = DIRECTION ( 'NONE',  ( 0.9999697198139515519, 0.000000000000000000, 0.007781995580013368816 ) ) ;
#2768 = DIRECTION ( 'NONE',  ( 0.005002170337468016433, -0.7660444431189770143, -0.6427681459581293666 ) ) ;
#2769 = LINE ( 'NONE', #36906, #22342 ) ;
#2770 = FACE_OUTER_BOUND ( 'NONE', #9873, .T. ) ;
#2771 = LINE ( 'NONE', #16147, #55511 ) ;
#2772 =( NAMED_UNIT ( * ) SI_UNIT ( $, .STERADIAN. ) SOLID_ANGLE_UNIT ( ) );
#2773 = ORIENTED_EDGE ( 'NONE', *, *, #22297, .F. ) ;
#2774 = LINE ( 'NONE', #51050, #21993 ) ;
#2775 = DIRECTION ( 'NONE',  ( -0.6246952433987893460, -0.7422098413412802076, 0.2426528472758542054 ) ) ;
#2776 = CARTESIAN_POINT ( 'NONE',  ( -11.16658230751120584, 0.000000000000000000, 6.210834479239226269 ) ) ;
#2777 = DIRECTION ( 'NONE',  ( 0.005002170337468016433, -0.7660444431189770143, -0.6427681459581293666 ) ) ;
#2778 = DIRECTION ( 'NONE',  ( 0.6246952433987894571, -0.7422098413412800966, -0.2426528472758541777 ) ) ;
#2779 = VECTOR ( 'NONE', #30383, 1000.000000000000114 ) ;
#2780 = CARTESIAN_POINT ( 'NONE',  ( -11.24522430293745501, 0.4483081953215036219, 1.985098250129335495 ) ) ;
#2781 = ADVANCED_FACE ( 'NONE', ( #40004 ), #9656, .F. ) ;
#2782 = DIRECTION ( 'NONE',  ( 0.6427681459581294776, -0.7660444431189769032, 0.005002170337467562802 ) ) ;
#2783 = LINE ( 'NONE', #20408, #617 ) ;
#2784 = DIRECTION ( 'NONE',  ( -0.2426528472758541499, 0.7422098413412800966, -0.6246952433987894571 ) ) ;
#2785 = EDGE_LOOP ( 'NONE', ( #40511, #29941, #51061 ) ) ;
#2786 = VECTOR ( 'NONE', #9300, 1000.000000000000227 ) ;
#2787 = DIRECTION ( 'NONE',  ( 0.007781995580012663651, 0.000000000000000000, -0.9999697198139515519 ) ) ;
#2788 = DIRECTION ( 'NONE',  ( 0.5449076811759707706, 0.6444004775717708799, -0.5364919789714476250 ) ) ;
#2789 = VERTEX_POINT ( 'NONE', #26670 ) ;
#2790 = LINE ( 'NONE', #15878, #12215 ) ;
#2791 = CARTESIAN_POINT ( 'NONE',  ( -9.745487481051126721, 0.000000000000000000, 2.728579125928399574 ) ) ;
#2792 = EDGE_CURVE ( 'NONE', #32241, #56100, #565, .T. ) ;
#2793 = ORIENTED_EDGE ( 'NONE', *, *, #11703, .F. ) ;
#2794 = ORIENTED_EDGE ( 'NONE', *, *, #32132, .T. ) ;
#2795 = CARTESIAN_POINT ( 'NONE',  ( -15.60102546347950536, 0.000000000000000000, 12.95077420755565356 ) ) ;
#2796 = ADVANCED_FACE ( 'NONE', ( #35468 ), #26380, .F. ) ;
#2797 = ORIENTED_EDGE ( 'NONE', *, *, #4762, .F. ) ;
#2798 = ORIENTED_EDGE ( 'NONE', *, *, #40347, .T. ) ;
#2799 = VERTEX_POINT ( 'NONE', #39464 ) ;
#2800 =( BOUNDED_SURFACE ( )  B_SPLINE_SURFACE ( 2, 3, ( 
 ( #15547, #23270, #2213, #41672 ),
 ( #28335, #15020, #45653, #32877 ),
 ( #27817, #11304, #28636, #40593 ) ),
 .UNSPECIFIED., .F., .F., .T. ) 
 B_SPLINE_SURFACE_WITH_KNOTS ( ( 3, 3 ),
 ( 4, 4 ),
 ( 0.000000000000000000, 1.000000000000000000 ),
 ( -0.001575000000000004998, 7.500000000001961749E-05 ),
 .UNSPECIFIED. ) 
 GEOMETRIC_REPRESENTATION_ITEM ( )  RATIONAL_B_SPLINE_SURFACE ( (
 ( 1.000000000000000000, 1.000000000000000000, 1.000000000000000000, 1.000000000000000000),
 ( 0.7071067811865475727, 0.7071067811865475727, 0.7071067811865484609, 0.7071067811865484609),
 ( 1.000000000000000000, 1.000000000000000000, 1.000000000000000000, 1.000000000000000000) ) ) 
 REPRESENTATION_ITEM ( '' )  SURFACE ( )  );
#2801 = PLANE ( 'NONE',  #50166 ) ;
#2802 = FACE_OUTER_BOUND ( 'NONE', #39333, .T. ) ;
#2803 =( REPRESENTATION_RELATIONSHIP ('NONE','NONE', #51076, #24540 ) REPRESENTATION_RELATIONSHIP_WITH_TRANSFORMATION ( #3916 )SHAPE_REPRESENTATION_RELATIONSHIP( ) );
#2804 = DIRECTION ( 'NONE',  ( -0.005961354470445682716, -0.6427876096865404731, 0.7660212471507180654 ) ) ;
#2805 = AXIS2_PLACEMENT_3D ( 'NONE', #4769, #22095, #9613 ) ;
#2806 = AXIS2_PLACEMENT_3D ( 'NONE', #29236, #24997, #28705 ) ;
#2807 = ADVANCED_FACE ( 'NONE', ( #5114 ), #27229, .T. ) ;
#2808 = ORIENTED_EDGE ( 'NONE', *, *, #17190, .T. ) ;
#2809 = ORIENTED_EDGE ( 'NONE', *, *, #18861, .T. ) ;
#2810 = EDGE_CURVE ( 'NONE', #28463, #18921, #43990, .T. ) ;
#2811 = DIRECTION ( 'NONE',  ( 0.000000000000000000, -0.000000000000000000, -1.000000000000000000 ) ) ;
#2812 = DIRECTION ( 'NONE',  ( 0.9659258262890692004, -0.2588190451025176864, 0.000000000000000000 ) ) ;
#2813 = ORIENTED_EDGE ( 'NONE', *, *, #381, .F. ) ;
#2814 = DIRECTION ( 'NONE',  ( -0.005002170337468016433, -0.7660444431189770143, 0.6427681459581293666 ) ) ;
#2815 = VERTEX_POINT ( 'NONE', #18732 ) ;
#2816 = PLANE ( 'NONE',  #41191 ) ;
#2817 = DIRECTION ( 'NONE',  ( 0.007781995580012662783, 0.000000000000000000, -0.9999697198139514409 ) ) ;
#2818 = EDGE_CURVE ( 'NONE', #40788, #43960, #13883, .T. ) ;
#2819 = ORIENTED_EDGE ( 'NONE', *, *, #33090, .T. ) ;
#2820 = LINE ( 'NONE', #6840, #25906 ) ;
#2821 = VECTOR ( 'NONE', #46547, 1000.000000000000000 ) ;
#2822 = EDGE_CURVE ( 'NONE', #42246, #17041, #52778, .T. ) ;
#2823 = PLANE ( 'NONE',  #30010 ) ;
#2824 = ORIENTED_EDGE ( 'NONE', *, *, #16381, .F. ) ;
#2825 = PLANE ( 'NONE',  #20406 ) ;
#2826 = CARTESIAN_POINT ( 'NONE',  ( -14.32396506529822666, -2.137015261443159009, 2.377053617101271499 ) ) ;
#2827 = LINE ( 'NONE', #46871, #26501 ) ;
#2828 = VERTEX_POINT ( 'NONE', #39749 ) ;
#2829 = DIRECTION ( 'NONE',  ( 0.9335804264972041855, -0.3583679495452941066, 0.000000000000000000 ) ) ;
#2830 = CARTESIAN_POINT ( 'NONE',  ( -15.08522782531868245, 0.000000000000000000, 6.380344729941936244 ) ) ;
#2831 = LINE ( 'NONE', #37493, #29453 ) ;
#2832 = DIRECTION ( 'NONE',  ( -0.005961354470445682716, -0.6427876096865404731, 0.7660212471507180654 ) ) ;
#2833 = CARTESIAN_POINT ( 'NONE',  ( -13.02512989487554940, 0.000000000000000000, 6.196370832167189313 ) ) ;
#2834 = DIRECTION ( 'NONE',  ( 0.2426528472758541499, 0.7422098413412800966, 0.6246952433987894571 ) ) ;
#2835 = DIRECTION ( 'NONE',  ( 0.5364919789714477361, 0.6444004775717706579, 0.5449076811759711036 ) ) ;
#2836 = ORIENTED_EDGE ( 'NONE', *, *, #20286, .T. ) ;
#2837 = CARTESIAN_POINT ( 'NONE',  ( -25.20200914511100265, -0.1191753592594197858, 6.570942640130446932 ) ) ;
#2838 = DIRECTION ( 'NONE',  ( 0.005002170337468016433, -0.7660444431189770143, -0.6427681459581293666 ) ) ;
#2839 = FACE_OUTER_BOUND ( 'NONE', #25705, .T. ) ;
#2840 = VERTEX_POINT ( 'NONE', #5384 ) ;
#2841 = FACE_OUTER_BOUND ( 'NONE', #18482, .T. ) ;
#2842 = LINE ( 'NONE', #29264, #19987 ) ;
#2843 = VECTOR ( 'NONE', #20640, 1000.000000000000227 ) ;
#2844 = AXIS2_PLACEMENT_3D ( 'NONE', #47481, #8595, #4349 ) ;
#2845 = CARTESIAN_POINT ( 'NONE',  ( -18.29747203306047609, -0.1191753592594177458, 14.03778604627889059 ) ) ;
#2846 = EDGE_CURVE ( 'NONE', #12718, #33290, #53368, .T. ) ;
#2847 = CARTESIAN_POINT ( 'NONE',  ( -12.06711556614055425, 0.000000000000000000, 2.510505623125562913 ) ) ;
#2848 = CARTESIAN_POINT ( 'NONE',  ( -55.47117325737978888, 6.581829179614757663, 1.080525476705103127 ) ) ;
#2849 = ORIENTED_EDGE ( 'NONE', *, *, #8680, .T. ) ;
#2850 = EDGE_CURVE ( 'NONE', #42368, #7355, #52513, .T. ) ;
#2851 = AXIS2_PLACEMENT_3D ( 'NONE', #4890, #39549, #12848 ) ;
#2852 = ORIENTED_EDGE ( 'NONE', *, *, #36181, .T. ) ;
#2853 = EDGE_CURVE ( 'NONE', #41757, #16888, #43694, .T. ) ;
#2854 = CARTESIAN_POINT ( 'NONE',  ( -14.20280369269832832, 0.000000000000000000, 12.40765738797303719 ) ) ;
#2855 = EDGE_CURVE ( 'NONE', #53976, #35993, #43666, .T. ) ;
#2856 = EDGE_CURVE ( 'NONE', #44514, #12005, #22441, .T. ) ;
#2857 = EDGE_CURVE ( 'NONE', #33148, #14703, #823, .T. ) ;
#2858 = DIRECTION ( 'NONE',  ( 0.5364919789714477361, 0.6444004775717706579, 0.5449076811759711036 ) ) ;
#2859 = CARTESIAN_POINT ( 'NONE',  ( -18.62663913851612563, 0.000000000000000000, 9.476767220270952308 ) ) ;
#2860 = EDGE_LOOP ( 'NONE', ( #1705, #6529, #37523, #49504 ) ) ;
#2861 = CARTESIAN_POINT ( 'NONE',  ( -13.02093818698098637, 0.000000000000000000, 5.657745369614448627 ) ) ;
#2862 = VECTOR ( 'NONE', #12985, 1000.000000000000227 ) ;
#2863 = EDGE_LOOP ( 'NONE', ( #42435, #41654, #17547, #53947 ) ) ;
#2864 = CARTESIAN_POINT ( 'NONE',  ( 1.086233639165236964, 0.000000000000000000, 2.796443541562362078 ) ) ;
#2865 = AXIS2_PLACEMENT_3D ( 'NONE', #17953, #29888, #34422 ) ;
#2866 = VERTEX_POINT ( 'NONE', #30924 ) ;
#2867 = VERTEX_POINT ( 'NONE', #48827 ) ;
#2868 = DIRECTION ( 'NONE',  ( -0.5449076811759708816, 0.6444004775717707689, 0.5364919789714475140 ) ) ;
#2869 = DIRECTION ( 'NONE',  ( -0.7660212471507179544, -0.6427876096865405842, -0.005961354470445141482 ) ) ;
#2870 = FACE_OUTER_BOUND ( 'NONE', #43731, .T. ) ;
#2871 = ORIENTED_EDGE ( 'NONE', *, *, #8357, .T. ) ;
#2872 = CARTESIAN_POINT ( 'NONE',  ( -18.09544690614880835, -4.403642575758163424, 3.769707965726611487 ) ) ;
#2873 = EDGE_CURVE ( 'NONE', #5037, #51473, #23271, .T. ) ;
#2874 = ORIENTED_EDGE ( 'NONE', *, *, #30411, .T. ) ;
#2876 = ORIENTED_EDGE ( 'NONE', *, *, #23935, .F. ) ;
#2875 = ADVANCED_FACE ( 'NONE', ( #47974 ), #48233, .F. ) ;
#2877 = ORIENTED_EDGE ( 'NONE', *, *, #44526, .F. ) ;
#2878 = CARTESIAN_POINT ( 'NONE',  ( -19.77061338776520216, 21.24370688441071664, -4.270683379717145733 ) ) ;
#2879 = CARTESIAN_POINT ( 'NONE',  ( -17.88741947389161524, 0.000000000000000000, 8.205197775622702139 ) ) ;
#2880 = EDGE_CURVE ( 'NONE', #24728, #43341, #28914, .T. ) ;
#2881 = ORIENTED_EDGE ( 'NONE', *, *, #27054, .F. ) ;
#2882 = FACE_OUTER_BOUND ( 'NONE', #23254, .T. ) ;
#2883 = ORIENTED_EDGE ( 'NONE', *, *, #24520, .T. ) ;
#2884 = CARTESIAN_POINT ( 'NONE',  ( -11.69463168032301326, -0.1191753592594202577, 1.505411197543670365 ) ) ;
#2885 = CARTESIAN_POINT ( 'NONE',  ( -15.87975247367846166, 0.000000000000000000, 2.850166870931599927 ) ) ;
#2886 = VECTOR ( 'NONE', #39581, 1000.000000000000114 ) ;
#2887 = EDGE_CURVE ( 'NONE', #43329, #54540, #28637, .T. ) ;
#2888 = VECTOR ( 'NONE', #13063, 999.9999999999998863 ) ;
#2889 = ORIENTED_EDGE ( 'NONE', *, *, #52752, .T. ) ;
#2890 = PLANE ( 'NONE',  #39525 ) ;
#2891 = ORIENTED_EDGE ( 'NONE', *, *, #15645, .F. ) ;
#2892 = CARTESIAN_POINT ( 'NONE',  ( -11.87243407472968926, 0.000000000000000000, 11.50246268866867361 ) ) ;
#2893 = LINE ( 'NONE', #46080, #9382 ) ;
#2894 = VECTOR ( 'NONE', #48238, 1000.000000000000227 ) ;
#2895 = DIRECTION ( 'NONE',  ( 0.7660212471507180654, -0.6427876096865404731, 0.005961354470445141482 ) ) ;
#2896 = LINE ( 'NONE', #11986, #27515 ) ;
#2897 = CARTESIAN_POINT ( 'NONE',  ( -28.92982233430281980, 0.000000000000000000, 7.919257187036034651 ) ) ;
#2898 = CARTESIAN_POINT ( 'NONE',  ( -20.43633616049215718, 0.000000000000000000, 5.030698901913927656 ) ) ;
#2899 = ORIENTED_EDGE ( 'NONE', *, *, #21688, .T. ) ;
#2900 = ORIENTED_EDGE ( 'NONE', *, *, #32772, .F. ) ;
#2901 = FACE_OUTER_BOUND ( 'NONE', #30824, .T. ) ;
#2902 = LINE ( 'NONE', #16003, #44808 ) ;
#2903 = VECTOR ( 'NONE', #33445, 999.9999999999998863 ) ;
#2904 = CARTESIAN_POINT ( 'NONE',  ( -70.00259797851279586, 0.1329035588801656675, 7.501778215771297553 ) ) ;
#2905 = DIRECTION ( 'NONE',  ( 0.005961354470445682716, -0.6427876096865404731, -0.7660212471507180654 ) ) ;
#2906 = FACE_OUTER_BOUND ( 'NONE', #32702, .T. ) ;
#2907 = PLANE ( 'NONE',  #7691 ) ;
#2908 = ORIENTED_EDGE ( 'NONE', *, *, #24683, .F. ) ;
#2909 = PLANE ( 'NONE',  #55826 ) ;
#2910 = FACE_OUTER_BOUND ( 'NONE', #55312, .T. ) ;
#2911 = VERTEX_POINT ( 'NONE', #46208 ) ;
#2912 = DIRECTION ( 'NONE',  ( 0.9999697198139515519, 0.000000000000000000, 0.007781995580013368816 ) ) ;
#2913 = PLANE ( 'NONE',  #14153 ) ;
#2914 = ORIENTED_EDGE ( 'NONE', *, *, #43481, .T. ) ;
#2915 = DIRECTION ( 'NONE',  ( -0.6427681459581293666, -0.7660444431189770143, -0.005002170337467561935 ) ) ;
#2916 = DIRECTION ( 'NONE',  ( 0.007781995580012662783, 0.000000000000000000, -0.9999697198139514409 ) ) ;
#2917 = FACE_OUTER_BOUND ( 'NONE', #18796, .T. ) ;
#2918 = AXIS2_PLACEMENT_3D ( 'NONE', #41002, #46366, #32228 ) ;
#2919 = PLANE ( 'NONE',  #19624 ) ;
#2920 = CARTESIAN_POINT ( 'NONE',  ( -19.59569683186026268, 0.000000000000000000, 14.58168106541950948 ) ) ;
#2921 = EDGE_LOOP ( 'NONE', ( #19656, #11735, #44024, #28947 ) ) ;
#2922 = EDGE_CURVE ( 'NONE', #20518, #8803, #19258, .T. ) ;
#2923 = EDGE_LOOP ( 'NONE', ( #52614, #13442, #55232, #24009 ) ) ;
#2924 = LINE ( 'NONE', #28228, #44797 ) ;
#2925 = DIRECTION ( 'NONE',  ( 0.007781995580012662783, 0.000000000000000000, -0.9999697198139514409 ) ) ;
#2926 = VECTOR ( 'NONE', #5765, 1000.000000000000000 ) ;
#2927 = CARTESIAN_POINT ( 'NONE',  ( -11.80822072027282132, 0.000000000000000000, 3.251184542293097390 ) ) ;
#2928 = EDGE_CURVE ( 'NONE', #4850, #1558, #10491, .T. ) ;
#2929 = ADVANCED_FACE ( 'NONE', ( #37411 ), #36312, .F. ) ;
#2930 = ADVANCED_FACE ( 'NONE', ( #1925 ), #54732, .F. ) ;
#2931 = VECTOR ( 'NONE', #10735, 1000.000000000000227 ) ;
#2932 = DIRECTION ( 'NONE',  ( 0.005002170337468016433, -0.7660444431189770143, -0.6427681459581293666 ) ) ;
#2933 = VECTOR ( 'NONE', #18950, 1000.000000000000227 ) ;
#2934 = CARTESIAN_POINT ( 'NONE',  ( -23.33693525117809386, 0.000000000000000000, 5.746789908705562944 ) ) ;
#2935 = DIRECTION ( 'NONE',  ( -0.005961354470445682716, -0.6427876096865404731, 0.7660212471507180654 ) ) ;
#2937 = EDGE_CURVE ( 'NONE', #32587, #49888, #53902, .T. ) ;
#2936 = ORIENTED_EDGE ( 'NONE', *, *, #46529, .T. ) ;
#2938 = DIRECTION ( 'NONE',  ( 0.9999697198139515519, 0.000000000000000000, 0.007781995580013368816 ) ) ;
#2939 = PLANE ( 'NONE',  #34163 ) ;
#2940 = VECTOR ( 'NONE', #5078, 1000.000000000000227 ) ;
#2941 = DIRECTION ( 'NONE',  ( 0.007781995580012662783, 0.000000000000000000, -0.9999697198139514409 ) ) ;
#2942 = VECTOR ( 'NONE', #45333, 999.9999999999998863 ) ;
#2943 = VERTEX_POINT ( 'NONE', #36590 ) ;
#2944 = CARTESIAN_POINT ( 'NONE',  ( -46.00906441860537655, 4.911362066797487103, -5.000000000000000000 ) ) ;
#2945 = PLANE ( 'NONE',  #8701 ) ;
#2946 = DIRECTION ( 'NONE',  ( 0.7660212471507180654, -0.6427876096865404731, 0.005961354470445141482 ) ) ;
#2947 = ORIENTED_EDGE ( 'NONE', *, *, #28986, .T. ) ;
#2948 = LINE ( 'NONE', #28831, #5967 ) ;
#2949 = AXIS2_PLACEMENT_3D ( 'NONE', #19117, #1792, #27952 ) ;
#2950 = ORIENTED_EDGE ( 'NONE', *, *, #25639, .T. ) ;
#2951 = AXIS2_PLACEMENT_3D ( 'NONE', #679, #52619, #23096 ) ;
#2952 = ADVANCED_FACE ( 'NONE', ( #28070 ), #53623, .F. ) ;
#2953 = VERTEX_POINT ( 'NONE', #41673 ) ;
#2954 = ORIENTED_EDGE ( 'NONE', *, *, #25341, .T. ) ;
#2955 = ORIENTED_EDGE ( 'NONE', *, *, #45559, .F. ) ;
#2956 = EDGE_CURVE ( 'NONE', #40825, #9112, #32054, .T. ) ;
#2957 = ORIENTED_EDGE ( 'NONE', *, *, #28999, .F. ) ;
#2958 = DIRECTION ( 'NONE',  ( -0.9999697198139514409, -0.000000000000000000, -0.007781995580013368816 ) ) ;
#2959 = EDGE_LOOP ( 'NONE', ( #42217, #35903, #17895, #34758 ) ) ;
#2960 = VECTOR ( 'NONE', #50948, 1000.000000000000000 ) ;
#2961 = EDGE_CURVE ( 'NONE', #19083, #21088, #50196, .T. ) ;
#2962 = ORIENTED_EDGE ( 'NONE', *, *, #16469, .F. ) ;
#2963 = CARTESIAN_POINT ( 'NONE',  ( -60.92294909528611413, 7.225036622302098976, 2.999999999999993339 ) ) ;
#2964 = ORIENTED_EDGE ( 'NONE', *, *, #47329, .T. ) ;
#2965 = VECTOR ( 'NONE', #31800, 999.9999999999998863 ) ;
#2966 = ORIENTED_EDGE ( 'NONE', *, *, #35287, .T. ) ;
#2967 = ADVANCED_FACE ( 'NONE', ( #33182 ), #50501, .F. ) ;
#2968 = DIRECTION ( 'NONE',  ( 0.007781995580012663651, -3.146120232559066537E-19, -0.9999697198139514409 ) ) ;
#2969 = CARTESIAN_POINT ( 'NONE',  ( -18.86354292863559579, 0.000000000000000000, 14.21804678658176080 ) ) ;
#2970 = LINE ( 'NONE', #50419, #13270 ) ;
#2971 = CARTESIAN_POINT ( 'NONE',  ( -12.65552006256329776, -0.1191753592594181482, 5.560586109843058011 ) ) ;
#2972 = VECTOR ( 'NONE', #20123, 999.9999999999998863 ) ;
#2973 = CARTESIAN_POINT ( 'NONE',  ( -17.73140113748535285, 0.000000000000000000, 13.85752530597602039 ) ) ;
#2974 = ORIENTED_EDGE ( 'NONE', *, *, #54492, .T. ) ;
#2975 = AXIS2_PLACEMENT_3D ( 'NONE', #51575, #8402, #13516 ) ;
#2976 = VECTOR ( 'NONE', #2912, 999.9999999999998863 ) ;
#2977 = ORIENTED_EDGE ( 'NONE', *, *, #26956, .F. ) ;
#2978 = CARTESIAN_POINT ( 'NONE',  ( -12.76491739461853925, 0.000000000000000000, 6.767733992039747015 ) ) ;
#2979 = DIRECTION ( 'NONE',  ( 0.000000000000000000, -1.000000000000000000, 0.000000000000000000 ) ) ;
#2980 = DIRECTION ( 'NONE',  ( 0.005961354470445682716, -0.6427876096865404731, -0.7660212471507180654 ) ) ;
#2981 = AXIS2_PLACEMENT_3D ( 'NONE', #1584, #27709, #18911 ) ;
#2982 = VECTOR ( 'NONE', #50286, 1000.000000000000227 ) ;
#2983 = CARTESIAN_POINT ( 'NONE',  ( -16.33317936670417225, 0.000000000000000000, 13.31440848639340224 ) ) ;
#2984 = DIRECTION ( 'NONE',  ( 0.007781995580012662783, 0.000000000000000000, -0.9999697198139514409 ) ) ;
#2985 = LINE ( 'NONE', #20027, #25899 ) ;
#2986 = ORIENTED_EDGE ( 'NONE', *, *, #28270, .F. ) ;
#2987 = CARTESIAN_POINT ( 'NONE',  ( -17.73140113748535285, 0.000000000000000000, 13.85752530597602039 ) ) ;
#2988 = ORIENTED_EDGE ( 'NONE', *, *, #29125, .F. ) ;
#2989 = CARTESIAN_POINT ( 'NONE',  ( -10.00813838035478298, 0.000000000000000000, 10.77830692922518452 ) ) ;
#2990 = CARTESIAN_POINT ( 'NONE',  ( -9.442067484779661513, -0.1191753592594197858, 10.59804618892231254 ) ) ;
#2991 = CARTESIAN_POINT ( 'NONE',  ( -18.19747506107908563, 0.000000000000000000, 14.03856424583689311 ) ) ;
#2992 = CARTESIAN_POINT ( 'NONE',  ( -16.03843301287463419, 0.000000000000000000, 9.448245625342075016 ) ) ;
#2993 = VECTOR ( 'NONE', #22135, 1000.000000000000227 ) ;
#2994 = CARTESIAN_POINT ( 'NONE',  ( -15.13495153988577968, 0.000000000000000000, 12.76973526769478084 ) ) ;
#2995 = VECTOR ( 'NONE', #14646, 999.9999999999998863 ) ;
#2996 = CARTESIAN_POINT ( 'NONE',  ( -20.17205406794205302, 1.095915999411505526, 4.482477119187890935 ) ) ;
#2997 = EDGE_LOOP ( 'NONE', ( #8233, #40338, #18781, #7169 ) ) ;
#2998 = ORIENTED_EDGE ( 'NONE', *, *, #49170, .T. ) ;
#2999 = LINE ( 'NONE', #20331, #9449 ) ;
#3000 = DIRECTION ( 'NONE',  ( -0.8531650599175529814, -0.4028455766673920135, 0.3313982828793697877 ) ) ;
#3001 = PLANE ( 'NONE',  #24276 ) ;
#3002 = VECTOR ( 'NONE', #42716, 1000.000000000000114 ) ;
#3003 = ADVANCED_FACE ( 'NONE', ( #45654 ), #7315, .F. ) ;
#3004 = PLANE ( 'NONE',  #134 ) ;
#3005 = CARTESIAN_POINT ( 'NONE',  ( -23.66772770479517618, 18.99370688441070953, -4.657437592157546824 ) ) ;
#3006 = AXIS2_PLACEMENT_3D ( 'NONE', #31023, #4920, #47517 ) ;
#3007 = EDGE_CURVE ( 'NONE', #29949, #485, #45375, .T. ) ;
#3008 = PLANE ( 'NONE',  #46303 ) ;
#3009 = ADVANCED_FACE ( 'NONE', ( #54446 ), #23796, .F. ) ;
#3010 = DIRECTION ( 'NONE',  ( 0.5364919789714477361, 0.6444004775717706579, 0.5449076811759711036 ) ) ;
#3011 = CARTESIAN_POINT ( 'NONE',  ( -19.95974260052372529, -4.403642575758163424, 4.493863725170102796 ) ) ;
#3012 = VECTOR ( 'NONE', #48995, 1000.000000000000227 ) ;
#3013 = CARTESIAN_POINT ( 'NONE',  ( -17.40439531852770827, -1.726076655135827531, 12.83624927358758150 ) ) ;
#3014 = ORIENTED_EDGE ( 'NONE', *, *, #44568, .F. ) ;
#3015 = VECTOR ( 'NONE', #7754, 1000.000000000000227 ) ;
#3016 = VECTOR ( 'NONE', #30105, 999.9999999999998863 ) ;
#3017 = ORIENTED_EDGE ( 'NONE', *, *, #22656, .F. ) ;
#3018 = VECTOR ( 'NONE', #21344, 1000.000000000000000 ) ;
#3019 = EDGE_LOOP ( 'NONE', ( #37350, #37916, #12693, #18271 ) ) ;
#3020 = VERTEX_POINT ( 'NONE', #32606 ) ;
#3021 = AXIS2_PLACEMENT_3D ( 'NONE', #14685, #49329, #511 ) ;
#3022 = VERTEX_POINT ( 'NONE', #36894 ) ;
#3023 = ORIENTED_EDGE ( 'NONE', *, *, #25164, .F. ) ;
#3024 = CARTESIAN_POINT ( 'NONE',  ( -12.57198921205559650, 0.000000000000000000, 7.677225556966255304 ) ) ;
#3025 = CARTESIAN_POINT ( 'NONE',  ( -12.70458494993575194, -0.1191753592594197858, 11.86531876794841978 ) ) ;
#3026 = CARTESIAN_POINT ( 'NONE',  ( -9.308034720146865837, 0.000000000000000000, 6.225298126311265889 ) ) ;
#3027 = ORIENTED_EDGE ( 'NONE', *, *, #20319, .T. ) ;
#3028 = ORIENTED_EDGE ( 'NONE', *, *, #21970, .T. ) ;
#3029 = VERTEX_POINT ( 'NONE', #15548 ) ;
#3030 = PLANE ( 'NONE',  #30447 ) ;
#3031 = ORIENTED_EDGE ( 'NONE', *, *, #36729, .T. ) ;
#3032 = EDGE_CURVE ( 'NONE', #9919, #40769, #54197, .T. ) ;
#3033 = CARTESIAN_POINT ( 'NONE',  ( -67.01351477598909412, -8.774122127324863740, -3.373741216800328235 ) ) ;
#3034 = AXIS2_PLACEMENT_3D ( 'NONE', #9972, #36111, #27280 ) ;
#3035 = B_SPLINE_CURVE_WITH_KNOTS ( 'NONE', 3,
 ( #45030, #32522, #1827, #23445, #5547, #44723, #19152, #41320, #36223, #23165, #36482 ),
 .UNSPECIFIED., .F., .F.,
 ( 4, 1, 1, 2, 2, 1, 4 ),
 ( 0.2333392773190904879, 0.2451180778799246229, 0.2480627780201330179, 0.2495351280902372015, 0.2502713031252893350, 0.2510074781603415239, 0.2568968784407584804 ),
 .UNSPECIFIED. ) ;
#3036 = EDGE_CURVE ( 'NONE', #46187, #16497, #51341, .T. ) ;
#3037 = LINE ( 'NONE', #46473, #16500 ) ;
#3038 = CARTESIAN_POINT ( 'NONE',  ( -12.66937793510369836, -0.1117717739993998177, 8.139590219543800131 ) ) ;
#3039 = EDGE_CURVE ( 'NONE', #547, #45990, #8174, .T. ) ;
#3040 = EDGE_LOOP ( 'NONE', ( #25753, #41866, #19410, #8096 ) ) ;
#3041 = CARTESIAN_POINT ( 'NONE',  ( -17.24885704207722270, -1.165603555308156736, 5.294927591850882465 ) ) ;
#3042 = VECTOR ( 'NONE', #26070, 999.9999999999998863 ) ;
#3043 = EDGE_LOOP ( 'NONE', ( #5014, #21818, #42478, #22197 ) ) ;
#3044 = CARTESIAN_POINT ( 'NONE',  ( -17.38673753587113424, 0.000000000000000000, 3.577103304334748213 ) ) ;
#3045 = ADVANCED_FACE ( 'NONE', ( #29175 ), #55578, .F. ) ;
#3047 = VECTOR ( 'NONE', #25229, 1000.000000000000227 ) ;
#3046 = CARTESIAN_POINT ( 'NONE',  ( -16.89925026227929195, -0.1191753592594197858, 13.49466922669627422 ) ) ;
#3048 = CARTESIAN_POINT ( 'NONE',  ( -12.83283603900386538, 0.1245042932765033361, 2.070363196038105702 ) ) ;
#3049 = CARTESIAN_POINT ( 'NONE',  ( -11.87243407472968926, 0.000000000000000000, 11.50246268866867361 ) ) ;
#3050 = DIRECTION ( 'NONE',  ( -0.9983709377222390602, -0.05705673239519656187, 0.000000000000000000 ) ) ;
#3051 = LINE ( 'NONE', #46487, #53022 ) ;
#3052 = CARTESIAN_POINT ( 'NONE',  ( -3.360905869600907092, 1.745854407020028306E-14, 3.600000000000000089 ) ) ;
#3053 = AXIS2_PLACEMENT_3D ( 'NONE', #49954, #2548, #49129 ) ;
#3054 = DIRECTION ( 'NONE',  ( 0.9999697198139515519, 0.000000000000000000, 0.007781995580013368816 ) ) ;
#3055 = ORIENTED_EDGE ( 'NONE', *, *, #35926, .F. ) ;
#3056 = FACE_OUTER_BOUND ( 'NONE', #42855, .T. ) ;
#3057 = ORIENTED_EDGE ( 'NONE', *, *, #42262, .F. ) ;
#3058 = AXIS2_PLACEMENT_3D ( 'NONE', #13884, #18146, #35469 ) ;
#3059 = LINE ( 'NONE', #10499, #1121 ) ;
#3060 = CARTESIAN_POINT ( 'NONE',  ( -22.40634380310664397, 0.000000000000000000, 5.584705972946605534 ) ) ;
#3061 = LINE ( 'NONE', #20941, #16905 ) ;
#3062 = LINE ( 'NONE', #3634, #51225 ) ;
#3063 = DIRECTION ( 'NONE',  ( 0.007781995580012663651, -3.146120232559066537E-19, -0.9999697198139514409 ) ) ;
#3064 = AXIS2_PLACEMENT_3D ( 'NONE', #35299, #43277, #22232 ) ;
#3065 = DIRECTION ( 'NONE',  ( -0.5364919789714478471, 0.6444004775717705469, -0.5449076811759709926 ) ) ;
#3066 = VECTOR ( 'NONE', #50377, 1000.000000000000227 ) ;
#3067 = DIRECTION ( 'NONE',  ( 1.000000000000000000, 0.000000000000000000, 0.000000000000000000 ) ) ;
#3068 = EDGE_LOOP ( 'NONE', ( #47046, #46184, #18788, #22466 ) ) ;
#3069 = FACE_OUTER_BOUND ( 'NONE', #44691, .T. ) ;
#3070 = DIRECTION ( 'NONE',  ( 0.5449076811759707706, 0.6444004775717708799, -0.5364919789714476250 ) ) ;
#3071 = DIRECTION ( 'NONE',  ( 0.007781995580012662783, 0.000000000000000000, -0.9999697198139514409 ) ) ;
#3072 = EDGE_CURVE ( 'NONE', #14373, #36044, #12141, .T. ) ;
#3073 = LINE ( 'NONE', #55599, #38188 ) ;
#3074 = DIRECTION ( 'NONE',  ( 0.000000000000000000, -1.000000000000000000, 0.000000000000000000 ) ) ;
#3075 = DIRECTION ( 'NONE',  ( -0.5449076811759708816, 0.6444004775717707689, 0.5364919789714475140 ) ) ;
#3076 = FACE_OUTER_BOUND ( 'NONE', #6412, .T. ) ;
#3077 = CARTESIAN_POINT ( 'NONE',  ( -27.99767448711536133, 0.000000000000000000, 7.557179307314289218 ) ) ;
#3078 = EDGE_CURVE ( 'NONE', #55515, #38688, #12994, .T. ) ;
#3080 = ADVANCED_FACE ( 'NONE', ( #17240 ), #56156, .F. ) ;
#3079 = DIRECTION ( 'NONE',  ( 0.5364919789714477361, 0.6444004775717706579, 0.5449076811759711036 ) ) ;
#3081 = EDGE_LOOP ( 'NONE', ( #39139, #29071, #8654, #36254 ) ) ;
#3082 = VECTOR ( 'NONE', #11779, 1000.000000000000114 ) ;
#3083 = CARTESIAN_POINT ( 'NONE',  ( -17.26532721389163072, 0.000000000000000000, 13.67648636611514590 ) ) ;
#3084 = PLANE ( 'NONE',  #20541 ) ;
#3085 = VERTEX_POINT ( 'NONE', #42791 ) ;
#3086 = AXIS2_PLACEMENT_3D ( 'NONE', #4649, #12620, #3798 ) ;
#3087 = CARTESIAN_POINT ( 'NONE',  ( -14.00280974873554030, 0.000000000000000000, 12.40921378708904044 ) ) ;
#3088 = DIRECTION ( 'NONE',  ( 0.5449076811759707706, 0.6444004775717708799, -0.5364919789714476250 ) ) ;
#3089 = VECTOR ( 'NONE', #48108, 1000.000000000000114 ) ;
#3090 = EDGE_LOOP ( 'NONE', ( #5536, #2164, #53372, #44752, #49270 ) ) ;
#3091 = VECTOR ( 'NONE', #39681, 1000.000000000000000 ) ;
#3092 = ORIENTED_EDGE ( 'NONE', *, *, #22942, .F. ) ;
#3093 = DIRECTION ( 'NONE',  ( 0.5364919789714477361, 0.6444004775717706579, 0.5449076811759711036 ) ) ;
#3094 = ADVANCED_FACE ( 'NONE', ( #37722 ), #33715, .F. ) ;
#3095 = ORIENTED_EDGE ( 'NONE', *, *, #13668, .T. ) ;
#3096 = ORIENTED_EDGE ( 'NONE', *, *, #20339, .T. ) ;
#3097 = ORIENTED_EDGE ( 'NONE', *, *, #53075, .T. ) ;
#3098 = DIRECTION ( 'NONE',  ( 0.000000000000000000, -1.000000000000000000, 0.000000000000000000 ) ) ;
#3099 = VECTOR ( 'NONE', #43967, 999.9999999999998863 ) ;
#3100 = LINE ( 'NONE', #29810, #46864 ) ;
#3101 = DIRECTION ( 'NONE',  ( 0.9999697198139515519, 0.000000000000000000, 0.007781995580013368816 ) ) ;
#3102 = VECTOR ( 'NONE', #38409, 1000.000000000000227 ) ;
#3103 = ORIENTED_EDGE ( 'NONE', *, *, #38974, .T. ) ;
#3104 = ORIENTED_EDGE ( 'NONE', *, *, #20854, .F. ) ;
#3105 = AXIS2_PLACEMENT_3D ( 'NONE', #32314, #36282, #32013 ) ;
#3106 = AXIS2_PLACEMENT_3D ( 'NONE', #19590, #15577, #54222 ) ;
#3107 = LINE ( 'NONE', #16180, #1228 ) ;
#3108 = DIRECTION ( 'NONE',  ( -0.9999697198139514409, -0.000000000000000000, -0.007781995580013368816 ) ) ;
#3109 = ORIENTED_EDGE ( 'NONE', *, *, #43723, .F. ) ;
#3110 = LINE ( 'NONE', #15343, #18247 ) ;
#3111 = ORIENTED_EDGE ( 'NONE', *, *, #14473, .F. ) ;
#3112 = LINE ( 'NONE', #20991, #23085 ) ;
#3113 = LINE ( 'NONE', #29234, #50267 ) ;
#3114 = ORIENTED_EDGE ( 'NONE', *, *, #51577, .T. ) ;
#3115 = CARTESIAN_POINT ( 'NONE',  ( 5.284365508485809215, -1.088618427183434934, -2.393569053917001810 ) ) ;
#3116 = EDGE_CURVE ( 'NONE', #39305, #54919, #7913, .T. ) ;
#3117 = VECTOR ( 'NONE', #13013, 1000.000000000000000 ) ;
#3118 = LINE ( 'NONE', #55103, #11872 ) ;
#3119 = ORIENTED_EDGE ( 'NONE', *, *, #2464, .F. ) ;
#3120 = CARTESIAN_POINT ( 'NONE',  ( -20.26176469941677993, 0.000000000000000000, 14.76116360616437895 ) ) ;
#3122 = VECTOR ( 'NONE', #46264, 1000.000000000000227 ) ;
#3121 = CARTESIAN_POINT ( 'NONE',  ( -15.98897725045028650, -1.327505506330656893, 5.071256179035622758 ) ) ;
#3123 = DIRECTION ( 'NONE',  ( -0.5364919789714478471, 0.6444004775717705469, -0.5449076811759709926 ) ) ;
#3124 = ORIENTED_EDGE ( 'NONE', *, *, #25835, .F. ) ;
#3125 = VECTOR ( 'NONE', #18742, 999.9999999999998863 ) ;
#3126 = ADVANCED_FACE ( 'NONE', ( #38845 ), #12712, .F. ) ;
#3127 = FACE_OUTER_BOUND ( 'NONE', #39854, .T. ) ;
#3128 = CARTESIAN_POINT ( 'NONE',  ( -28.92982233430281980, 0.000000000000000000, 7.919257187036034651 ) ) ;
#3129 = CARTESIAN_POINT ( 'NONE',  ( -15.13495153988577968, 0.000000000000000000, 12.76973526769478084 ) ) ;
#3130 = DIRECTION ( 'NONE',  ( 0.7660212471507180654, -0.6427876096865404731, 0.005961354470445141482 ) ) ;
#3131 = EDGE_CURVE ( 'NONE', #28798, #27319, #46486, .T. ) ;
#3132 = CARTESIAN_POINT ( 'NONE',  ( -20.54049170961573267, 0.000000000000000000, 4.660556269540326646 ) ) ;
#3134 = EDGE_CURVE ( 'NONE', #24424, #39217, #55884, .T. ) ;
#3133 = CARTESIAN_POINT ( 'NONE',  ( -15.87975247367846166, 0.000000000000000000, 2.850166870931599927 ) ) ;
#3135 = CARTESIAN_POINT ( 'NONE',  ( -68.97404544921916170, -9.738005235595720066, -6.894786738962547901 ) ) ;
#3136 = VECTOR ( 'NONE', #37095, 1000.000000000000227 ) ;
#3137 = ORIENTED_EDGE ( 'NONE', *, *, #32947, .F. ) ;
#3138 = DIRECTION ( 'NONE',  ( 0.007781995580012663651, 0.000000000000000000, -0.9999697198139515519 ) ) ;
#3139 = DIRECTION ( 'NONE',  ( -0.7660212471507179544, -0.6427876096865405842, -0.005961354470445141482 ) ) ;
#3140 = CARTESIAN_POINT ( 'NONE',  ( -17.93139508144814442, 0.000000000000000000, 13.85596890686001537 ) ) ;
#3141 = EDGE_LOOP ( 'NONE', ( #28178, #47376, #2053, #11930 ) ) ;
#3142 = VECTOR ( 'NONE', #44207, 1000.000000000000000 ) ;
#3143 = DIRECTION ( 'NONE',  ( 0.9999697198139515519, 0.000000000000000000, 0.007781995580013368816 ) ) ;
#3144 = EDGE_CURVE ( 'NONE', #5924, #13188, #16987, .T. ) ;
#3145 = LINE ( 'NONE', #50840, #34510 ) ;
#3146 = AXIS2_PLACEMENT_3D ( 'NONE', #45199, #6300, #44919 ) ;
#3147 = ADVANCED_FACE ( 'NONE', ( #25772 ), #55044, .T. ) ;
#3148 = DIRECTION ( 'NONE',  ( -0.7660212471507179544, -0.6427876096865405842, -0.005961354470445141482 ) ) ;
#3149 = DIRECTION ( 'NONE',  ( -0.005961354470445682716, -0.6427876096865404731, 0.7660212471507180654 ) ) ;
#3150 = EDGE_CURVE ( 'NONE', #5616, #32386, #20381, .T. ) ;
#3151 = PLANE ( 'NONE',  #12051 ) ;
#3152 = ORIENTED_EDGE ( 'NONE', *, *, #56206, .T. ) ;
#3153 = VECTOR ( 'NONE', #27066, 1000.000000000000000 ) ;
#3154 = VECTOR ( 'NONE', #26834, 1000.000000000000000 ) ;
#3155 = ORIENTED_EDGE ( 'NONE', *, *, #46332, .F. ) ;
#3156 = SHAPE_REPRESENTATION ( 'Steel Pivot Pin Shaft', ( #2610 ), #1760 ) ;
#3157 = DIRECTION ( 'NONE',  ( -0.005961354470445682716, -0.6427876096865404731, 0.7660212471507180654 ) ) ;
#3158 = CARTESIAN_POINT ( 'NONE',  ( -63.00984630926863161, 1.788483511016180305, 2.999999999999993339 ) ) ;
#3159 = EDGE_CURVE ( 'NONE', #52910, #43897, #16135, .T. ) ;
#3160 = EDGE_LOOP ( 'NONE', ( #36097, #10100, #38673, #5435 ) ) ;
#3161 = CARTESIAN_POINT ( 'NONE',  ( -15.96710241509184058, -0.1191753592594218814, 13.13259134697452879 ) ) ;
#3162 = ORIENTED_EDGE ( 'NONE', *, *, #44223, .F. ) ;
#3163 = FACE_OUTER_BOUND ( 'NONE', #1568, .T. ) ;
#3164 = AXIS2_PLACEMENT_3D ( 'NONE', #43944, #53034, #34881 ) ;
#3165 = ADVANCED_FACE ( 'NONE', ( #11849, #24934, #38254 ), #42254, .F. ) ;
#3166 = VERTEX_POINT ( 'NONE', #55296 ) ;
#3167 = VERTEX_POINT ( 'NONE', #770 ) ;
#3168 = VERTEX_POINT ( 'NONE', #43384 ) ;
#3169 = VECTOR ( 'NONE', #18339, 999.9999999999998863 ) ;
#3170 = DIRECTION ( 'NONE',  ( 0.007781995580012663651, 0.000000000000000000, -0.9999697198139515519 ) ) ;
#3171 = DIRECTION ( 'NONE',  ( 0.007781995580012663651, -3.146120232559066537E-19, -0.9999697198139514409 ) ) ;
#3172 = VECTOR ( 'NONE', #33044, 1000.000000000000227 ) ;
#3173 = DIRECTION ( 'NONE',  ( 0.007781995580012663651, -3.146120232559066537E-19, -0.9999697198139514409 ) ) ;
#3174 = LINE ( 'NONE', #49769, #14771 ) ;
#3175 = VECTOR ( 'NONE', #55438, 999.9999999999998863 ) ;
#3176 = ORIENTED_EDGE ( 'NONE', *, *, #1230, .T. ) ;
#3177 = EDGE_LOOP ( 'NONE', ( #23035, #7420, #52955, #11886, #36290 ) ) ;
#3178 = VERTEX_POINT ( 'NONE', #9591 ) ;
#3179 = VECTOR ( 'NONE', #19684, 999.9999999999998863 ) ;
#3180 = CARTESIAN_POINT ( 'NONE',  ( -20.54049170961573267, 0.000000000000000000, 4.660556269540326646 ) ) ;
#3181 = VECTOR ( 'NONE', #26205, 1000.000000000000227 ) ;
#3182 = FACE_OUTER_BOUND ( 'NONE', #22117, .T. ) ;
#3183 = ORIENTED_EDGE ( 'NONE', *, *, #52450, .T. ) ;
#3184 = VECTOR ( 'NONE', #23070, 1000.000000000000000 ) ;
#3185 = CARTESIAN_POINT ( 'NONE',  ( -19.60834386242827776, 0.000000000000000000, 4.298478389818581213 ) ) ;
#3186 = VERTEX_POINT ( 'NONE', #36008 ) ;
#3187 = CARTESIAN_POINT ( 'NONE',  ( -19.27689971179358253, 0.000000000000000000, 7.625046393098118713 ) ) ;
#3188 = DIRECTION ( 'NONE',  ( 0.9999697198139515519, 0.000000000000000000, 0.007781995580013368816 ) ) ;
#3189 = AXIS2_PLACEMENT_3D ( 'NONE', #52789, #31223, #31529 ) ;
#3190 = EDGE_LOOP ( 'NONE', ( #23473, #4661, #4874, #25203 ) ) ;
#3191 = DIRECTION ( 'NONE',  ( 0.7660212471507180654, -0.6427876096865404731, 0.005961354470445141482 ) ) ;
#3192 = EDGE_CURVE ( 'NONE', #54019, #5570, #53317, .T. ) ;
#3193 = VERTEX_POINT ( 'NONE', #31457 ) ;
#3194 = VECTOR ( 'NONE', #41765, 999.9999999999998863 ) ;
#3195 = FACE_OUTER_BOUND ( 'NONE', #20613, .T. ) ;
#3196 = VECTOR ( 'NONE', #12858, 1000.000000000000227 ) ;
#3197 = FACE_OUTER_BOUND ( 'NONE', #32327, .T. ) ;
#3198 = CARTESIAN_POINT ( 'NONE',  ( -11.80402901237825652, 0.000000000000000000, 2.712559079740358481 ) ) ;
#3199 = CARTESIAN_POINT ( 'NONE',  ( -15.13495153988577968, 0.000000000000000000, 12.76973526769478084 ) ) ;
#3200 = FACE_OUTER_BOUND ( 'NONE', #36237, .T. ) ;
#3201 = DIRECTION ( 'NONE',  ( -0.6427681459581293666, -0.7660444431189770143, -0.005002170337467561935 ) ) ;
#3202 = VERTEX_POINT ( 'NONE', #48771 ) ;
#3203 = EDGE_CURVE ( 'NONE', #52569, #44385, #40231, .T. ) ;
#3204 = EDGE_CURVE ( 'NONE', #39994, #11098, #1319, .T. ) ;
#3205 = ORIENTED_EDGE ( 'NONE', *, *, #34669, .T. ) ;
#3206 = PLANE ( 'NONE',  #8309 ) ;
#3207 = CARTESIAN_POINT ( 'NONE',  ( -12.32763377081944789, 1.743523803501506375, 1.414775798601282331 ) ) ;
#3208 = LINE ( 'NONE', #15695, #30442 ) ;
#3209 = DIRECTION ( 'NONE',  ( 0.9999697198139515519, 0.000000000000000000, 0.007781995580013368816 ) ) ;
#3211 = ADVANCED_FACE ( 'NONE', ( #49026 ), #9870, .F. ) ;
#3210 = LINE ( 'NONE', #46947, #14326 ) ;
#3212 = VECTOR ( 'NONE', #48720, 1000.000000000000227 ) ;
#3213 = FACE_OUTER_BOUND ( 'NONE', #44582, .T. ) ;
#3214 = ORIENTED_EDGE ( 'NONE', *, *, #24753, .T. ) ;
#3215 = AXIS2_PLACEMENT_3D ( 'NONE', #595, #13635, #39779 ) ;
#3216 = DIRECTION ( 'NONE',  ( 0.007781995580012663651, -3.146120232559066537E-19, -0.9999697198139514409 ) ) ;
#3217 = CARTESIAN_POINT ( 'NONE',  ( 2.072287782118878319, 0.000000000000000000, -2.950529333540147015 ) ) ;
#3218 = EDGE_LOOP ( 'NONE', ( #44652, #1493, #28736, #47844 ) ) ;
#3219 = CARTESIAN_POINT ( 'NONE',  ( -21.92051860787708506, 5.305366725996512045, 14.10300561120236829 ) ) ;
#3220 = VECTOR ( 'NONE', #52177, 1000.000000000000227 ) ;
#3221 = EDGE_LOOP ( 'NONE', ( #24910, #12552, #9508, #26640 ) ) ;
#3222 = PLANE ( 'NONE',  #31625 ) ;
#3223 = CARTESIAN_POINT ( 'NONE',  ( -24.26908309836554878, 0.000000000000000000, 6.108867788427308376 ) ) ;
#3224 = EDGE_CURVE ( 'NONE', #21409, #19068, #24895, .T. ) ;
#3225 = VECTOR ( 'NONE', #30101, 999.9999999999998863 ) ;
#3226 = CARTESIAN_POINT ( 'NONE',  ( -19.59569683186026268, 0.000000000000000000, 14.58168106541950948 ) ) ;
#3227 = LINE ( 'NONE', #37042, #11485 ) ;
#3228 = EDGE_CURVE ( 'NONE', #33629, #48984, #22375, .T. ) ;
#3229 = CARTESIAN_POINT ( 'NONE',  ( -67.91288919400373914, 1.999999999999992673, -8.053057903404074125 ) ) ;
#3230 = VERTEX_POINT ( 'NONE', #52714 ) ;
#3231 = VECTOR ( 'NONE', #27577, 1000.000000000000227 ) ;
#3232 = VECTOR ( 'NONE', #6092, 999.9999999999998863 ) ;
#3233 = ORIENTED_EDGE ( 'NONE', *, *, #22010, .F. ) ;
#3234 = CARTESIAN_POINT ( 'NONE',  ( -67.13585797164662949, -0.6008874593650106455, 1.683582515887796172 ) ) ;
#3235 = FACE_OUTER_BOUND ( 'NONE', #53824, .T. ) ;
#3236 = FACE_OUTER_BOUND ( 'NONE', #25218, .T. ) ;
#3237 = AXIS2_PLACEMENT_3D ( 'NONE', #27969, #23963, #15190 ) ;
#3238 = CARTESIAN_POINT ( 'NONE',  ( -17.74404816805336793, 0.000000000000000000, 3.574322630375089460 ) ) ;
#3239 = ADVANCED_FACE ( 'NONE', ( #31723 ), #44479, .F. ) ;
#3241 = DIRECTION ( 'NONE',  ( 0.000000000000000000, -1.000000000000000000, 0.000000000000000000 ) ) ;
#3240 = AXIS2_PLACEMENT_3D ( 'NONE', #51092, #25274, #47395 ) ;
#3242 = CARTESIAN_POINT ( 'NONE',  ( -24.27063949748155380, 0.000000000000000000, 6.308861732390097288 ) ) ;
#3243 = VECTOR ( 'NONE', #8785, 1000.000000000000227 ) ;
#3244 = ORIENTED_EDGE ( 'NONE', *, *, #54262, .F. ) ;
#3245 = LINE ( 'NONE', #33904, #42826 ) ;
#3246 = AXIS2_PLACEMENT_3D ( 'NONE', #12349, #21117, #50672 ) ;
#3247 = CARTESIAN_POINT ( 'NONE',  ( -12.15193928448664629, -0.1191753592594197858, 1.501852324026012209 ) ) ;
#3248 = VECTOR ( 'NONE', #32969, 999.9999999999998863 ) ;
#3249 = LINE ( 'NONE', #55470, #45951 ) ;
#3250 = EDGE_LOOP ( 'NONE', ( #6976, #32229, #2742, #44453 ) ) ;
#3251 = PLANE ( 'NONE',  #10255 ) ;
#3252 = LINE ( 'NONE', #42695, #44967 ) ;
#3253 = DIRECTION ( 'NONE',  ( 0.000000000000000000, 0.000000000000000000, 1.000000000000000000 ) ) ;
#3254 = VERTEX_POINT ( 'NONE', #9020 ) ;
#3255 = DIRECTION ( 'NONE',  ( 0.007781995580012663651, 0.000000000000000000, -0.9999697198139515519 ) ) ;
#3256 = ORIENTED_EDGE ( 'NONE', *, *, #41988, .F. ) ;
#3257 = AXIS2_PLACEMENT_3D ( 'NONE', #65, #56049, #26482 ) ;
#3258 = ORIENTED_EDGE ( 'NONE', *, *, #48896, .F. ) ;
#3259 = ORIENTED_EDGE ( 'NONE', *, *, #22885, .F. ) ;
#3260 = EDGE_LOOP ( 'NONE', ( #43362, #36796, #10568, #21821 ) ) ;
#3261 = DIRECTION ( 'NONE',  ( 0.5449076811759707706, 0.6444004775717708799, -0.5364919789714476250 ) ) ;
#3262 = AXIS2_PLACEMENT_3D ( 'NONE', #3217, #29053, #8313 ) ;
#3264 = EDGE_CURVE ( 'NONE', #42364, #52074, #22911, .T. ) ;
#3263 = ORIENTED_EDGE ( 'NONE', *, *, #15711, .F. ) ;
#3265 = ORIENTED_EDGE ( 'NONE', *, *, #16683, .T. ) ;
#3266 = CARTESIAN_POINT ( 'NONE',  ( -15.87975247367846166, 0.000000000000000000, 2.850166870931599927 ) ) ;
#3267 = ORIENTED_EDGE ( 'NONE', *, *, #47021, .F. ) ;
#3268 = VECTOR ( 'NONE', #33871, 1000.000000000000227 ) ;
#3269 = EDGE_CURVE ( 'NONE', #6150, #1131, #31147, .T. ) ;
#3270 = ORIENTED_EDGE ( 'NONE', *, *, #27910, .T. ) ;
#3271 = VECTOR ( 'NONE', #11860, 1000.000000000000227 ) ;
#3272 = VECTOR ( 'NONE', #12374, 1000.000000000000227 ) ;
#3273 = DIRECTION ( 'NONE',  ( 0.000000000000000000, -0.000000000000000000, -1.000000000000000000 ) ) ;
#3274 = LINE ( 'NONE', #41869, #26685 ) ;
#3275 = ADVANCED_FACE ( 'NONE', ( #21789 ), #18361, .F. ) ;
#3276 = LINE ( 'NONE', #50112, #21456 ) ;
#3277 = CARTESIAN_POINT ( 'NONE',  ( -12.66060981992452028, -3.432230869623160263, 7.232618128541711933 ) ) ;
#3278 =( NAMED_UNIT ( * ) PLANE_ANGLE_UNIT ( ) SI_UNIT ( $, .RADIAN. ) );
#3279 = ORIENTED_EDGE ( 'NONE', *, *, #10440, .F. ) ;
#3280 = EDGE_CURVE ( 'NONE', #20837, #35428, #4748, .T. ) ;
#3281 = VECTOR ( 'NONE', #53110, 999.9999999999998863 ) ;
#3282 = EDGE_CURVE ( 'NONE', #55101, #50478, #35161, .T. ) ;
#3283 = EDGE_CURVE ( 'NONE', #23095, #33080, #52458, .T. ) ;
#3284 = ORIENTED_EDGE ( 'NONE', *, *, #29779, .T. ) ;
#3285 = AXIS2_PLACEMENT_3D ( 'NONE', #54437, #15535, #25215 ) ;
#3286 = CARTESIAN_POINT ( 'NONE',  ( -24.27063949748155380, 0.000000000000000000, 6.308861732390097288 ) ) ;
#3287 = CARTESIAN_POINT ( 'NONE',  ( -10.89774764673834895, 0.000000000000000000, 5.674268529338492684 ) ) ;
#3288 = EDGE_CURVE ( 'NONE', #51394, #40825, #9283, .T. ) ;
#3289 = VECTOR ( 'NONE', #3171, 1000.000000000000227 ) ;
#3290 = CARTESIAN_POINT ( 'NONE',  ( 2.072287782118878319, 0.000000000000000000, -2.950529333540147015 ) ) ;
#3291 = VECTOR ( 'NONE', #16278, 999.9999999999998863 ) ;
#3292 = DIRECTION ( 'NONE',  ( 0.005961354470445682716, -0.6427876096865404731, -0.7660212471507180654 ) ) ;
#3293 = CARTESIAN_POINT ( 'NONE',  ( -12.71762380888595700, -5.213152330870666873, 1.654951243671639372 ) ) ;
#3294 = DIRECTION ( 'NONE',  ( 0.005002170337468016433, -0.7660444431189770143, -0.6427681459581293666 ) ) ;
#3295 = EDGE_LOOP ( 'NONE', ( #4257, #36445, #3014, #14840 ) ) ;
#3296 = DIRECTION ( 'NONE',  ( 0.7660212471507180654, -0.6427876096865404731, 0.005961354470445141482 ) ) ;
#3297 = FACE_OUTER_BOUND ( 'NONE', #42415, .T. ) ;
#3298 = ORIENTED_EDGE ( 'NONE', *, *, #15621, .T. ) ;
#3299 = DIRECTION ( 'NONE',  ( 0.000000000000000000, -0.000000000000000000, -1.000000000000000000 ) ) ;
#3300 = DIRECTION ( 'NONE',  ( -0.6427681459581293666, -0.7660444431189770143, -0.005002170337467561935 ) ) ;
#3301 = DIRECTION ( 'NONE',  ( 0.2426528472758542054, 0.7422098413412800966, 0.6246952433987894571 ) ) ;
#3302 = EDGE_CURVE ( 'NONE', #33305, #52665, #43923, .T. ) ;
#3303 = DIRECTION ( 'NONE',  ( -0.005961354470445682716, -0.6427876096865404731, 0.7660212471507180654 ) ) ;
#3304 = CARTESIAN_POINT ( 'NONE',  ( -27.06630483948590893, -0.1191753592594197858, 7.295098399573937797 ) ) ;
#3305 = AXIS2_PLACEMENT_3D ( 'NONE', #10676, #41318, #14371 ) ;
#3306 = EDGE_CURVE ( 'NONE', #36173, #14307, #35413, .T. ) ;
#3307 = ORIENTED_EDGE ( 'NONE', *, *, #34691, .F. ) ;
#3308 = VERTEX_POINT ( 'NONE', #32811 ) ;
#3309 = EDGE_CURVE ( 'NONE', #4402, #17065, #10425, .T. ) ;
#3310 = LINE ( 'NONE', #56111, #16705 ) ;
#3311 = CARTESIAN_POINT ( 'NONE',  ( -19.03013902487656495, 0.2864062442990046309, 4.743314820996812564 ) ) ;
#3312 = LINE ( 'NONE', #37109, #33320 ) ;
#3313 = VECTOR ( 'NONE', #5201, 999.9999999999998863 ) ;
#3314 = EDGE_CURVE ( 'NONE', #18318, #35555, #54665, .T. ) ;
#3315 = DIRECTION ( 'NONE',  ( 0.005961354470445682716, -0.6427876096865404731, -0.7660212471507180654 ) ) ;
#3316 = VECTOR ( 'NONE', #3388, 1000.000000000000227 ) ;
#3317 = DIRECTION ( 'NONE',  ( 0.005002170337468016433, -0.7660444431189770143, -0.6427681459581293666 ) ) ;
#3318 = CARTESIAN_POINT ( 'NONE',  ( -13.01064681732981398, 25.14657540356444088, -3.506683753893632183 ) ) ;
#3319 = LINE ( 'NONE', #20643, #46461 ) ;
#3320 = EDGE_CURVE ( 'NONE', #3819, #39923, #41619, .T. ) ;
#3322 = VECTOR ( 'NONE', #6718, 1000.000000000000227 ) ;
#3321 = CARTESIAN_POINT ( 'NONE',  ( -10.44173291041310847, 0.000000000000000000, 6.785813550879795208 ) ) ;
#3323 = CARTESIAN_POINT ( 'NONE',  ( -69.84290760269591658, -9.703778660409923873, -9.299316846403153036 ) ) ;
#3324 = CARTESIAN_POINT ( 'NONE',  ( -21.47341775636118655, -0.1191753592594197858, 5.122631121243466090 ) ) ;
#3325 = ORIENTED_EDGE ( 'NONE', *, *, #9204, .T. ) ;
#3326 = CARTESIAN_POINT ( 'NONE',  ( -14.17742873937475423, 4.495856970884013037, 2.045485145604081012 ) ) ;
#3327 = ORIENTED_EDGE ( 'NONE', *, *, #36979, .T. ) ;
#3328 = VECTOR ( 'NONE', #20303, 1000.000000000000000 ) ;
#3329 = VECTOR ( 'NONE', #39144, 1000.000000000000000 ) ;
#3330 = ORIENTED_EDGE ( 'NONE', *, *, #8084, .F. ) ;
#3331 = VECTOR ( 'NONE', #37226, 1000.000000000000227 ) ;
#3332 = EDGE_LOOP ( 'NONE', ( #33829, #36635, #20089, #6403 ) ) ;
#3333 = ORIENTED_EDGE ( 'NONE', *, *, #7758, .T. ) ;
#3334 = ORIENTED_EDGE ( 'NONE', *, *, #28833, .T. ) ;
#3335 = PLANE ( 'NONE',  #53205 ) ;
#3336 = LINE ( 'NONE', #46458, #12081 ) ;
#3337 = CARTESIAN_POINT ( 'NONE',  ( -69.47171822008920117, -0.5008832641493313753, 7.490399608206209869 ) ) ;
#3338 = ORIENTED_EDGE ( 'NONE', *, *, #31775, .T. ) ;
#3339 = CARTESIAN_POINT ( 'NONE',  ( 2.072287782118878319, 0.000000000000000000, -2.950529333540147015 ) ) ;
#3340 = VERTEX_POINT ( 'NONE', #14666 ) ;
#3341 = DIRECTION ( 'NONE',  ( 0.000000000000000000, -0.000000000000000000, -1.000000000000000000 ) ) ;
#3342 = ORIENTED_EDGE ( 'NONE', *, *, #41815, .F. ) ;
#3343 = VECTOR ( 'NONE', #17600, 999.9999999999998863 ) ;
#3344 = CARTESIAN_POINT ( 'NONE',  ( -66.62858553107250259, -8.730383453837468721, -1.359962337618603412 ) ) ;
#3345 = DIRECTION ( 'NONE',  ( 0.005002170337468016433, -0.7660444431189770143, -0.6427681459581293666 ) ) ;
#3346 = CARTESIAN_POINT ( 'NONE',  ( -69.43561177275644525, -9.791245164465275153, -7.501782499249458169 ) ) ;
#3347 = ORIENTED_EDGE ( 'NONE', *, *, #48896, .T. ) ;
#3348 = FACE_OUTER_BOUND ( 'NONE', #55072, .T. ) ;
#3349 = B_SPLINE_CURVE_WITH_KNOTS ( 'NONE', 3,
 ( #54065, #27957, #496, #771, #22637, #34862 ),
 .UNSPECIFIED., .F., .F.,
 ( 4, 2, 4 ),
 ( 0.3753454237082048950, 0.4999999468611081022, 0.6246544700140113093 ),
 .UNSPECIFIED. ) ;
#3350 = ORIENTED_EDGE ( 'NONE', *, *, #1814, .F. ) ;
#3351 = ADVANCED_FACE ( 'NONE', ( #40798 ), #1869, .F. ) ;
#3352 = ADVANCED_FACE ( 'NONE', ( #10958 ), #31991, .F. ) ;
#3353 = B_SPLINE_CURVE_WITH_KNOTS ( 'NONE', 3,
 ( #24155, #20137, #37194, #54790, #41474, #2553, #19875, #46543, #55938, #42850, #22116, #30081, #43679, #47692, #30661, #17579, #38895, #26116, #30908, #47961 ),
 .UNSPECIFIED., .F., .F.,
 ( 4, 2, 2, 2, 2, 2, 2, 2, 2, 4 ),
 ( 6.071532165918824830E-18, 0.001980665692890082059, 0.003961331385780158046, 0.005941997078670233599, 0.006932329925115271810, 0.007922662771560309153, 0.009903328464450387308, 0.01188399415734046199, 0.01386465985023053668, 0.01584532554312061484 ),
 .UNSPECIFIED. ) ;
#3354 = CARTESIAN_POINT ( 'NONE',  ( -17.99722147484924051, 0.000000000000000000, 3.772358433381585385 ) ) ;
#3355 = VECTOR ( 'NONE', #10923, 999.9999999999998863 ) ;
#3356 = DIRECTION ( 'NONE',  ( 0.7660212471507180654, -0.6427876096865404731, 0.005961354470445141482 ) ) ;
#3357 = EDGE_CURVE ( 'NONE', #50871, #10700, #50130, .T. ) ;
#3358 = LINE ( 'NONE', #24627, #10647 ) ;
#3359 = VECTOR ( 'NONE', #47213, 1000.000000000000227 ) ;
#3360 = CARTESIAN_POINT ( 'NONE',  ( -16.33317936670417225, 0.000000000000000000, 13.31440848639340224 ) ) ;
#3361 = CARTESIAN_POINT ( 'NONE',  ( -1.246832498358330099E-15, 2.000000000000000000, 0.000000000000000000 ) ) ;
#3362 = CARTESIAN_POINT ( 'NONE',  ( -14.03793453906542688, -0.1191753592594188005, 4.072499561507972210 ) ) ;
#3363 = DIRECTION ( 'NONE',  ( -0.7886751345948130876, 0.2113248654051844977, 0.5773502691896263972 ) ) ;
#3364 = PLANE ( 'NONE',  #24748 ) ;
#3365 = ORIENTED_EDGE ( 'NONE', *, *, #16323, .F. ) ;
#3366 = CARTESIAN_POINT ( 'NONE',  ( -13.73672976910459909, 0.000000000000000000, 12.22661844811216270 ) ) ;
#3367 = ORIENTED_EDGE ( 'NONE', *, *, #9914, .F. ) ;
#3368 = AXIS2_PLACEMENT_3D ( 'NONE', #36891, #41125, #54730 ) ;
#3369 = DIRECTION ( 'NONE',  ( 0.000000000000000000, -1.000000000000000000, 0.000000000000000000 ) ) ;
#3370 = CARTESIAN_POINT ( 'NONE',  ( -17.88454542038633122, 0.000000000000000000, 7.835888072364936008 ) ) ;
#3371 = CARTESIAN_POINT ( 'NONE',  ( -19.59569683186026268, 0.000000000000000000, 14.58168106541950948 ) ) ;
#3372 = FACE_OUTER_BOUND ( 'NONE', #26240, .T. ) ;
#3373 = LINE ( 'NONE', #17542, #6853 ) ;
#3374 = AXIS2_PLACEMENT_3D ( 'NONE', #20265, #51217, #6961 ) ;
#3375 = DIRECTION ( 'NONE',  ( 0.9659258262890692004, -0.2588190451025176864, 0.000000000000000000 ) ) ;
#3376 = ORIENTED_EDGE ( 'NONE', *, *, #44258, .T. ) ;
#3377 = FACE_OUTER_BOUND ( 'NONE', #36993, .T. ) ;
#3378 = CARTESIAN_POINT ( 'NONE',  ( -9.075990533167328067, 0.000000000000000000, 10.41622904950343909 ) ) ;
#3379 = CARTESIAN_POINT ( 'NONE',  ( -15.52687229411750813, 0.000000000000000000, 3.422251192111810170 ) ) ;
#3380 = CARTESIAN_POINT ( 'NONE',  ( -13.09628788616446116, -0.1134144341942139589, 1.868669391131170698 ) ) ;
#3381 = CARTESIAN_POINT ( 'NONE',  ( -14.01545677930355183, 0.000000000000000000, 2.126011111488108174 ) ) ;
#3382 = DIRECTION ( 'NONE',  ( 0.007781995580012663651, -3.146120232559066537E-19, -0.9999697198139514409 ) ) ;
#3383 = ADVANCED_FACE ( 'NONE', ( #23480 ), #11239, .F. ) ;
#3384 = LINE ( 'NONE', #34586, #54928 ) ;
#3385 = DIRECTION ( 'NONE',  ( 0.000000000000000000, 1.000000000000000000, 0.000000000000000000 ) ) ;
#3386 = ORIENTED_EDGE ( 'NONE', *, *, #19417, .F. ) ;
#3387 = CARTESIAN_POINT ( 'NONE',  ( -10.47421230394850866, 0.000000000000000000, 10.95934586908605723 ) ) ;
#3388 = DIRECTION ( 'NONE',  ( 0.007781995580012662783, 0.000000000000000000, -0.9999697198139514409 ) ) ;
#3389 = ORIENTED_EDGE ( 'NONE', *, *, #27915, .F. ) ;
#3390 = ADVANCED_FACE ( 'NONE', ( #28565 ), #44769, .F. ) ;
#3391 = ORIENTED_EDGE ( 'NONE', *, *, #39249, .F. ) ;
#3392 = LINE ( 'NONE', #37451, #42835 ) ;
#3393 = EDGE_CURVE ( 'NONE', #3819, #12179, #10126, .T. ) ;
#3394 = ORIENTED_EDGE ( 'NONE', *, *, #2477, .T. ) ;
#3395 = EDGE_CURVE ( 'NONE', #44587, #48743, #24028, .T. ) ;
#3396 = ORIENTED_EDGE ( 'NONE', *, *, #41729, .F. ) ;
#3397 = DIRECTION ( 'NONE',  ( -0.5364919789714478471, 0.6444004775717705469, -0.5449076811759709926 ) ) ;
#3398 = VECTOR ( 'NONE', #2716, 1000.000000000000000 ) ;
#3399 = VERTEX_POINT ( 'NONE', #23210 ) ;
#3400 = ORIENTED_EDGE ( 'NONE', *, *, #34127, .T. ) ;
#3401 = ORIENTED_EDGE ( 'NONE', *, *, #40228, .F. ) ;
#3402 = CARTESIAN_POINT ( 'NONE',  ( -25.20200914511100265, -0.1191753592594197858, 6.570942640130446932 ) ) ;
#3403 = CARTESIAN_POINT ( 'NONE',  ( -28.92982233430281980, 0.000000000000000000, 7.919257187036034651 ) ) ;
#3404 = DIRECTION ( 'NONE',  ( -0.005002170337468016433, -0.7660444431189770143, 0.6427681459581293666 ) ) ;
#3405 = AXIS2_PLACEMENT_3D ( 'NONE', #26830, #13493, #44156 ) ;
#3406 = ORIENTED_EDGE ( 'NONE', *, *, #8580, .F. ) ;
#3407 = ORIENTED_EDGE ( 'NONE', *, *, #44777, .T. ) ;
#3408 = DIRECTION ( 'NONE',  ( 0.9999697198139515519, 0.000000000000000000, 0.007781995580013368816 ) ) ;
#3409 = DIRECTION ( 'NONE',  ( 0.5449076811759707706, 0.6444004775717708799, -0.5364919789714476250 ) ) ;
#3410 = ORIENTED_EDGE ( 'NONE', *, *, #39397, .T. ) ;
#3411 = CARTESIAN_POINT ( 'NONE',  ( -13.59629007026659941, -0.1191753592594190225, 7.030593099338098284 ) ) ;
#3412 = ORIENTED_EDGE ( 'NONE', *, *, #28944, .F. ) ;
#3413 = CARTESIAN_POINT ( 'NONE',  ( -21.55226037509761738, -4.565544526780660917, 12.54639795354807141 ) ) ;
#3414 = CARTESIAN_POINT ( 'NONE',  ( -19.69569380384165669, -0.1191753592594177458, 14.58090286586150697 ) ) ;
#3416 = EDGE_LOOP ( 'NONE', ( #23314, #10175, #32909, #13734 ) ) ;
#3415 = EDGE_CURVE ( 'NONE', #17026, #4038, #28277, .T. ) ;
#3417 = DIRECTION ( 'NONE',  ( -0.005002170337468016433, -0.7660444431189770143, 0.6427681459581293666 ) ) ;
#3418 = EDGE_CURVE ( 'NONE', #29528, #18631, #15243, .T. ) ;
#3419 = ADVANCED_FACE ( 'NONE', ( #45892 ), #7007, .F. ) ;
#3420 = DIRECTION ( 'NONE',  ( 0.5449076811759707706, 0.6444004775717708799, -0.5364919789714476250 ) ) ;
#3421 = ORIENTED_EDGE ( 'NONE', *, *, #10902, .T. ) ;
#3422 = DIRECTION ( 'NONE',  ( 0.005961354470445682716, -0.6427876096865404731, -0.7660212471507180654 ) ) ;
#3423 = PLANE ( 'NONE',  #39244 ) ;
#3424 = CARTESIAN_POINT ( 'NONE',  ( -15.16984770538739014, 4.495856970884011261, 10.15227235917422455 ) ) ;
#3425 = DIRECTION ( 'NONE',  ( 0.005002170337468016433, -0.7660444431189770143, -0.6427681459581293666 ) ) ;
#3426 = ORIENTED_EDGE ( 'NONE', *, *, #37039, .F. ) ;
#3427 = CARTESIAN_POINT ( 'NONE',  ( -13.11936205432852987, -1.813211359398158029, 1.919475938924976255 ) ) ;
#3428 = CARTESIAN_POINT ( 'NONE',  ( -13.02800394838083342, 0.000000000000000000, 6.565680535424952780 ) ) ;
#3429 = CARTESIAN_POINT ( 'NONE',  ( -13.39181721811076997, -2.137015261443160341, 2.014975737379525178 ) ) ;
#3430 = LINE ( 'NONE', #8834, #40458 ) ;
#3431 = DIRECTION ( 'NONE',  ( 0.005961354470445682716, -0.6427876096865404731, -0.7660212471507180654 ) ) ;
#3432 = CARTESIAN_POINT ( 'NONE',  ( -19.59569683186026268, 0.000000000000000000, 14.58168106541950948 ) ) ;
#3433 = EDGE_CURVE ( 'NONE', #83, #29572, #24309, .T. ) ;
#3434 = CARTESIAN_POINT ( 'NONE',  ( -22.02230563637845151, 19.67040402849924163, -4.420763475398227449 ) ) ;
#3435 = ORIENTED_EDGE ( 'NONE', *, *, #26539, .T. ) ;
#3436 = FACE_OUTER_BOUND ( 'NONE', #35039, .T. ) ;
#3437 = CARTESIAN_POINT ( 'NONE',  ( -16.33317936670417225, 0.000000000000000000, 13.31440848639340224 ) ) ;
#3438 = ORIENTED_EDGE ( 'NONE', *, *, #9188, .T. ) ;
#3439 = DIRECTION ( 'NONE',  ( 0.005961354470445682716, -0.6427876096865404731, -0.7660212471507180654 ) ) ;
#3440 = CARTESIAN_POINT ( 'NONE',  ( -15.93097076849315386, -0.1191753592594191752, 8.489752353529109286 ) ) ;
#3441 = VECTOR ( 'NONE', #40082, 999.9999999999998863 ) ;
#3442 = DIRECTION ( 'NONE',  ( -0.5364919789714478471, 0.6444004775717705469, -0.5449076811759709926 ) ) ;
#3443 = CARTESIAN_POINT ( 'NONE',  ( -70.00279782826048347, 0.1332992376639058896, -7.501782499249456393 ) ) ;
#3444 = CARTESIAN_POINT ( 'NONE',  ( -24.27063949748155380, 0.000000000000000000, 6.308861732390097288 ) ) ;
#3445 = ORIENTED_EDGE ( 'NONE', *, *, #11205, .T. ) ;
#3446 = ORIENTED_EDGE ( 'NONE', *, *, #29401, .F. ) ;
#3447 = LINE ( 'NONE', #2322, #16849 ) ;
#3448 = FACE_OUTER_BOUND ( 'NONE', #11114, .T. ) ;
#3449 = B_SPLINE_CURVE_WITH_KNOTS ( 'NONE', 3,
 ( #47504, #55745, #16551, #4070 ),
 .UNSPECIFIED., .F., .F.,
 ( 4, 4 ),
 ( 0.0001648889278767292786, 0.0003345323828099543780 ),
 .UNSPECIFIED. ) ;
#3450 = CARTESIAN_POINT ( 'NONE',  ( -21.93567689722629765, 19.99370688441071309, -4.657437592157546824 ) ) ;
#3451 = ORIENTED_EDGE ( 'NONE', *, *, #8832, .F. ) ;
#3452 = CARTESIAN_POINT ( 'NONE',  ( -26.26580391614848864, 17.49370688441070953, -4.622528711259356271 ) ) ;
#3453 = EDGE_CURVE ( 'NONE', #55170, #5309, #45325, .T. ) ;
#3454 = ORIENTED_EDGE ( 'NONE', *, *, #18798, .F. ) ;
#3455 = CARTESIAN_POINT ( 'NONE',  ( 2.072287782118878319, 0.000000000000000000, -2.950529333540147015 ) ) ;
#3456 = VERTEX_POINT ( 'NONE', #41062 ) ;
#3457 = EDGE_LOOP ( 'NONE', ( #36767, #49794, #55702, #37261 ) ) ;
#3458 = ORIENTED_EDGE ( 'NONE', *, *, #42269, .T. ) ;
#3459 = LINE ( 'NONE', #2606, #40218 ) ;
#3460 = CARTESIAN_POINT ( 'NONE',  ( -26.13337879274045505, 0.000000000000000000, 6.833023547870798353 ) ) ;
#3461 = CARTESIAN_POINT ( 'NONE',  ( -10.37219204796779337, -9.994947293139700761, 0.8105380568915174777 ) ) ;
#3462 = EDGE_CURVE ( 'NONE', #41178, #1421, #2148, .T. ) ;
#3463 = LINE ( 'NONE', #20779, #50227 ) ;
#3464 = EDGE_LOOP ( 'NONE', ( #10205, #16971, #45019 ) ) ;
#3465 = EDGE_CURVE ( 'NONE', #40362, #49112, #54143, .T. ) ;
#3466 = ADVANCED_FACE ( 'NONE', ( #50434 ), #16617, .F. ) ;
#3467 = ORIENTED_EDGE ( 'NONE', *, *, #56052, .F. ) ;
#3468 = VERTEX_POINT ( 'NONE', #20619 ) ;
#3469 = FACE_OUTER_BOUND ( 'NONE', #45038, .T. ) ;
#3470 = CARTESIAN_POINT ( 'NONE',  ( -16.86599266918588924, -0.1191753592594177180, 9.221139936508615520 ) ) ;
#3471 = ORIENTED_EDGE ( 'NONE', *, *, #15401, .F. ) ;
#3472 = LINE ( 'NONE', #38102, #42939 ) ;
#3473 = ADVANCED_FACE ( 'NONE', ( #50960, #8114 ), #12651, .T. ) ;
#3474 = ORIENTED_EDGE ( 'NONE', *, *, #47318, .T. ) ;
#3475 = DIRECTION ( 'NONE',  ( 0.000000000000000000, -1.000000000000000000, 0.000000000000000000 ) ) ;
#3476 = DIRECTION ( 'NONE',  ( 0.005961354470445682716, -0.6427876096865404731, -0.7660212471507180654 ) ) ;
#3477 = VECTOR ( 'NONE', #12224, 999.9999999999998863 ) ;
#3478 = VERTEX_POINT ( 'NONE', #43025 ) ;
#3479 = EDGE_CURVE ( 'NONE', #27552, #55206, #25166, .T. ) ;
#3480 = CARTESIAN_POINT ( 'NONE',  ( -21.47263955680318404, 0.000000000000000000, 5.022634149262071190 ) ) ;
#3481 = VERTEX_POINT ( 'NONE', #24566 ) ;
#3482 = EDGE_CURVE ( 'NONE', #29459, #34227, #11538, .T. ) ;
#3483 = LINE ( 'NONE', #20795, #5612 ) ;
#3484 = DIRECTION ( 'NONE',  ( -0.9999697198139514409, -0.000000000000000000, -0.007781995580013368816 ) ) ;
#3485 = ORIENTED_EDGE ( 'NONE', *, *, #50766, .F. ) ;
#3486 = DIRECTION ( 'NONE',  ( -0.005002170337468016433, -0.7660444431189770143, 0.6427681459581293666 ) ) ;
#3487 = CARTESIAN_POINT ( 'NONE',  ( -14.97295643975815871, -0.1191753592594183703, 4.803887144487482885 ) ) ;
#3488 = DIRECTION ( 'NONE',  ( -0.5364919789714478471, 0.6444004775717705469, -0.5449076811759709926 ) ) ;
#3489 = ADVANCED_FACE ( 'NONE', ( #24861 ), #16326, .F. ) ;
#3490 = DIRECTION ( 'NONE',  ( 0.000000000000000000, -0.000000000000000000, -1.000000000000000000 ) ) ;
#3491 = EDGE_LOOP ( 'NONE', ( #24539, #39559, #35140, #18071 ) ) ;
#3492 = EDGE_CURVE ( 'NONE', #29905, #3617, #47010, .T. ) ;
#3493 = EDGE_LOOP ( 'NONE', ( #13375, #23166, #30243, #39850 ) ) ;
#3494 = DIRECTION ( 'NONE',  ( 0.000000000000000000, -0.000000000000000000, -1.000000000000000000 ) ) ;
#3495 = CARTESIAN_POINT ( 'NONE',  ( -9.943925025897915049, 0.000000000000000000, 2.527028782849607857 ) ) ;
#3496 = LINE ( 'NONE', #30172, #4132 ) ;
#3497 = LINE ( 'NONE', #11729, #50288 ) ;
#3498 = CARTESIAN_POINT ( 'NONE',  ( -13.07066190154808361, 0.000000000000000000, 12.04713590736729678 ) ) ;
#3499 = EDGE_CURVE ( 'NONE', #25139, #32467, #20869, .T. ) ;
#3500 = CARTESIAN_POINT ( 'NONE',  ( -14.00280974873554030, 0.000000000000000000, 12.40921378708904044 ) ) ;
#3501 = ORIENTED_EDGE ( 'NONE', *, *, #44751, .T. ) ;
#3502 =( BOUNDED_CURVE ( )  B_SPLINE_CURVE ( 3, ( #14514, #2281, #50256, #36950 ),
 .UNSPECIFIED., .F., .F. ) 
 B_SPLINE_CURVE_WITH_KNOTS ( ( 4, 4 ),
 ( 0.3868401276509516040, 2.001189637452388759 ),
 .UNSPECIFIED. ) 
 CURVE ( )  GEOMETRIC_REPRESENTATION_ITEM ( )  RATIONAL_B_SPLINE_CURVE ( ( 1.000000000000000000, 0.7943613114863611324, 0.7943613114863611324, 1.000000000000000000 ) ) 
 REPRESENTATION_ITEM ( '' )  );
#3503 = CARTESIAN_POINT ( 'NONE',  ( -60.88973930853472183, 7.404220597074750110, 2.999999999999993339 ) ) ;
#3504 = CARTESIAN_POINT ( 'NONE',  ( -19.15040009907104235, -0.1191753592594162470, 4.220292173140257397 ) ) ;
#3505 = VERTEX_POINT ( 'NONE', #56097 ) ;
#3506 = CARTESIAN_POINT ( 'NONE',  ( -16.06709938707323460, 0.000000000000000000, 13.13181314741652628 ) ) ;
#3507 = ORIENTED_EDGE ( 'NONE', *, *, #25874, .F. ) ;
#3508 = DIRECTION ( 'NONE',  ( 0.000000000000000000, 0.000000000000000000, -1.000000000000000000 ) ) ;
#3509 = DIRECTION ( 'NONE',  ( 0.9999697198139515519, 0.000000000000000000, 0.007781995580013368816 ) ) ;
#3510 = CARTESIAN_POINT ( 'NONE',  ( -30.79411802867772607, 0.000000000000000000, 8.643412946479525516 ) ) ;
#3511 = DIRECTION ( 'NONE',  ( -0.005002170337468016433, -0.7660444431189770143, 0.6427681459581293666 ) ) ;
#3512 = CARTESIAN_POINT ( 'NONE',  ( -68.03033152755355673, 2.000000000000001332, -8.215550190268007924 ) ) ;
#3513 = VERTEX_POINT ( 'NONE', #55810 ) ;
#3514 = ORIENTED_EDGE ( 'NONE', *, *, #26059, .F. ) ;
#3515 = CARTESIAN_POINT ( 'NONE',  ( -68.33274616240578325, -0.6011730142051754378, 5.504334939579325514 ) ) ;
#3516 = CARTESIAN_POINT ( 'NONE',  ( -13.27065584551087163, 0.000000000000000000, 12.04557950825129176 ) ) ;
#3517 = DIRECTION ( 'NONE',  ( 0.005961354470445682716, -0.6427876096865404731, -0.7660212471507180654 ) ) ;
#3518 = CARTESIAN_POINT ( 'NONE',  ( 2.072287782118878319, 0.000000000000000000, -2.950529333540147015 ) ) ;
#3519 = VECTOR ( 'NONE', #51754, 1000.000000000000114 ) ;
#3520 = PLANE ( 'NONE',  #16519 ) ;
#3521 = DIRECTION ( 'NONE',  ( 0.000000000000000000, -0.000000000000000000, -1.000000000000000000 ) ) ;
#3522 = ADVANCED_FACE ( 'NONE', ( #42728 ), #33650, .F. ) ;
#3523 = ORIENTED_EDGE ( 'NONE', *, *, #7285, .T. ) ;
#3524 = CARTESIAN_POINT ( 'NONE',  ( -16.49770049126292193, 0.000000000000000000, 8.754670973479470319 ) ) ;
#3525 = DIRECTION ( 'NONE',  ( 0.5449076811759707706, 0.6444004775717708799, -0.5364919789714476250 ) ) ;
#3526 = LINE ( 'NONE', #54622, #44137 ) ;
#3527 = ORIENTED_EDGE ( 'NONE', *, *, #8696, .F. ) ;
#3528 = CARTESIAN_POINT ( 'NONE',  ( -11.91804826722769128, 25.86399001096056338, -3.000000000000000000 ) ) ;
#3529 = CYLINDRICAL_SURFACE ( 'NONE', #534, 0.5000000000000004441 ) ;
#3530 = DIRECTION ( 'NONE',  ( 0.7660212471507180654, -0.6427876096865404731, 0.005961354470445141482 ) ) ;
#3531 = VERTEX_POINT ( 'NONE', #38480 ) ;
#3532 = CARTESIAN_POINT ( 'NONE',  ( -19.53866861116660303, 0.000000000000000000, 7.253677177188349035 ) ) ;
#3533 = ORIENTED_EDGE ( 'NONE', *, *, #246, .T. ) ;
#3534 = ADVANCED_FACE ( 'NONE', ( #33395 ), #29712, .F. ) ;
#3535 = VERTEX_POINT ( 'NONE', #55238 ) ;
#3536 = ORIENTED_EDGE ( 'NONE', *, *, #11158, .F. ) ;
#3537 = ORIENTED_EDGE ( 'NONE', *, *, #25672, .T. ) ;
#3538 = LINE ( 'NONE', #42159, #49263 ) ;
#3539 = ORIENTED_EDGE ( 'NONE', *, *, #51811, .F. ) ;
#3540 = CARTESIAN_POINT ( 'NONE',  ( -13.18266667305592499, 23.31520888598613084, -3.678144203997483430 ) ) ;
#3541 = EDGE_LOOP ( 'NONE', ( #15578, #43860, #22731, #39612 ) ) ;
#3542 = PLANE ( 'NONE',  #47657 ) ;
#3543 = ADVANCED_FACE ( 'NONE', ( #47269 ), #37931, .F. ) ;
#3544 = ORIENTED_EDGE ( 'NONE', *, *, #20901, .F. ) ;
#3545 = ORIENTED_EDGE ( 'NONE', *, *, #18337, .T. ) ;
#3546 = EDGE_CURVE ( 'NONE', #32426, #10918, #7846, .T. ) ;
#3547 = CARTESIAN_POINT ( 'NONE',  ( -10.42736264288669723, 0.000000000000000000, 4.939265034590974324 ) ) ;
#3548 = CARTESIAN_POINT ( 'NONE',  ( -20.97744843082703881, -1.165603555308156736, 6.743239110737863307 ) ) ;
#3549 = LINE ( 'NONE', #37921, #33249 ) ;
#3550 = FACE_OUTER_BOUND ( 'NONE', #51387, .T. ) ;
#3551 =( LENGTH_UNIT ( ) NAMED_UNIT ( * ) SI_UNIT ( .MILLI., .METRE. ) );
#3552 = EDGE_LOOP ( 'NONE', ( #12740, #41321, #55076, #31005 ) ) ;
#3553 = EDGE_CURVE ( 'NONE', #18849, #17489, #33945, .T. ) ;
#3554 = VECTOR ( 'NONE', #6570, 1000.000000000000000 ) ;
#3555 = ORIENTED_EDGE ( 'NONE', *, *, #245, .F. ) ;
#3556 = DIRECTION ( 'NONE',  ( 0.9999697198139515519, 0.000000000000000000, 0.007781995580013368816 ) ) ;
#3557 = DIRECTION ( 'NONE',  ( 0.005961354470445682716, -0.6427876096865404731, -0.7660212471507180654 ) ) ;
#3558 = UNCERTAINTY_MEASURE_WITH_UNIT (LENGTH_MEASURE( 1.000000000000000082E-05 ), #11031, 'distance_accuracy_value', 'NONE');
#3559 = ADVANCED_BREP_SHAPE_REPRESENTATION ( '', ( #2589, #2610 ), #47980 ) ;
#3560 = DIRECTION ( 'NONE',  ( 0.7660212471507180654, -0.6427876096865404731, 0.005961354470445141482 ) ) ;
#3561 = EDGE_CURVE ( 'NONE', #29456, #7607, #8376, .T. ) ;
#3562 = DIRECTION ( 'NONE',  ( 0.005002170337468016433, -0.7660444431189770143, -0.6427681459581293666 ) ) ;
#3563 = LINE ( 'NONE', #3293, #12241 ) ;
#3564 = CARTESIAN_POINT ( 'NONE',  ( -23.33849165029409889, 0.000000000000000000, 5.946783852668351855 ) ) ;
#3565 = VERTEX_POINT ( 'NONE', #54978 ) ;
#3566 = CARTESIAN_POINT ( 'NONE',  ( -14.54935328597183819, -0.1191753592594172878, 8.869836490052643185 ) ) ;
#3567 = CARTESIAN_POINT ( 'NONE',  ( -16.06146926423485866, -3.594132820645661308, 8.819336114335181165 ) ) ;
#3568 = ORIENTED_EDGE ( 'NONE', *, *, #40271, .T. ) ;
#3569 = LINE ( 'NONE', #7855, #27979 ) ;
#3570 = CARTESIAN_POINT ( 'NONE',  ( -14.61196876796175204, 0.000000000000000000, 5.276031531936651753 ) ) ;
#3571 = FACE_OUTER_BOUND ( 'NONE', #44321, .T. ) ;
#3572 = CARTESIAN_POINT ( 'NONE',  ( -18.76354595665420177, -0.1191753592594177458, 14.21882498613976331 ) ) ;
#3573 = PLANE ( 'NONE',  #9628 ) ;
#3574 = EDGE_LOOP ( 'NONE', ( #36640, #40801, #23513 ) ) ;
#3575 = EDGE_LOOP ( 'NONE', ( #25272, #45240, #10854, #12770 ) ) ;
#3576 = LINE ( 'NONE', #26027, #8516 ) ;
#3577 = DIRECTION ( 'NONE',  ( 0.000000000000000000, -0.000000000000000000, -1.000000000000000000 ) ) ;
#3578 = CARTESIAN_POINT ( 'NONE',  ( -58.00000000000000711, -9.999999999999998224, 7.102951435054649637E-15 ) ) ;
#3579 = EDGE_CURVE ( 'NONE', #11430, #10812, #50701, .T. ) ;
#3580 = CARTESIAN_POINT ( 'NONE',  ( -13.93957187223785077, 1.419719901456504285, 4.625926450176987892 ) ) ;
#3581 = DIRECTION ( 'NONE',  ( 0.007781995580012663651, 0.000000000000000000, -0.9999697198139515519 ) ) ;
#3582 = EDGE_CURVE ( 'NONE', #54123, #13455, #39041, .T. ) ;
#3583 = CARTESIAN_POINT ( 'NONE',  ( -19.60990026154428278, 0.000000000000000000, 4.498472333781370125 ) ) ;
#3584 = DIRECTION ( 'NONE',  ( -0.6427681459581293666, -0.7660444431189770143, -0.005002170337467561935 ) ) ;
#3585 = CARTESIAN_POINT ( 'NONE',  ( -10.28842178966973897, 0.000000000000000000, 0.8776935365639153552 ) ) ;
#3586 = CARTESIAN_POINT ( 'NONE',  ( -68.40341787366602944, -9.538706321749058858, -7.664179260766974089 ) ) ;
#3587 = EDGE_CURVE ( 'NONE', #21782, #10029, #14046, .T. ) ;
#3588 = ADVANCED_FACE ( 'NONE', ( #30809 ), #52100, .F. ) ;
#3589 = LINE ( 'NONE', #33682, #180 ) ;
#3590 = ORIENTED_EDGE ( 'NONE', *, *, #23040, .F. ) ;
#3591 = DIRECTION ( 'NONE',  ( 0.9321478471874540261, 0.000000000000000000, -0.3620778797217457101 ) ) ;
#3592 = EDGE_CURVE ( 'NONE', #44810, #31885, #47564, .T. ) ;
#3593 = EDGE_CURVE ( 'NONE', #47105, #49493, #707, .T. ) ;
#3594 = ADVANCED_FACE ( 'NONE', ( #35350 ), #4968, .F. ) ;
#3595 = ORIENTED_EDGE ( 'NONE', *, *, #3264, .F. ) ;
#3596 = ORIENTED_EDGE ( 'NONE', *, *, #45911, .T. ) ;
#3597 = ORIENTED_EDGE ( 'NONE', *, *, #44568, .T. ) ;
#3598 = ORIENTED_EDGE ( 'NONE', *, *, #11027, .T. ) ;
#3599 = ORIENTED_EDGE ( 'NONE', *, *, #8048, .F. ) ;
#3600 = ORIENTED_EDGE ( 'NONE', *, *, #52374, .F. ) ;
#3601 = CARTESIAN_POINT ( 'NONE',  ( -27.06552663992790997, 0.000000000000000000, 7.195101427592543786 ) ) ;
#3602 = PLANE ( 'NONE',  #41073 ) ;
#3603 = CARTESIAN_POINT ( 'NONE',  ( -69.59775774058348929, -0.6007421665236040154, 7.493101075386322307 ) ) ;
#3604 = ORIENTED_EDGE ( 'NONE', *, *, #45738, .T. ) ;
#3605 = DIRECTION ( 'NONE',  ( 0.6427681459581294776, -0.7660444431189769032, 0.005002170337467562802 ) ) ;
#3606 = EDGE_CURVE ( 'NONE', #21318, #55411, #52647, .T. ) ;
#3607 = ORIENTED_EDGE ( 'NONE', *, *, #29372, .F. ) ;
#3608 = DIRECTION ( 'NONE',  ( 0.9999697198139515519, 0.000000000000000000, 0.007781995580013368816 ) ) ;
#3609 = ORIENTED_EDGE ( 'NONE', *, *, #22281, .T. ) ;
#3610 = EDGE_CURVE ( 'NONE', #21327, #34381, #34498, .T. ) ;
#3611 = DIRECTION ( 'NONE',  ( 0.7660212471507180654, -0.6427876096865404731, 0.005961354470445141482 ) ) ;
#3612 = ADVANCED_FACE ( 'NONE', ( #13753 ), #17449, .F. ) ;
#3613 = CARTESIAN_POINT ( 'NONE',  ( -13.68113857516357967, 0.000000000000000000, 5.083269411509881763 ) ) ;
#3614 = FACE_OUTER_BOUND ( 'NONE', #12624, .T. ) ;
#3615 = VERTEX_POINT ( 'NONE', #22571 ) ;
#3616 = CARTESIAN_POINT ( 'NONE',  ( -3.335658863730355694, -6.482724466489810489, -1.922690393539094433 ) ) ;
#3617 = VERTEX_POINT ( 'NONE', #34786 ) ;
#3618 = EDGE_CURVE ( 'NONE', #8639, #20837, #4678, .T. ) ;
#3619 = DIRECTION ( 'NONE',  ( 0.007781995580012663651, -3.146120232559066537E-19, -0.9999697198139514409 ) ) ;
#3620 = CARTESIAN_POINT ( 'NONE',  ( -16.15650678959040221, 3.524445264749011208, 2.845219389405668320 ) ) ;
#3621 = VECTOR ( 'NONE', #5850, 1000.000000000000000 ) ;
#3622 = DIRECTION ( 'NONE',  ( -0.000000000000000000, -0.000000000000000000, -1.000000000000000000 ) ) ;
#3623 = CARTESIAN_POINT ( 'NONE',  ( -16.49638283687364293, 0.000000000000000000, 8.585355214184495765 ) ) ;
#3624 = CARTESIAN_POINT ( 'NONE',  ( -19.32961685222932147, 0.000000000000000000, 14.39908572644263351 ) ) ;
#3625 = DIRECTION ( 'NONE',  ( -0.05705673239519650636, 0.9983709377222390602, 2.351258244848514932E-16 ) ) ;
#3626 = FACE_OUTER_BOUND ( 'NONE', #3696, .T. ) ;
#3627 = CARTESIAN_POINT ( 'NONE',  ( -70.19153117219258320, -11.75686401390256464, -8.809708619959531362 ) ) ;
#3628 = VERTEX_POINT ( 'NONE', #31071 ) ;
#3629 = CARTESIAN_POINT ( 'NONE',  ( -56.65747392845349850, 6.423369595003239674, -2.400381607668001571 ) ) ;
#3630 = EDGE_LOOP ( 'NONE', ( #44556, #45588, #23509, #56008 ) ) ;
#3631 = CARTESIAN_POINT ( 'NONE',  ( -11.15478472993248715, -0.03228989815065527735, 1.213188107564080020 ) ) ;
#3632 = LINE ( 'NONE', #16698, #16948 ) ;
#3633 = LINE ( 'NONE', #7326, #10551 ) ;
#3634 = CARTESIAN_POINT ( 'NONE',  ( -21.26187472307101345, 2.391131607591508335, 4.864476313006088404 ) ) ;
#3635 = CARTESIAN_POINT ( 'NONE',  ( -11.52190826124595091, 0.7721120973665037690, 2.623989063664057042 ) ) ;
#3636 = LINE ( 'NONE', #42547, #9270 ) ;
#3637 = PRODUCT_CONTEXT ( 'NONE', #12626, 'mechanical' ) ;
#3638 = ORIENTED_EDGE ( 'NONE', *, *, #20025, .T. ) ;
#3639 = DIRECTION ( 'NONE',  ( 0.000000000000000000, -0.000000000000000000, -1.000000000000000000 ) ) ;
#3640 = PLANE ( 'NONE',  #53043 ) ;
#3641 = DIRECTION ( 'NONE',  ( 0.5364919789714477361, 0.6444004775717706579, 0.5449076811759711036 ) ) ;
#3642 = CARTESIAN_POINT ( 'NONE',  ( -13.17065887352947762, -0.1191753592594197858, 12.04635770780929427 ) ) ;
#3643 = CARTESIAN_POINT ( 'NONE',  ( -14.89316374707889423, 4.172053068839010059, 9.513381545639502335 ) ) ;
#3644 = DIRECTION ( 'NONE',  ( 0.007781995580012662783, 0.000000000000000000, -0.9999697198139514409 ) ) ;
#3645 = CARTESIAN_POINT ( 'NONE',  ( -17.42122617793452477, 0.000000000000000000, 8.008819743427922688 ) ) ;
#3646 = ORIENTED_EDGE ( 'NONE', *, *, #15003, .F. ) ;
#3647 = CARTESIAN_POINT ( 'NONE',  ( -16.93647090655645826, 0.000000000000000000, 5.427267732391580779 ) ) ;
#3648 = CARTESIAN_POINT ( 'NONE',  ( -14.34960227313585790, 3.038739411681509850, 2.158852872141225898 ) ) ;
#3649 = VERTEX_POINT ( 'NONE', #413 ) ;
#3650 = VERTEX_POINT ( 'NONE', #51810 ) ;
#3651 = CARTESIAN_POINT ( 'NONE',  ( -12.20525343324862355, -0.1191753592594177180, 7.410750537899888357 ) ) ;
#3652 = EDGE_CURVE ( 'NONE', #22884, #21327, #9507, .T. ) ;
#3653 = EDGE_CURVE ( 'NONE', #40408, #13812, #12920, .T. ) ;
#3654 = VERTEX_POINT ( 'NONE', #8684 ) ;
#3655 = FACE_OUTER_BOUND ( 'NONE', #46060, .T. ) ;
#3656 = EDGE_CURVE ( 'NONE', #39352, #20003, #13215, .T. ) ;
#3657 = VECTOR ( 'NONE', #6871, 1000.000000000000227 ) ;
#3658 = VERTEX_POINT ( 'NONE', #26832 ) ;
#3659 = EDGE_LOOP ( 'NONE', ( #42625, #8808, #26182, #49251 ) ) ;
#3660 = VERTEX_POINT ( 'NONE', #44159 ) ;
#3661 = FACE_OUTER_BOUND ( 'NONE', #42039, .T. ) ;
#3662 = CARTESIAN_POINT ( 'NONE',  ( -65.13109422105631552, -9.163455212069004929, 1.319813854473150805 ) ) ;
#3663 = CARTESIAN_POINT ( 'NONE',  ( -20.34698012014669999, -3.756034771668160577, 4.664942007982749494 ) ) ;
#3664 = ORIENTED_EDGE ( 'NONE', *, *, #36806, .T. ) ;
#3665 = VERTEX_POINT ( 'NONE', #35623 ) ;
#3666 = EDGE_CURVE ( 'NONE', #49206, #6270, #35094, .T. ) ;
#3667 = FACE_OUTER_BOUND ( 'NONE', #8087, .T. ) ;
#3668 = CARTESIAN_POINT ( 'NONE',  ( -13.27065584551087163, 0.000000000000000000, 12.04557950825129176 ) ) ;
#3669 = ORIENTED_EDGE ( 'NONE', *, *, #23512, .F. ) ;
#3670 = EDGE_CURVE ( 'NONE', #15326, #187, #52940, .T. ) ;
#3671 = FACE_OUTER_BOUND ( 'NONE', #40330, .T. ) ;
#3672 = CARTESIAN_POINT ( 'NONE',  ( -24.26986129792355129, -0.1191753592594197858, 6.208864760408702388 ) ) ;
#3673 = VERTEX_POINT ( 'NONE', #31380 ) ;
#3674 = FACE_OUTER_BOUND ( 'NONE', #5919, .T. ) ;
#3675 = CARTESIAN_POINT ( 'NONE',  ( -25.85160320928759248, 17.67349956316208193, 4.606045228336897779 ) ) ;
#3676 = ORIENTED_EDGE ( 'NONE', *, *, #53272, .T. ) ;
#3677 = EDGE_CURVE ( 'NONE', #52348, #36108, #48701, .T. ) ;
#3678 = CARTESIAN_POINT ( 'NONE',  ( -22.40478740399063895, 0.000000000000000000, 5.384712028983816623 ) ) ;
#3679 = EDGE_CURVE ( 'NONE', #27005, #10812, #36748, .T. ) ;
#3680 = LINE ( 'NONE', #7972, #35439 ) ;
#3681 = VERTEX_POINT ( 'NONE', #18880 ) ;
#3682 = DIRECTION ( 'NONE',  ( -0.9999697198139514409, -0.000000000000000000, -0.007781995580013368816 ) ) ;
#3683 = CARTESIAN_POINT ( 'NONE',  ( -11.81552522639938907, 0.000000000000000000, 4.189797892771416343 ) ) ;
#3684 = DIRECTION ( 'NONE',  ( 0.007781995580012663651, 0.000000000000000000, -0.9999697198139515519 ) ) ;
#3685 = FACE_OUTER_BOUND ( 'NONE', #34439, .T. ) ;
#3686 = EDGE_LOOP ( 'NONE', ( #27087, #1582, #10444, #55744, #6293 ) ) ;
#3687 = VECTOR ( 'NONE', #38903, 999.9999999999998863 ) ;
#3688 = CARTESIAN_POINT ( 'NONE',  ( -17.29990502820820453, -0.6798977022406551551, 4.517630311409670973 ) ) ;
#3689 = FACE_OUTER_BOUND ( 'NONE', #39722, .T. ) ;
#3690 = FACE_OUTER_BOUND ( 'NONE', #36286, .T. ) ;
#3691 = DIRECTION ( 'NONE',  ( -0.5364919789714478471, 0.6444004775717705469, -0.5449076811759709926 ) ) ;
#3692 = FACE_OUTER_BOUND ( 'NONE', #23485, .T. ) ;
#3693 = CARTESIAN_POINT ( 'NONE',  ( -13.47484560386877028, 2.553033558614008047, 1.834564234598528465 ) ) ;
#3694 = VECTOR ( 'NONE', #30113, 1000.000000000000227 ) ;
#3695 = DIRECTION ( 'NONE',  ( 0.007781995580012662783, 0.000000000000000000, -0.9999697198139514409 ) ) ;
#3696 = EDGE_LOOP ( 'NONE', ( #50013, #22668, #7321, #9847 ) ) ;
#3697 = DIRECTION ( 'NONE',  ( 1.000000000000000000, 0.000000000000000000, 0.000000000000000000 ) ) ;
#3698 = CARTESIAN_POINT ( 'NONE',  ( -69.44698877097060574, -0.5991245381873403497, 7.306242118358709625 ) ) ;
#3699 = VERTEX_POINT ( 'NONE', #6935 ) ;
#3700 = CARTESIAN_POINT ( 'NONE',  ( -18.68332481975068760, -2.298917212465658277, 7.712084379083277597 ) ) ;
#3701 = CARTESIAN_POINT ( 'NONE',  ( -18.12332189171708663, 0.000000000000000000, 4.510041230393051492 ) ) ;
#3702 = DIRECTION ( 'NONE',  ( -0.005002170337468016433, -0.7660444431189770143, 0.6427681459581293666 ) ) ;
#3703 = LINE ( 'NONE', #34647, #41439 ) ;
#3704 = CARTESIAN_POINT ( 'NONE',  ( -12.62864409447993808, 2.067327705546504912, 5.179552317802938788 ) ) ;
#3705 = ORIENTED_EDGE ( 'NONE', *, *, #45656, .T. ) ;
#3706 = VERTEX_POINT ( 'NONE', #45261 ) ;
#3707 = FACE_OUTER_BOUND ( 'NONE', #4565, .T. ) ;
#3708 = CARTESIAN_POINT ( 'NONE',  ( -26.13493519185646008, 0.000000000000000000, 7.033017491833586377 ) ) ;
#3709 = ORIENTED_EDGE ( 'NONE', *, *, #38832, .F. ) ;
#3710 = CARTESIAN_POINT ( 'NONE',  ( -8.831699957570222637, -8.502732429729430663, 0.2121586136495015040 ) ) ;
#3711 = EDGE_CURVE ( 'NONE', #40367, #11131, #54069, .T. ) ;
#3712 = VECTOR ( 'NONE', #23295, 999.9999999999998863 ) ;
#3713 = VECTOR ( 'NONE', #30723, 999.9999999999998863 ) ;
#3714 = ORIENTED_EDGE ( 'NONE', *, *, #35463, .T. ) ;
#3715 = LINE ( 'NONE', #55396, #3194 ) ;
#3716 = ORIENTED_EDGE ( 'NONE', *, *, #25034, .F. ) ;
#3717 = LINE ( 'NONE', #24460, #6642 ) ;
#3718 = EDGE_CURVE ( 'NONE', #18779, #46324, #15132, .T. ) ;
#3719 = ADVANCED_FACE ( 'NONE', ( #23132 ), #6367, .T. ) ;
#3720 = ORIENTED_EDGE ( 'NONE', *, *, #36641, .T. ) ;
#3721 = ORIENTED_EDGE ( 'NONE', *, *, #24479, .F. ) ;
#3722 = ORIENTED_EDGE ( 'NONE', *, *, #16123, .F. ) ;
#3723 = CARTESIAN_POINT ( 'NONE',  ( -10.24493344548221430, 0.000000000000000000, 7.197853645293383451 ) ) ;
#3724 = CARTESIAN_POINT ( 'NONE',  ( -19.19976828709737049, -2.946525016555661125, 4.245153571985499141 ) ) ;
#3725 = DIRECTION ( 'NONE',  ( 0.6246952433987894571, -0.7422098413412800966, -0.2426528472758541777 ) ) ;
#3727 = PLANE ( 'NONE',  #24862 ) ;
#3726 = AXIS2_PLACEMENT_3D ( 'NONE', #10183, #26665, #18992 ) ;
#3728 = VERTEX_POINT ( 'NONE', #24247 ) ;
#3729 = VECTOR ( 'NONE', #31537, 1000.000000000000227 ) ;
#3730 = ORIENTED_EDGE ( 'NONE', *, *, #17146, .T. ) ;
#3731 = ORIENTED_EDGE ( 'NONE', *, *, #14251, .T. ) ;
#3732 = CARTESIAN_POINT ( 'NONE',  ( 2.072287782118878319, 0.000000000000000000, -2.950529333540147015 ) ) ;
#3733 = DIRECTION ( 'NONE',  ( 0.7660212471507180654, -0.6427876096865404731, 0.005961354470445141482 ) ) ;
#3734 = ORIENTED_EDGE ( 'NONE', *, *, #14449, .F. ) ;
#3735 = CARTESIAN_POINT ( 'NONE',  ( -13.96458224818957561, 0.000000000000000000, 7.497062062367251478 ) ) ;
#3736 = ORIENTED_EDGE ( 'NONE', *, *, #39966, .T. ) ;
#3737 = LINE ( 'NONE', #7438, #12438 ) ;
#3738 = DIRECTION ( 'NONE',  ( 0.007781995580012662783, 0.000000000000000000, -0.9999697198139514409 ) ) ;
#3739 = ORIENTED_EDGE ( 'NONE', *, *, #43733, .F. ) ;
#3740 = LINE ( 'NONE', #47777, #35884 ) ;
#3741 = ORIENTED_EDGE ( 'NONE', *, *, #39483, .F. ) ;
#3742 = EDGE_CURVE ( 'NONE', #21263, #55546, #15180, .T. ) ;
#3743 = LINE ( 'NONE', #25921, #14695 ) ;
#3744 = LINE ( 'NONE', #29889, #55585 ) ;
#3746 = ADVANCED_FACE ( 'NONE', ( #14598 ), #14345, .F. ) ;
#3745 = ORIENTED_EDGE ( 'NONE', *, *, #55058, .T. ) ;
#3747 = DIRECTION ( 'NONE',  ( 0.6427681459581294776, -0.7660444431189769032, 0.005002170337467562802 ) ) ;
#3748 = CARTESIAN_POINT ( 'NONE',  ( -17.73140113748535285, 0.000000000000000000, 13.85752530597602039 ) ) ;
#3749 = PLANE ( 'NONE',  #37824 ) ;
#3750 = DIRECTION ( 'NONE',  ( 0.9999697198139515519, 0.000000000000000000, 0.007781995580013368816 ) ) ;
#3751 = ADVANCED_FACE ( 'NONE', ( #19126 ), #49232, .F. ) ;
#3752 = VERTEX_POINT ( 'NONE', #14884 ) ;
#3753 = AXIS2_PLACEMENT_3D ( 'NONE', #49561, #26856, #1820 ) ;
#3754 = VECTOR ( 'NONE', #35210, 1000.000000000000114 ) ;
#3755 = DIRECTION ( 'NONE',  ( -2.710505431213760161E-17, 4.336808689942016257E-16, -1.000000000000000000 ) ) ;
#3756 = EDGE_CURVE ( 'NONE', #7643, #16969, #49536, .T. ) ;
#3757 = FACE_OUTER_BOUND ( 'NONE', #26067, .T. ) ;
#3758 = CARTESIAN_POINT ( 'NONE',  ( -9.751071550147864642, -0.1191753592594205075, 1.889868501687798741 ) ) ;
#3759 = DIRECTION ( 'NONE',  ( 0.005002170337468016433, -0.7660444431189770143, -0.6427681459581293666 ) ) ;
#3760 = DIRECTION ( 'NONE',  ( -0.9999697198139514409, -0.000000000000000000, -0.007781995580013368816 ) ) ;
#3761 = DIRECTION ( 'NONE',  ( 0.007781995580012663651, 0.000000000000000000, -0.9999697198139515519 ) ) ;
#3762 = VECTOR ( 'NONE', #52967, 999.9999999999998863 ) ;
#3763 = ORIENTED_EDGE ( 'NONE', *, *, #25850, .T. ) ;
#3764 = CARTESIAN_POINT ( 'NONE',  ( 2.072287782118878319, 0.000000000000000000, -2.950529333540147015 ) ) ;
#3765 = DIRECTION ( 'NONE',  ( 0.000000000000000000, -1.000000000000000000, 0.000000000000000000 ) ) ;
#3766 = CARTESIAN_POINT ( 'NONE',  ( -16.13086958175276919, -2.622721114510659479, 3.063420134365714809 ) ) ;
#3767 = VERTEX_POINT ( 'NONE', #45519 ) ;
#3768 = FACE_OUTER_BOUND ( 'NONE', #49837, .T. ) ;
#3769 = ORIENTED_EDGE ( 'NONE', *, *, #11557, .T. ) ;
#3770 = DIRECTION ( 'NONE',  ( -0.7660212471507179544, -0.6427876096865405842, -0.005961354470445141482 ) ) ;
#3771 = CARTESIAN_POINT ( 'NONE',  ( -8.875996589204540044, 0.000000000000000000, 10.41778544861944233 ) ) ;
#3772 = ADVANCED_FACE ( 'NONE', ( #10350 ), #23413, .F. ) ;
#3773 = CARTESIAN_POINT ( 'NONE',  ( -17.73140113748535285, 0.000000000000000000, 13.85752530597602039 ) ) ;
#3774 = VECTOR ( 'NONE', #31503, 1000.000000000000227 ) ;
#3775 = CARTESIAN_POINT ( 'NONE',  ( -68.15687750496505259, 0.1329650153340585228, 4.357869429823836960 ) ) ;
#3776 = ORIENTED_EDGE ( 'NONE', *, *, #20339, .F. ) ;
#3777 = ORIENTED_EDGE ( 'NONE', *, *, #24800, .T. ) ;
#3778 = CARTESIAN_POINT ( 'NONE',  ( -67.13280394075316337, -0.6010134810807099548, -1.671631898859742060 ) ) ;
#3779 = CARTESIAN_POINT ( 'NONE',  ( 5.618093942130458096, -1.050357310661657939, 2.260478214906367800 ) ) ;
#3780 = DIRECTION ( 'NONE',  ( -0.5449076811759708816, 0.6444004775717707689, 0.5364919789714475140 ) ) ;
#3781 = ADVANCED_FACE ( 'NONE', ( #1800 ), #19409, .F. ) ;
#3782 = CARTESIAN_POINT ( 'NONE',  ( -21.66636548695712250, -3.108426967578159950, 5.198098170517139849 ) ) ;
#3783 = FACE_OUTER_BOUND ( 'NONE', #50688, .T. ) ;
#3784 = EDGE_CURVE ( 'NONE', #40645, #45163, #45001, .T. ) ;
#3785 = DIRECTION ( 'NONE',  ( -0.2426528472758541499, 0.7422098413412800966, -0.6246952433987894571 ) ) ;
#3786 = ORIENTED_EDGE ( 'NONE', *, *, #16463, .F. ) ;
#3787 = LINE ( 'NONE', #29072, #21101 ) ;
#3788 = EDGE_CURVE ( 'NONE', #42922, #32724, #35930, .T. ) ;
#3789 = LINE ( 'NONE', #21111, #45069 ) ;
#3790 = CARTESIAN_POINT ( 'NONE',  ( -17.76560056444620272, -4.565544526780662693, 3.636418925093014121 ) ) ;
#3791 = VERTEX_POINT ( 'NONE', #27959 ) ;
#3792 = LINE ( 'NONE', #8079, #24755 ) ;
#3793 = CARTESIAN_POINT ( 'NONE',  ( -16.73072885558310929, 0.000000000000000000, 4.690204724992056207 ) ) ;
#3794 = CARTESIAN_POINT ( 'NONE',  ( -12.24460538506144580, -1.327505506330657781, 1.595187301382279488 ) ) ;
#3795 = ORIENTED_EDGE ( 'NONE', *, *, #30079, .F. ) ;
#3796 = VECTOR ( 'NONE', #18535, 1000.000000000000114 ) ;
#3797 = VECTOR ( 'NONE', #43253, 999.9999999999998863 ) ;
#3798 = DIRECTION ( 'NONE',  ( -0.6427681459581293666, -0.7660444431189770143, -0.005002170337467561935 ) ) ;
#3799 = VERTEX_POINT ( 'NONE', #53764 ) ;
#3800 = EDGE_CURVE ( 'NONE', #40584, #33081, #23952, .T. ) ;
#3801 = EDGE_LOOP ( 'NONE', ( #49292, #19039, #48026, #9314, #35593 ) ) ;
#3802 = ORIENTED_EDGE ( 'NONE', *, *, #47332, .F. ) ;
#3803 = VECTOR ( 'NONE', #6295, 1000.000000000000114 ) ;
#3804 = VERTEX_POINT ( 'NONE', #50053 ) ;
#3805 = FACE_OUTER_BOUND ( 'NONE', #21835, .T. ) ;
#3806 = ORIENTED_EDGE ( 'NONE', *, *, #31549, .F. ) ;
#3807 = CARTESIAN_POINT ( 'NONE',  ( -16.84012618763835434, -0.1191753592594188005, 5.897352607188737217 ) ) ;
#3808 = ORIENTED_EDGE ( 'NONE', *, *, #48998, .T. ) ;
#3809 = CARTESIAN_POINT ( 'NONE',  ( -11.42723989371472548, -0.3560938001956568399, 1.308687906018629166 ) ) ;
#3810 = ORIENTED_EDGE ( 'NONE', *, *, #21752, .F. ) ;
#3811 = VECTOR ( 'NONE', #16978, 1000.000000000000114 ) ;
#3812 = ORIENTED_EDGE ( 'NONE', *, *, #56007, .T. ) ;
#3813 = VECTOR ( 'NONE', #23785, 1000.000000000000227 ) ;
#3814 = DIRECTION ( 'NONE',  ( -0.7660212471507179544, -0.6427876096865405842, -0.005961354470445141482 ) ) ;
#3815 = DIRECTION ( 'NONE',  ( 0.5449076811759707706, 0.6444004775717708799, -0.5364919789714476250 ) ) ;
#3816 = PLANE ( 'NONE',  #33117 ) ;
#3817 = FACE_OUTER_BOUND ( 'NONE', #29021, .T. ) ;
#3818 = LINE ( 'NONE', #15762, #5686 ) ;
#3819 = VERTEX_POINT ( 'NONE', #11165 ) ;
#3820 = ORIENTED_EDGE ( 'NONE', *, *, #22266, .F. ) ;
#3821 = CARTESIAN_POINT ( 'NONE',  ( 2.072287782118878319, 0.000000000000000000, -2.950529333540147015 ) ) ;
#3822 = EDGE_CURVE ( 'NONE', #34361, #51066, #10057, .T. ) ;
#3823 = DIRECTION ( 'NONE',  ( 0.9659258262890682012, -0.2588190451025213501, 0.000000000000000000 ) ) ;
#3824 = VECTOR ( 'NONE', #41146, 1000.000000000000227 ) ;
#3825 = LINE ( 'NONE', #21153, #16093 ) ;
#3826 = DIRECTION ( 'NONE',  ( 0.5449076811759707706, 0.6444004775717708799, -0.5364919789714476250 ) ) ;
#3827 = DIRECTION ( 'NONE',  ( 0.007781995580012662783, 0.000000000000000000, -0.9999697198139514409 ) ) ;
#3828 = CARTESIAN_POINT ( 'NONE',  ( -23.33849165029409889, 0.000000000000000000, 5.946783852668351855 ) ) ;
#3829 = ORIENTED_EDGE ( 'NONE', *, *, #37551, .T. ) ;
#3831 = CARTESIAN_POINT ( 'NONE',  ( -17.39404204199770376, 0.000000000000000000, 4.515716654813066278 ) ) ;
#3830 = VECTOR ( 'NONE', #21801, 1000.000000000000227 ) ;
#3832 = CARTESIAN_POINT ( 'NONE',  ( -19.99336569310255740, 0.000000000000000000, 5.972816396352070178 ) ) ;
#3833 = ORIENTED_EDGE ( 'NONE', *, *, #50571, .F. ) ;
#3834 = ADVANCED_FACE ( 'NONE', ( #44690 ), #25361, .F. ) ;
#3835 = VECTOR ( 'NONE', #31745, 1000.000000000000227 ) ;
#3836 = VECTOR ( 'NONE', #19329, 1000.000000000000227 ) ;
#3837 = DIRECTION ( 'NONE',  ( 0.007781995580012662783, 0.000000000000000000, -0.9999697198139514409 ) ) ;
#3838 = DIRECTION ( 'NONE',  ( 0.7660212471507180654, -0.6427876096865404731, 0.005961354470445141482 ) ) ;
#3839 = CARTESIAN_POINT ( 'NONE',  ( 2.602374448188125350E-16, 2.000000000000000000, 2.125000000000000000 ) ) ;
#3840 = EDGE_CURVE ( 'NONE', #17107, #4086, #7466, .T. ) ;
#3841 = EDGE_CURVE ( 'NONE', #12750, #47914, #19964, .T. ) ;
#3842 = LINE ( 'NONE', #50143, #8744 ) ;
#3843 = ORIENTED_EDGE ( 'NONE', *, *, #35667, .T. ) ;
#3844 = VECTOR ( 'NONE', #525, 999.9999999999998863 ) ;
#3845 = VECTOR ( 'NONE', #40239, 999.9999999999998863 ) ;
#3846 = ORIENTED_EDGE ( 'NONE', *, *, #10440, .T. ) ;
#3847 = PLANE ( 'NONE',  #23951 ) ;
#3848 = CARTESIAN_POINT ( 'NONE',  ( -20.16419826038267260, 21.01647055225602401, 4.297939206181997207 ) ) ;
#3849 = CARTESIAN_POINT ( 'NONE',  ( -10.37421533196711465, -0.1191753592594197858, 10.96012406864405975 ) ) ;
#3850 = EDGE_CURVE ( 'NONE', #25320, #21782, #7768, .T. ) ;
#3851 = CARTESIAN_POINT ( 'NONE',  ( -22.02230563637845151, 19.67040402849924163, -4.420763475398227449 ) ) ;
#3852 = EDGE_CURVE ( 'NONE', #42332, #5412, #42662, .T. ) ;
#3853 = VECTOR ( 'NONE', #15237, 1000.000000000000114 ) ;
#3854 = CARTESIAN_POINT ( 'NONE',  ( -18.39746900504187010, 0.000000000000000000, 14.03700784672088808 ) ) ;
#3855 = CARTESIAN_POINT ( 'NONE',  ( 2.072287782118878319, 0.000000000000000000, -2.950529333540147015 ) ) ;
#3856 = CARTESIAN_POINT ( 'NONE',  ( -19.12962290826653700, 0.000000000000000000, 14.40064212555863854 ) ) ;
#3857 = ADVANCED_FACE ( 'NONE', ( #54587 ), #25098, .F. ) ;
#3858 = CARTESIAN_POINT ( 'NONE',  ( -50.45472955569960760, 3.742236127018431890, 5.000000000000000000 ) ) ;
#3859 = PLANE ( 'NONE',  #26922 ) ;
#3860 = FACE_OUTER_BOUND ( 'NONE', #50099, .T. ) ;
#3861 = VERTEX_POINT ( 'NONE', #29050 ) ;
#3862 = CARTESIAN_POINT ( 'NONE',  ( -12.66414222307914450, -0.1191753592594190225, 6.668515219616352852 ) ) ;
#3863 = EDGE_CURVE ( 'NONE', #19811, #13531, #16544, .T. ) ;
#3864 = ORIENTED_EDGE ( 'NONE', *, *, #48035, .F. ) ;
#3865 = ORIENTED_EDGE ( 'NONE', *, *, #3822, .T. ) ;
#3866 = ADVANCED_FACE ( 'NONE', ( #21081 ), #33875, .F. ) ;
#3867 = ORIENTED_EDGE ( 'NONE', *, *, #714, .T. ) ;
#3868 = EDGE_LOOP ( 'NONE', ( #33554, #45631, #19997 ) ) ;
#3869 = ORIENTED_EDGE ( 'NONE', *, *, #29298, .F. ) ;
#3870 = ORIENTED_EDGE ( 'NONE', *, *, #6691, .T. ) ;
#3871 = VECTOR ( 'NONE', #24820, 1000.000000000000227 ) ;
#3872 = CARTESIAN_POINT ( 'NONE',  ( -21.30476517517178436, 4.657758921906512306, 4.808819142744448882 ) ) ;
#3873 = CARTESIAN_POINT ( 'NONE',  ( -12.60458797795435615, 0.000000000000000000, 11.86609696750642229 ) ) ;
#3874 = LINE ( 'NONE', #46460, #20330 ) ;
#3875 = AXIS2_PLACEMENT_3D ( 'NONE', #52206, #47944, #52481 ) ;
#3876 = VECTOR ( 'NONE', #15494, 999.9999999999998863 ) ;
#3877 = ORIENTED_EDGE ( 'NONE', *, *, #48509, .T. ) ;
#3878 = LINE ( 'NONE', #21203, #53963 ) ;
#3879 = ORIENTED_EDGE ( 'NONE', *, *, #41297, .F. ) ;
#3880 = CARTESIAN_POINT ( 'NONE',  ( -19.22617103857668397, 4.333955019861509328, 11.46217741115471433 ) ) ;
#3881 = ORIENTED_EDGE ( 'NONE', *, *, #17818, .F. ) ;
#3882 = AXIS2_PLACEMENT_3D ( 'NONE', #2030, #49190, #10309 ) ;
#3883 = VECTOR ( 'NONE', #18095, 1000.000000000000000 ) ;
#3884 = PLANE ( 'NONE',  #30184 ) ;
#3885 = LINE ( 'NONE', #34007, #47308 ) ;
#3886 = DIRECTION ( 'NONE',  ( 0.005002170337468016433, -0.7660444431189770143, -0.6427681459581293666 ) ) ;
#3887 = EDGE_LOOP ( 'NONE', ( #8947, #2217, #37332, #24607 ) ) ;
#3888 = DIRECTION ( 'NONE',  ( 0.000000000000000000, -1.000000000000000000, 0.000000000000000000 ) ) ;
#3889 = ORIENTED_EDGE ( 'NONE', *, *, #36503, .T. ) ;
#3890 = DIRECTION ( 'NONE',  ( 0.9999697198139515519, 0.000000000000000000, 0.007781995580013368816 ) ) ;
#3891 = VECTOR ( 'NONE', #14337, 999.9999999999998863 ) ;
#3892 = ADVANCED_FACE ( 'NONE', ( #54897 ), #2907, .F. ) ;
#3893 = PLANE ( 'NONE',  #17572 ) ;
#3894 = AXIS2_PLACEMENT_3D ( 'NONE', #12116, #46189, #29149 ) ;
#3895 = DIRECTION ( 'NONE',  ( -0.7660212471507179544, -0.6427876096865405842, -0.005961354470445141482 ) ) ;
#3896 = PLANE ( 'NONE',  #9569 ) ;
#3897 = DIRECTION ( 'NONE',  ( 0.007781995580012662783, 0.000000000000000000, -0.9999697198139514409 ) ) ;
#3898 = LINE ( 'NONE', #30031, #10387 ) ;
#3899 = LINE ( 'NONE', #50760, #12137 ) ;
#3900 = DIRECTION ( 'NONE',  ( 0.9999697198139515519, 0.000000000000000000, 0.007781995580013368816 ) ) ;
#3901 = ORIENTED_EDGE ( 'NONE', *, *, #25657, .F. ) ;
#3902 = CARTESIAN_POINT ( 'NONE',  ( -19.99468334749183995, 0.000000000000000000, 6.142132155647047398 ) ) ;
#3903 = ORIENTED_EDGE ( 'NONE', *, *, #49899, .T. ) ;
#3904 = ADVANCED_FACE ( 'NONE', ( #50898 ), #29646, .F. ) ;
#3905 = VECTOR ( 'NONE', #43838, 999.9999999999998863 ) ;
#3906 = EDGE_CURVE ( 'NONE', #17592, #39633, #51197, .T. ) ;
#3907 = ADVANCED_FACE ( 'NONE', ( #3213 ), #55736, .F. ) ;
#3908 = DIRECTION ( 'NONE',  ( 0.5449076811759707706, 0.6444004775717708799, -0.5364919789714476250 ) ) ;
#3909 = DIRECTION ( 'NONE',  ( 0.9999697198139515519, 0.000000000000000000, 0.007781995580013368816 ) ) ;
#3910 = CARTESIAN_POINT ( 'NONE',  ( -17.93139508144814442, 0.000000000000000000, 13.85596890686001537 ) ) ;
#3911 = AXIS2_PLACEMENT_3D ( 'NONE', #9096, #31240, #1118 ) ;
#3912 = DIRECTION ( 'NONE',  ( -0.5449076811759708816, 0.6444004775717707689, 0.5364919789714475140 ) ) ;
#3913 = CARTESIAN_POINT ( 'NONE',  ( -12.56911515855031425, 0.000000000000000000, 7.307915853708490950 ) ) ;
#3914 = EDGE_CURVE ( 'NONE', #49603, #49579, #33334, .T. ) ;
#3915 = FACE_OUTER_BOUND ( 'NONE', #2107, .T. ) ;
#3916 = ITEM_DEFINED_TRANSFORMATION ( 'NONE', 'NONE', #42584,  #2610 ) ;
#3917 = VERTEX_POINT ( 'NONE', #20809 ) ;
#3918 = AXIS2_PLACEMENT_3D ( 'NONE', #48578, #47754, #43219 ) ;
#3919 = DIRECTION ( 'NONE',  ( -0.005002170337468016433, -0.7660444431189770143, 0.6427681459581293666 ) ) ;
#3920 = FACE_OUTER_BOUND ( 'NONE', #45311, .T. ) ;
#3921 = DIRECTION ( 'NONE',  ( 0.9999697198139515519, 0.000000000000000000, 0.007781995580013368816 ) ) ;
#3922 = AXIS2_PLACEMENT_3D ( 'NONE', #49264, #35961, #5544 ) ;
#3923 = VECTOR ( 'NONE', #34377, 1000.000000000000000 ) ;
#3924 = LINE ( 'NONE', #52478, #14635 ) ;
#3925 = EDGE_CURVE ( 'NONE', #428, #13272, #25627, .T. ) ;
#3926 = DIRECTION ( 'NONE',  ( 0.9999697198139515519, 0.000000000000000000, 0.007781995580013368816 ) ) ;
#3927 = DIRECTION ( 'NONE',  ( -0.005961354470445682716, -0.6427876096865404731, 0.7660212471507180654 ) ) ;
#3928 = CARTESIAN_POINT ( 'NONE',  ( 2.072287782118878319, 0.000000000000000000, -2.950529333540147015 ) ) ;
#3929 = VERTEX_POINT ( 'NONE', #46949 ) ;
#3930 = ADVANCED_FACE ( 'NONE', ( #8050 ), #2639, .F. ) ;
#3931 = VECTOR ( 'NONE', #41468, 1000.000000000000000 ) ;
#3932 = DIRECTION ( 'NONE',  ( 0.9999697198139515519, 0.000000000000000000, 0.007781995580013368816 ) ) ;
#3933 = VECTOR ( 'NONE', #48905, 999.9999999999998863 ) ;
#3934 = CARTESIAN_POINT ( 'NONE',  ( -23.33849165029409889, 0.000000000000000000, 5.946783852668351855 ) ) ;
#3935 = ORIENTED_EDGE ( 'NONE', *, *, #53244, .T. ) ;
#3936 = ADVANCED_FACE ( 'NONE', ( #29336 ), #46092, .F. ) ;
#3937 = ORIENTED_EDGE ( 'NONE', *, *, #27808, .F. ) ;
#3938 = DIRECTION ( 'NONE',  ( 0.007781995580012663651, 0.000000000000000000, -0.9999697198139515519 ) ) ;
#3939 = ADVANCED_FACE ( 'NONE', ( #25937 ), #30478, .F. ) ;
#3940 = ORIENTED_EDGE ( 'NONE', *, *, #55010, .T. ) ;
#3941 = ORIENTED_EDGE ( 'NONE', *, *, #53311, .T. ) ;
#3942 = ORIENTED_EDGE ( 'NONE', *, *, #40428, .T. ) ;
#3943 = ORIENTED_EDGE ( 'NONE', *, *, #51392, .F. ) ;
#3944 = VECTOR ( 'NONE', #49207, 1000.000000000000114 ) ;
#3945 = CARTESIAN_POINT ( 'NONE',  ( -19.60834386242827776, 0.000000000000000000, 4.298478389818581213 ) ) ;
#3946 = ORIENTED_EDGE ( 'NONE', *, *, #3320, .F. ) ;
#3947 = DIRECTION ( 'NONE',  ( -0.5364919789714478471, 0.6444004775717705469, -0.5449076811759709926 ) ) ;
#3948 = CARTESIAN_POINT ( 'NONE',  ( -13.91947430141211584, 1.419719901456504507, 2.043431759590222718 ) ) ;
#3949 = VECTOR ( 'NONE', #11593, 999.9999999999998863 ) ;
#3950 = ORIENTED_EDGE ( 'NONE', *, *, #15506, .F. ) ;
#3951 = VERTEX_POINT ( 'NONE', #13145 ) ;
#3952 = AXIS2_PLACEMENT_3D ( 'NONE', #17630, #4, #38360 ) ;
#3953 = DIRECTION ( 'NONE',  ( 0.000000000000000000, -0.000000000000000000, -1.000000000000000000 ) ) ;
#3954 = CARTESIAN_POINT ( 'NONE',  ( -13.89383709357448282, -0.5179957512181557755, 2.261632504550268763 ) ) ;
#3955 = ORIENTED_EDGE ( 'NONE', *, *, #20590, .T. ) ;
#3956 = VECTOR ( 'NONE', #41846, 1000.000000000000227 ) ;
#3957 = CARTESIAN_POINT ( 'NONE',  ( -20.28683642378279117, 0.1245042932765029059, 4.558055603545987822 ) ) ;
#3958 = DIRECTION ( 'NONE',  ( 0.007781995580012663651, -3.146120232559066537E-19, -0.9999697198139514409 ) ) ;
#3959 = ORIENTED_EDGE ( 'NONE', *, *, #34204, .T. ) ;
#3960 = PLANE ( 'NONE',  #10410 ) ;
#3961 = EDGE_CURVE ( 'NONE', #25102, #1588, #52860, .T. ) ;
#3962 = VECTOR ( 'NONE', #698, 1000.000000000000114 ) ;
#3963 = VERTEX_POINT ( 'NONE', #17681 ) ;
#3964 = FACE_OUTER_BOUND ( 'NONE', #56057, .T. ) ;
#3965 = EDGE_CURVE ( 'NONE', #23095, #41647, #43264, .T. ) ;
#3966 = AXIS2_PLACEMENT_3D ( 'NONE', #39829, #9158, #22521 ) ;
#3967 = PLANE ( 'NONE',  #6430 ) ;
#3968 = VECTOR ( 'NONE', #55064, 999.9999999999998863 ) ;
#3969 = ORIENTED_EDGE ( 'NONE', *, *, #41662, .F. ) ;
#3970 = LINE ( 'NONE', #11917, #30396 ) ;
#3971 = DIRECTION ( 'NONE',  ( -0.3313982828793700652, 0.4028455766673916250, -0.8531650599175529814 ) ) ;
#3972 = LINE ( 'NONE', #55363, #17586 ) ;
#3973 = DIRECTION ( 'NONE',  ( 0.5449076811759707706, 0.6444004775717708799, -0.5364919789714476250 ) ) ;
#3974 = ORIENTED_EDGE ( 'NONE', *, *, #35887, .F. ) ;
#3975 = EDGE_CURVE ( 'NONE', #37937, #52731, #21387, .T. ) ;
#3976 = ADVANCED_FACE ( 'NONE', ( #56031, #44080 ), #646, .T. ) ;
#3977 = EDGE_CURVE ( 'NONE', #41994, #11772, #52331, .T. ) ;
#3978 = PLANE ( 'NONE',  #54572 ) ;
#3979 = CARTESIAN_POINT ( 'NONE',  ( -14.66887761629205222, 0.000000000000000000, 12.58869632783390990 ) ) ;
#3980 = PLANE ( 'NONE',  #1312 ) ;
#3981 = DIRECTION ( 'NONE',  ( 1.007958083594381472E-15, -3.869188571150966132E-16, 1.000000000000000000 ) ) ;
#3982 = EDGE_CURVE ( 'NONE', #21963, #34820, #42952, .T. ) ;
#3983 = CARTESIAN_POINT ( 'NONE',  ( -18.32501161783028110, -2.460819163488160655, 3.920864934442803040 ) ) ;
#3984 = DIRECTION ( 'NONE',  ( -0.7660212471507179544, -0.6427876096865405842, -0.005961354470445141482 ) ) ;
#3985 = LINE ( 'NONE', #18159, #3016 ) ;
#3986 = LINE ( 'NONE', #4294, #41302 ) ;
#3987 = CIRCLE ( 'NONE', #7590, 3.692809041582069352 ) ;
#3988 = VERTEX_POINT ( 'NONE', #30750 ) ;
#3989 = CARTESIAN_POINT ( 'NONE',  ( 2.072287782118878319, 0.000000000000000000, -2.950529333540147015 ) ) ;
#3990 = ORIENTED_EDGE ( 'NONE', *, *, #45835, .T. ) ;
#3991 = PLANE ( 'NONE',  #46517 ) ;
#3992 = MANIFOLD_SOLID_BREP ( 'Boss-Extrude3', #22238 ) ;
#3993 = CARTESIAN_POINT ( 'NONE',  ( -27.06552663992790997, 0.000000000000000000, 7.195101427592543786 ) ) ;
#3994 = AXIS2_PLACEMENT_3D ( 'NONE', #9213, #16917, #4964 ) ;
#3995 = DIRECTION ( 'NONE',  ( 0.5449076811759707706, 0.6444004775717708799, -0.5364919789714476250 ) ) ;
#3996 = AXIS2_PLACEMENT_3D ( 'NONE', #7317, #29177, #55298 ) ;
#3997 = CARTESIAN_POINT ( 'NONE',  ( 1.086233639165236964, 0.000000000000000000, 2.796443541562362078 ) ) ;
#3998 = EDGE_CURVE ( 'NONE', #13117, #49510, #35549, .T. ) ;
#3999 = CARTESIAN_POINT ( 'NONE',  ( -13.60152578229115505, -0.1117717739994002479, 8.501668099265545564 ) ) ;
#4000 = ORIENTED_EDGE ( 'NONE', *, *, #19227, .F. ) ;
#4001 = ADVANCED_FACE ( 'NONE', ( #30175 ), #21667, .F. ) ;
#4002 = ORIENTED_EDGE ( 'NONE', *, *, #5169, .T. ) ;
#4003 = EDGE_CURVE ( 'NONE', #56039, #14373, #8606, .T. ) ;
#4004 = LINE ( 'NONE', #42615, #50400 ) ;
#4005 = VECTOR ( 'NONE', #5772, 1000.000000000000227 ) ;
#4006 = FACE_OUTER_BOUND ( 'NONE', #15641, .T. ) ;
#4007 = ORIENTED_EDGE ( 'NONE', *, *, #29411, .F. ) ;
#4008 = VECTOR ( 'NONE', #1466, 1000.000000000000114 ) ;
#4009 = FACE_OUTER_BOUND ( 'NONE', #1359, .T. ) ;
#4010 = ADVANCED_FACE ( 'NONE', ( #13683 ), #30996, .F. ) ;
#4011 = EDGE_LOOP ( 'NONE', ( #28267, #55445, #12491, #53597 ) ) ;
#4012 = CARTESIAN_POINT ( 'NONE',  ( -21.47263955680318404, 0.000000000000000000, 5.022634149262071190 ) ) ;
#4013 = ORIENTED_EDGE ( 'NONE', *, *, #29746, .F. ) ;
#4014 = LINE ( 'NONE', #28747, #12967 ) ;
#4015 = EDGE_CURVE ( 'NONE', #21230, #9004, #40085, .T. ) ;
#4016 = VECTOR ( 'NONE', #791, 999.9999999999998863 ) ;
#4017 = ORIENTED_EDGE ( 'NONE', *, *, #55575, .F. ) ;
#4018 = VECTOR ( 'NONE', #18303, 999.9999999999998863 ) ;
#4019 = ORIENTED_EDGE ( 'NONE', *, *, #10225, .F. ) ;
#4020 = ORIENTED_EDGE ( 'NONE', *, *, #21577, .T. ) ;
#4021 = FACE_OUTER_BOUND ( 'NONE', #50685, .T. ) ;
#4022 = CARTESIAN_POINT ( 'NONE',  ( -13.73672976910459909, 0.000000000000000000, 12.22661844811216270 ) ) ;
#4023 = LINE ( 'NONE', #3461, #48429 ) ;
#4024 = CARTESIAN_POINT ( 'NONE',  ( -10.47421230394850866, 0.000000000000000000, 10.95934586908605723 ) ) ;
#4025 = VERTEX_POINT ( 'NONE', #28144 ) ;
#4026 = ORIENTED_EDGE ( 'NONE', *, *, #35168, .F. ) ;
#4027 = AXIS2_PLACEMENT_3D ( 'NONE', #41047, #46142, #45878 ) ;
#4028 = EDGE_LOOP ( 'NONE', ( #26060, #54634 ) ) ;
#4029 = LINE ( 'NONE', #7433, #1414 ) ;
#4030 = DIRECTION ( 'NONE',  ( 0.007781995580012663651, 0.000000000000000000, -0.9999697198139515519 ) ) ;
#4031 = VECTOR ( 'NONE', #30379, 1000.000000000000227 ) ;
#4032 = VERTEX_POINT ( 'NONE', #36676 ) ;
#4033 = DIRECTION ( 'NONE',  ( -0.5364919789714478471, 0.6444004775717705469, -0.5449076811759709926 ) ) ;
#4034 = ORIENTED_EDGE ( 'NONE', *, *, #44223, .T. ) ;
#4035 = VECTOR ( 'NONE', #38334, 1000.000000000000114 ) ;
#4036 = FACE_OUTER_BOUND ( 'NONE', #24428, .T. ) ;
#4037 = CARTESIAN_POINT ( 'NONE',  ( -28.92982233430281980, 0.000000000000000000, 7.919257187036034651 ) ) ;
#4038 = VERTEX_POINT ( 'NONE', #1740 ) ;
#4039 = CARTESIAN_POINT ( 'NONE',  ( -22.43336023615409047, -5.051250379848161387, 13.68577311371102567 ) ) ;
#4040 = EDGE_LOOP ( 'NONE', ( #4527, #28209, #32537, #50784 ) ) ;
#4041 = DIRECTION ( 'NONE',  ( 0.007781995580012662783, 0.000000000000000000, -0.9999697198139514409 ) ) ;
#4042 = DIRECTION ( 'NONE',  ( 0.9999697198139515519, 0.000000000000000000, 0.007781995580013368816 ) ) ;
#4043 = VECTOR ( 'NONE', #44228, 999.9999999999998863 ) ;
#4044 = ORIENTED_EDGE ( 'NONE', *, *, #50823, .F. ) ;
#4045 = LINE ( 'NONE', #17111, #19571 ) ;
#4046 = LINE ( 'NONE', #38397, #47457 ) ;
#4047 = AXIS2_PLACEMENT_3D ( 'NONE', #46006, #50545, #12189 ) ;
#4048 = CARTESIAN_POINT ( 'NONE',  ( -10.68625748875443016, 0.000000000000000000, 4.198586115423438514 ) ) ;
#4049 = ORIENTED_EDGE ( 'NONE', *, *, #41228, .F. ) ;
#4050 = VECTOR ( 'NONE', #33033, 1000.000000000000000 ) ;
#4051 = ADVANCED_FACE ( 'NONE', ( #15363 ), #15130, .T. ) ;
#4052 = LINE ( 'NONE', #9141, #17382 ) ;
#4053 = CARTESIAN_POINT ( 'NONE',  ( -68.61315424319464285, 1.787077962669009867, 7.471997583267850018 ) ) ;
#4054 = LINE ( 'NONE', #38406, #52203 ) ;
#4055 = EDGE_CURVE ( 'NONE', #10808, #55191, #46883, .T. ) ;
#4056 = ADVANCED_FACE ( 'NONE', ( #15626 ), #41746, .F. ) ;
#4057 = CARTESIAN_POINT ( 'NONE',  ( -27.99767448711536133, 0.000000000000000000, 7.557179307314289218 ) ) ;
#4058 = LINE ( 'NONE', #50897, #16130 ) ;
#4059 = CIRCLE ( 'NONE', #6771, 2.749999999999997335 ) ;
#4060 = VECTOR ( 'NONE', #29509, 1000.000000000000114 ) ;
#4061 = DIRECTION ( 'NONE',  ( -0.5449076811759708816, 0.6444004775717707689, 0.5364919789714475140 ) ) ;
#4062 = EDGE_LOOP ( 'NONE', ( #33383, #6408, #9272, #13183 ) ) ;
#4063 = CARTESIAN_POINT ( 'NONE',  ( -18.13194405223293515, 0.000000000000000000, 5.617970340166344556 ) ) ;
#4064 = DIRECTION ( 'NONE',  ( 0.005961354470445682716, -0.6427876096865404731, -0.7660212471507180654 ) ) ;
#4065 = DIRECTION ( 'NONE',  ( 0.000000000000000000, 1.000000000000000000, 0.000000000000000000 ) ) ;
#4066 = ORIENTED_EDGE ( 'NONE', *, *, #49513, .F. ) ;
#4067 = CARTESIAN_POINT ( 'NONE',  ( -19.24265873919813430, -5.213152330870665097, 4.189496401723858732 ) ) ;
#4068 = DIRECTION ( 'NONE',  ( 0.000000000000000000, -0.000000000000000000, -1.000000000000000000 ) ) ;
#4069 = ORIENTED_EDGE ( 'NONE', *, *, #13133, .T. ) ;
#4070 = CARTESIAN_POINT ( 'NONE',  ( -23.29661890453421691, 19.01267837833611551, -4.488312987714206059 ) ) ;
#4071 = LINE ( 'NONE', #42671, #8621 ) ;
#4072 = CARTESIAN_POINT ( 'NONE',  ( -14.10280672071693431, -0.1191753592594197858, 12.40843558753103792 ) ) ;
#4073 = CARTESIAN_POINT ( 'NONE',  ( -69.63118656663708350, 0.1323540994886103217, 7.053755868282808983 ) ) ;
#4074 = VECTOR ( 'NONE', #54463, 1000.000000000000227 ) ;
#4075 = ORIENTED_EDGE ( 'NONE', *, *, #12242, .F. ) ;
#4076 = ORIENTED_EDGE ( 'NONE', *, *, #34202, .T. ) ;
#4077 = VECTOR ( 'NONE', #35395, 999.9999999999998863 ) ;
#4078 = CARTESIAN_POINT ( 'NONE',  ( -67.30049973920597495, -0.6012074100331669113, -2.670129092015942618 ) ) ;
#4079 = PLANE ( 'NONE',  #3257 ) ;
#4080 = PLANE ( 'NONE',  #26106 ) ;
#4081 = AXIS2_PLACEMENT_3D ( 'NONE', #10660, #27114, #39888 ) ;
#4082 = DIRECTION ( 'NONE',  ( 0.007781995580012663651, -3.146120232559066537E-19, -0.9999697198139514409 ) ) ;
#4083 = LINE ( 'NONE', #12337, #35540 ) ;
#4084 = DIRECTION ( 'NONE',  ( 0.005002170337468016433, -0.7660444431189770143, -0.6427681459581293666 ) ) ;
#4085 = AXIS2_PLACEMENT_3D ( 'NONE', #18495, #5443, #48038 ) ;
#4086 = VERTEX_POINT ( 'NONE', #29571 ) ;
#4087 = CARTESIAN_POINT ( 'NONE',  ( -70.10169143752739274, -0.9999999999999995559, 7.503902134509972122 ) ) ;
#4088 = EDGE_CURVE ( 'NONE', #13096, #45339, #33802, .T. ) ;
#4089 = CARTESIAN_POINT ( 'NONE',  ( -18.67775241435682432, 0.000000000000000000, 4.136394454059623804 ) ) ;
#4090 = AXIS2_PLACEMENT_3D ( 'NONE', #29696, #46990, #34477 ) ;
#4092 = VERTEX_POINT ( 'NONE', #3434 ) ;
#4091 = AXIS2_PLACEMENT_3D ( 'NONE', #42033, #28725, #25023 ) ;
#4093 = EDGE_CURVE ( 'NONE', #47084, #291, #11929, .T. ) ;
#4094 = VECTOR ( 'NONE', #46295, 1000.000000000000114 ) ;
#4095 = AXIS2_PLACEMENT_3D ( 'NONE', #52990, #49007, #6159 ) ;
#4096 = CARTESIAN_POINT ( 'NONE',  ( -26.13493519185646008, 0.000000000000000000, 7.033017491833586377 ) ) ;
#4097 = CARTESIAN_POINT ( 'NONE',  ( -11.36945030497927789, 0.000000000000000000, 6.578587783380987375 ) ) ;
#4098 = ADVANCED_FACE ( 'NONE', ( #11392 ), #7988, .F. ) ;
#4099 = CARTESIAN_POINT ( 'NONE',  ( -9.542064456761055524, 0.000000000000000000, 10.59726798936431180 ) ) ;
#4100 = VECTOR ( 'NONE', #30103, 999.9999999999998863 ) ;
#4101 = ORIENTED_EDGE ( 'NONE', *, *, #5244, .T. ) ;
#4102 = LINE ( 'NONE', #12352, #20311 ) ;
#4103 = EDGE_CURVE ( 'NONE', #20460, #40803, #46285, .T. ) ;
#4104 = VERTEX_POINT ( 'NONE', #55374 ) ;
#4105 = VECTOR ( 'NONE', #44639, 1000.000000000000227 ) ;
#4106 = EDGE_LOOP ( 'NONE', ( #43685, #39669, #51110, #44680 ) ) ;
#4107 = VECTOR ( 'NONE', #26526, 1000.000000000000000 ) ;
#4108 = EDGE_LOOP ( 'NONE', ( #16444, #19843, #55183, #6160, #885 ) ) ;
#4109 = ORIENTED_EDGE ( 'NONE', *, *, #10021, .T. ) ;
#4110 = FACE_OUTER_BOUND ( 'NONE', #46545, .T. ) ;
#4111 = ORIENTED_EDGE ( 'NONE', *, *, #51080, .T. ) ;
#4112 = LINE ( 'NONE', #29384, #17712 ) ;
#4113 = ORIENTED_EDGE ( 'NONE', *, *, #51878, .T. ) ;
#4114 = LINE ( 'NONE', #12366, #29539 ) ;
#4115 = EDGE_LOOP ( 'NONE', ( #8416, #31665, #54866, #30897 ) ) ;
#4116 = FACE_OUTER_BOUND ( 'NONE', #51961, .T. ) ;
#4117 = ORIENTED_EDGE ( 'NONE', *, *, #16794, .T. ) ;
#4118 = AXIS2_PLACEMENT_3D ( 'NONE', #38499, #12403, #55830 ) ;
#4119 = CARTESIAN_POINT ( 'NONE',  ( -10.90193935463291375, 0.000000000000000000, 6.212893991891234258 ) ) ;
#4120 = VECTOR ( 'NONE', #42359, 999.9999999999998863 ) ;
#4121 = LINE ( 'NONE', #29954, #29598 ) ;
#4122 = DIRECTION ( 'NONE',  ( 0.005961354470445682716, -0.6427876096865404731, -0.7660212471507180654 ) ) ;
#4123 = PLANE ( 'NONE',  #571 ) ;
#4124 = EDGE_CURVE ( 'NONE', #34978, #31046, #7392, .T. ) ;
#4125 = CARTESIAN_POINT ( 'NONE',  ( -12.33850799832341849, 0.000000000000000000, 11.68350162852954632 ) ) ;
#4126 = VECTOR ( 'NONE', #54667, 1000.000000000000227 ) ;
#4127 = ORIENTED_EDGE ( 'NONE', *, *, #24960, .F. ) ;
#4128 = ADVANCED_FACE ( 'NONE', ( #19900 ), #20474, .F. ) ;
#4129 = ORIENTED_EDGE ( 'NONE', *, *, #51950, .F. ) ;
#4130 = CARTESIAN_POINT ( 'NONE',  ( 5.058454994527578741, -1.127275664452432880, 2.289010529401726224 ) ) ;
#4131 = CARTESIAN_POINT ( 'NONE',  ( -17.79814051637334416, -0.1191753592594177180, 9.583217816230360953 ) ) ;
#4132 = VECTOR ( 'NONE', #16845, 1000.000000000000227 ) ;
#4133 = EDGE_CURVE ( 'NONE', #15482, #24338, #46572, .T. ) ;
#4134 = EDGE_CURVE ( 'NONE', #25745, #47834, #55116, .T. ) ;
#4135 = LINE ( 'NONE', #12918, #25188 ) ;
#4136 = VECTOR ( 'NONE', #16248, 1000.000000000000000 ) ;
#4137 = VECTOR ( 'NONE', #33076, 1000.000000000000114 ) ;
#4138 = DIRECTION ( 'NONE',  ( -0.005961354470445682716, -0.6427876096865404731, 0.7660212471507180654 ) ) ;
#4139 = CARTESIAN_POINT ( 'NONE',  ( -24.27063949748155380, 0.000000000000000000, 6.308861732390097288 ) ) ;
#4140 = LINE ( 'NONE', #42474, #28645 ) ;
#4141 = ORIENTED_EDGE ( 'NONE', *, *, #1948, .F. ) ;
#4142 = PLANE ( 'NONE',  #39276 ) ;
#4143 = LINE ( 'NONE', #30814, #42173 ) ;
#4144 = ORIENTED_EDGE ( 'NONE', *, *, #12828, .T. ) ;
#4145 = VECTOR ( 'NONE', #34317, 1000.000000000000114 ) ;
#4146 = LINE ( 'NONE', #51819, #39771 ) ;
#4147 = CARTESIAN_POINT ( 'NONE',  ( -14.69394934065806346, 0.1245042932765029059, 2.385588325215514782 ) ) ;
#4148 = VECTOR ( 'NONE', #45780, 1000.000000000000227 ) ;
#4149 = CARTESIAN_POINT ( 'NONE',  ( -22.65299646082626239, 19.57956224127125111, 4.449815307286153043 ) ) ;
#4150 = DIRECTION ( 'NONE',  ( 0.5449076811759707706, 0.6444004775717708799, -0.5364919789714476250 ) ) ;
#4151 = EDGE_CURVE ( 'NONE', #994, #45407, #14068, .T. ) ;
#4152 = AXIS2_PLACEMENT_3D ( 'NONE', #25449, #3591, #55543 ) ;
#4153 = ORIENTED_EDGE ( 'NONE', *, *, #41885, .T. ) ;
#4154 = VECTOR ( 'NONE', #7203, 1000.000000000000227 ) ;
#4155 = ORIENTED_EDGE ( 'NONE', *, *, #51174, .T. ) ;
#4156 = DIRECTION ( 'NONE',  ( -0.3620778797217457656, 0.000000000000000000, -0.9321478471874539151 ) ) ;
#4157 = LINE ( 'NONE', #34516, #27716 ) ;
#4158 = CARTESIAN_POINT ( 'NONE',  ( -17.87149280724919720, 0.000000000000000000, 6.158655315371090566 ) ) ;
#4159 = DIRECTION ( 'NONE',  ( -0.6427681459581293666, -0.7660444431189770143, -0.005002170337467561935 ) ) ;
#4160 = FACE_OUTER_BOUND ( 'NONE', #9057, .T. ) ;
#4161 = CARTESIAN_POINT ( 'NONE',  ( -12.27153996272462955, 0.000000000000000000, 3.078252871230112486 ) ) ;
#4162 = CARTESIAN_POINT ( 'NONE',  ( -12.23851102634202448, -0.1191753592594197858, 11.68427982808754884 ) ) ;
#4163 = ORIENTED_EDGE ( 'NONE', *, *, #10390, .T. ) ;
#4164 = CIRCLE ( 'NONE', #6875, 1.000000000000000000 ) ;
#4165 = DIRECTION ( 'NONE',  ( 0.005002170337468016433, -0.7660444431189770143, -0.6427681459581293666 ) ) ;
#4166 = DIRECTION ( 'NONE',  ( 0.5364919789714477361, 0.6444004775717706579, 0.5449076811759711036 ) ) ;
#4167 = VECTOR ( 'NONE', #11631, 1000.000000000000000 ) ;
#4168 = ORIENTED_EDGE ( 'NONE', *, *, #10986, .F. ) ;
#4169 = DIRECTION ( 'NONE',  ( 0.000000000000000000, -1.000000000000000000, 0.000000000000000000 ) ) ;
#4170 = EDGE_LOOP ( 'NONE', ( #12133, #46183, #26468, #26256 ) ) ;
#4171 = CARTESIAN_POINT ( 'NONE',  ( -7.081010562957787080, 4.806907600676791681, -0.4678686008800659324 ) ) ;
#4172 = VECTOR ( 'NONE', #31383, 1000.000000000000227 ) ;
#4173 = ORIENTED_EDGE ( 'NONE', *, *, #24544, .T. ) ;
#4174 = ADVANCED_FACE ( 'NONE', ( #2581 ), #37807, .F. ) ;
#4175 = VECTOR ( 'NONE', #52788, 999.9999999999998863 ) ;
#4176 = ORIENTED_EDGE ( 'NONE', *, *, #15511, .T. ) ;
#4177 = ORIENTED_EDGE ( 'NONE', *, *, #2682, .F. ) ;
#4178 = VECTOR ( 'NONE', #21601, 999.9999999999998863 ) ;
#4179 = ORIENTED_EDGE ( 'NONE', *, *, #24442, .F. ) ;
#4180 = VECTOR ( 'NONE', #35081, 1000.000000000000227 ) ;
#4181 = EDGE_LOOP ( 'NONE', ( #52548, #34976, #4615, #32027 ) ) ;
#4182 = VERTEX_POINT ( 'NONE', #55967 ) ;
#4183 = CARTESIAN_POINT ( 'NONE',  ( 3.882677180727608146, 0.000000000000000000, 1.710209902397122894 ) ) ;
#4184 = AXIS2_PLACEMENT_3D ( 'NONE', #34248, #3292, #51552 ) ;
#4185 = CARTESIAN_POINT ( 'NONE',  ( -14.62765668987744228, 0.000000000000000000, 7.291895807520449857 ) ) ;
#4186 = FACE_OUTER_BOUND ( 'NONE', #40053, .T. ) ;
#4187 = VECTOR ( 'NONE', #12397, 1000.000000000000227 ) ;
#4188 = EDGE_CURVE ( 'NONE', #37711, #28907, #51425, .T. ) ;
#4189 = AXIS2_PLACEMENT_3D ( 'NONE', #32343, #24085, #16125 ) ;
#4190 = EDGE_LOOP ( 'NONE', ( #16548, #22768, #40044, #24905 ) ) ;
#4191 = DIRECTION ( 'NONE',  ( -0.000000000000000000, -0.000000000000000000, 1.000000000000000000 ) ) ;
#4192 = ORIENTED_EDGE ( 'NONE', *, *, #17150, .F. ) ;
#4193 = DIRECTION ( 'NONE',  ( -0.6427681459581293666, -0.7660444431189770143, -0.005002170337467561935 ) ) ;
#4194 = EDGE_CURVE ( 'NONE', #27982, #52283, #47730, .T. ) ;
#4195 = ORIENTED_EDGE ( 'NONE', *, *, #45589, .T. ) ;
#4196 = EDGE_CURVE ( 'NONE', #30483, #51416, #8839, .T. ) ;
#4197 = VECTOR ( 'NONE', #31560, 1000.000000000000227 ) ;
#4198 = AXIS2_PLACEMENT_3D ( 'NONE', #18957, #12083, #21169 ) ;
#4199 = LINE ( 'NONE', #34005, #19306 ) ;
#4200 = CARTESIAN_POINT ( 'NONE',  ( -12.23851102634202448, -0.1191753592594197858, 11.68427982808754884 ) ) ;
#4201 = DIRECTION ( 'NONE',  ( -0.005002170337468016433, -0.7660444431189770143, 0.6427681459581293666 ) ) ;
#4202 = EDGE_CURVE ( 'NONE', #8687, #29343, #13073, .T. ) ;
#4203 = ORIENTED_EDGE ( 'NONE', *, *, #14094, .F. ) ;
#4204 = CARTESIAN_POINT ( 'NONE',  ( -18.39746900504187010, 0.000000000000000000, 14.03700784672088808 ) ) ;
#4205 = ORIENTED_EDGE ( 'NONE', *, *, #53531, .T. ) ;
#4206 = LINE ( 'NONE', #12447, #34604 ) ;
#4207 = EDGE_CURVE ( 'NONE', #35585, #45114, #34378, .T. ) ;
#4208 = DIRECTION ( 'NONE',  ( 0.005961354470445682716, -0.6427876096865404731, -0.7660212471507180654 ) ) ;
#4209 = EDGE_CURVE ( 'NONE', #13117, #16694, #51682, .T. ) ;
#4210 = VECTOR ( 'NONE', #1275, 999.9999999999998863 ) ;
#4211 = LINE ( 'NONE', #16984, #21498 ) ;
#4212 = DIRECTION ( 'NONE',  ( 0.005002170337468016433, -0.7660444431189770143, -0.6427681459581293666 ) ) ;
#4213 = CARTESIAN_POINT ( 'NONE',  ( 2.072287782118878319, 0.000000000000000000, -2.950529333540147015 ) ) ;
#4214 = DIRECTION ( 'NONE',  ( -0.9999697198139514409, -0.000000000000000000, -0.007781995580013368816 ) ) ;
#4215 = CARTESIAN_POINT ( 'NONE',  ( -19.27115160478301803, 0.000000000000000000, 6.886426986582589116 ) ) ;
#4216 = DIRECTION ( 'NONE',  ( 0.000000000000000000, -1.000000000000000000, 0.000000000000000000 ) ) ;
#4217 = EDGE_LOOP ( 'NONE', ( #48865, #43698, #34137, #17569 ) ) ;
#4218 = FACE_OUTER_BOUND ( 'NONE', #10818, .T. ) ;
#4219 = VERTEX_POINT ( 'NONE', #34636 ) ;
#4220 = VECTOR ( 'NONE', #583, 1000.000000000000227 ) ;
#4221 = EDGE_CURVE ( 'NONE', #16268, #24035, #38920, .T. ) ;
#4222 = CARTESIAN_POINT ( 'NONE',  ( -21.06965149344186372, 20.49370688441071664, -4.356725136697556344 ) ) ;
#4223 = DIRECTION ( 'NONE',  ( 0.7660212471507180654, -0.6427876096865404731, 0.005961354470445141482 ) ) ;
#4225 = CARTESIAN_POINT ( 'NONE',  ( 2.072287782118878319, 0.000000000000000000, -2.950529333540147015 ) ) ;
#4224 = AXIS2_PLACEMENT_3D ( 'NONE', #3934, #11881, #35189 ) ;
#4226 = CARTESIAN_POINT ( 'NONE',  ( -10.00813838035478298, 0.000000000000000000, 10.77830692922518452 ) ) ;
#4227 = DIRECTION ( 'NONE',  ( -0.5449076811759708816, 0.6444004775717707689, 0.5364919789714475140 ) ) ;
#4228 = CARTESIAN_POINT ( 'NONE',  ( -6.007464458508009919, -5.767005180143939036, -0.8848703656275269669 ) ) ;
#4229 = ADVANCED_FACE ( 'NONE', ( #30106 ), #47422, .F. ) ;
#4230 = VECTOR ( 'NONE', #42195, 1000.000000000000227 ) ;
#4231 = FACE_OUTER_BOUND ( 'NONE', #13736, .T. ) ;
#4232 = ORIENTED_EDGE ( 'NONE', *, *, #27277, .T. ) ;
#4233 = CARTESIAN_POINT ( 'NONE',  ( -19.63965433603666710, 19.58726532061008641, 4.312915315567922292 ) ) ;
#4234 = LINE ( 'NONE', #25243, #40348 ) ;
#4235 = PLANE ( 'NONE',  #11878 ) ;
#4236 = VECTOR ( 'NONE', #2238, 999.9999999999998863 ) ;
#4237 = VECTOR ( 'NONE', #26254, 1000.000000000000000 ) ;
#4238 = CARTESIAN_POINT ( 'NONE',  ( -61.10213307005876970, 6.758246409053502823, -3.000000000000006217 ) ) ;
#4239 = FACE_OUTER_BOUND ( 'NONE', #21147, .T. ) ;
#4240 = LINE ( 'NONE', #46825, #15051 ) ;
#4241 = PLANE ( 'NONE',  #3875 ) ;
#4242 = ORIENTED_EDGE ( 'NONE', *, *, #45670, .T. ) ;
#4243 = VECTOR ( 'NONE', #24341, 1000.000000000000227 ) ;
#4245 = CARTESIAN_POINT ( 'NONE',  ( -11.62547109734172501, 0.000000000000000000, 5.468599160955688987 ) ) ;
#4244 = AXIS2_PLACEMENT_3D ( 'NONE', #3773, #42968, #17395 ) ;
#4246 = CARTESIAN_POINT ( 'NONE',  ( -66.78407322188951412, -9.486793844097082484, -0.6948190221874483985 ) ) ;
#4247 = ORIENTED_EDGE ( 'NONE', *, *, #33800, .T. ) ;
#4248 = ORIENTED_EDGE ( 'NONE', *, *, #8217, .F. ) ;
#4249 = CARTESIAN_POINT ( 'NONE',  ( -19.22961988024793101, -0.1191753592594177458, 14.39986392600063603 ) ) ;
#4250 = ORIENTED_EDGE ( 'NONE', *, *, #53798, .F. ) ;
#4251 = EDGE_CURVE ( 'NONE', #38604, #17725, #8243, .T. ) ;
#4252 = AXIS2_PLACEMENT_3D ( 'NONE', #32134, #53987, #23599 ) ;
#4253 = VERTEX_POINT ( 'NONE', #43195 ) ;
#4254 = ORIENTED_EDGE ( 'NONE', *, *, #35222, .T. ) ;
#4255 = ORIENTED_EDGE ( 'NONE', *, *, #23423, .F. ) ;
#4256 = LINE ( 'NONE', #3402, #9402 ) ;
#4257 = ORIENTED_EDGE ( 'NONE', *, *, #55337, .F. ) ;
#4258 = CARTESIAN_POINT ( 'NONE',  ( -17.41850097848045920, 3.362543313726510164, 3.340586309761012451 ) ) ;
#4259 = FACE_OUTER_BOUND ( 'NONE', #15402, .T. ) ;
#4260 = VECTOR ( 'NONE', #42754, 1000.000000000000227 ) ;
#4261 = EDGE_LOOP ( 'NONE', ( #25981, #22306, #30077, #5804 ) ) ;
#4262 = ORIENTED_EDGE ( 'NONE', *, *, #26618, .T. ) ;
#4263 = EDGE_CURVE ( 'NONE', #44057, #46834, #3986, .T. ) ;
#4264 = VECTOR ( 'NONE', #7782, 1000.000000000000227 ) ;
#4265 = CARTESIAN_POINT ( 'NONE',  ( -19.60990026154428278, 0.000000000000000000, 4.498472333781370125 ) ) ;
#4266 = ORIENTED_EDGE ( 'NONE', *, *, #54011, .F. ) ;
#4267 = PLANE ( 'NONE',  #15519 ) ;
#4268 = PLANE ( 'NONE',  #3240 ) ;
#4269 = VERTEX_POINT ( 'NONE', #33439 ) ;
#4270 = DIRECTION ( 'NONE',  ( 0.6427681459581294776, -0.7660444431189769032, 0.005002170337467562802 ) ) ;
#4271 = ORIENTED_EDGE ( 'NONE', *, *, #6842, .F. ) ;
#4272 = VECTOR ( 'NONE', #820, 999.9999999999998863 ) ;
#4273 = DIRECTION ( 'NONE',  ( 0.000000000000000000, -0.000000000000000000, -1.000000000000000000 ) ) ;
#4274 = EDGE_CURVE ( 'NONE', #16523, #563, #8992, .T. ) ;
#4275 = EDGE_CURVE ( 'NONE', #8639, #947, #46467, .T. ) ;
#4276 = CARTESIAN_POINT ( 'NONE',  ( -16.17376003385353300, -4.889348428825664783, 3.007762964104071735 ) ) ;
#4277 = VECTOR ( 'NONE', #36690, 999.9999999999998863 ) ;
#4278 = EDGE_LOOP ( 'NONE', ( #3722, #27860, #49278, #43043 ) ) ;
#4279 = LINE ( 'NONE', #51937, #10421 ) ;
#4280 = DIRECTION ( 'NONE',  ( -0.005002170337468016433, -0.7660444431189770143, 0.6427681459581293666 ) ) ;
#4281 = CARTESIAN_POINT ( 'NONE',  ( -17.69604769044466863, 0.000000000000000000, 9.314683284511998451 ) ) ;
#4282 = LINE ( 'NONE', #52516, #43719 ) ;
#4283 = ORIENTED_EDGE ( 'NONE', *, *, #8142, .T. ) ;
#4284 = EDGE_CURVE ( 'NONE', #6902, #6537, #34290, .T. ) ;
#4285 = CARTESIAN_POINT ( 'NONE',  ( 2.072287782118878319, 0.000000000000000000, -2.950529333540147015 ) ) ;
#4286 = DIRECTION ( 'NONE',  ( -0.7660212471507179544, -0.6427876096865405842, -0.005961354470445141482 ) ) ;
#4287 = CARTESIAN_POINT ( 'NONE',  ( -29.86197018149027116, 0.000000000000000000, 8.281335066757780083 ) ) ;
#4288 = DIRECTION ( 'NONE',  ( 0.000000000000000000, -1.000000000000000000, 0.000000000000000000 ) ) ;
#4289 = LINE ( 'NONE', #17308, #27773 ) ;
#4290 = CARTESIAN_POINT ( 'NONE',  ( -15.38203175034444747, 4.819660872929013351, 2.503062823780374924 ) ) ;
#4291 = PLANE ( 'NONE',  #47915 ) ;
#4292 = EDGE_CURVE ( 'NONE', #35264, #24902, #50743, .T. ) ;
#4293 = CARTESIAN_POINT ( 'NONE',  ( -16.50057454476819885, 0.000000000000000000, 9.123980676737234674 ) ) ;
#4294 = CARTESIAN_POINT ( 'NONE',  ( -9.808144436391993182, 0.000000000000000000, 10.77986332834118777 ) ) ;
#4295 = EDGE_LOOP ( 'NONE', ( #23358, #5510, #1944, #12764 ) ) ;
#4296 = CARTESIAN_POINT ( 'NONE',  ( -18.29747203306047609, -0.1191753592594177458, 14.03778604627889059 ) ) ;
#4297 = ORIENTED_EDGE ( 'NONE', *, *, #7814, .F. ) ;
#4298 = FACE_OUTER_BOUND ( 'NONE', #19361, .T. ) ;
#4299 = LINE ( 'NONE', #14225, #3729 ) ;
#4300 = AXIS2_PLACEMENT_3D ( 'NONE', #38438, #30777, #26785 ) ;
#4301 = FACE_OUTER_BOUND ( 'NONE', #19185, .T. ) ;
#4302 = PLANE ( 'NONE',  #36910 ) ;
#4303 = CARTESIAN_POINT ( 'NONE',  ( -25.20278734466900517, 0.000000000000000000, 6.670939612111840944 ) ) ;
#4304 = ORIENTED_EDGE ( 'NONE', *, *, #17856, .T. ) ;
#4305 = VECTOR ( 'NONE', #12404, 1000.000000000000227 ) ;
#4306 = ORIENTED_EDGE ( 'NONE', *, *, #29314, .T. ) ;
#4307 = CARTESIAN_POINT ( 'NONE',  ( -17.73140113748535285, 0.000000000000000000, 13.85752530597602039 ) ) ;
#4308 = DIRECTION ( 'NONE',  ( -0.6427681459581293666, -0.7660444431189770143, -0.005002170337467561935 ) ) ;
#4309 = VERTEX_POINT ( 'NONE', #7899 ) ;
#4310 = ADVANCED_FACE ( 'NONE', ( #25211 ), #7049, .F. ) ;
#4311 = PLANE ( 'NONE',  #25684 ) ;
#4312 = VECTOR ( 'NONE', #39628, 1000.000000000000114 ) ;
#4313 = EDGE_LOOP ( 'NONE', ( #49019, #12159, #54261, #55365, #15419 ) ) ;
#4314 = PLANE ( 'NONE',  #11347 ) ;
#4315 = ADVANCED_FACE ( 'NONE', ( #45941 ), #16373, .F. ) ;
#4316 = ORIENTED_EDGE ( 'NONE', *, *, #45969, .F. ) ;
#4317 = DIRECTION ( 'NONE',  ( -0.9999697198139514409, -0.000000000000000000, -0.007781995580013368816 ) ) ;
#4318 = ORIENTED_EDGE ( 'NONE', *, *, #4451, .T. ) ;
#4319 = ORIENTED_EDGE ( 'NONE', *, *, #529, .T. ) ;
#4320 = ORIENTED_EDGE ( 'NONE', *, *, #31957, .F. ) ;
#4321 = ADVANCED_FACE ( 'NONE', ( #29155 ), #47055, .F. ) ;
#4322 = CARTESIAN_POINT ( 'NONE',  ( -15.07660566480283748, 0.000000000000000000, 5.272415620168643180 ) ) ;
#4323 = DIRECTION ( 'NONE',  ( 0.005002170337468016433, -0.7660444431189770143, -0.6427681459581293666 ) ) ;
#4324 = CARTESIAN_POINT ( 'NONE',  ( -12.13851405436063047, 0.000000000000000000, 11.68505802764555135 ) ) ;
#4325 = EDGE_CURVE ( 'NONE', #43270, #32747, #21206, .T. ) ;
#4326 = EDGE_CURVE ( 'NONE', #33148, #46628, #33699, .T. ) ;
#4327 = EDGE_CURVE ( 'NONE', #21477, #9006, #28899, .T. ) ;
#4328 = CARTESIAN_POINT ( 'NONE',  ( 2.072287782118878319, 0.000000000000000000, -2.950529333540147015 ) ) ;
#4329 = EDGE_LOOP ( 'NONE', ( #27371, #12486, #40200, #8277 ) ) ;
#4330 = ORIENTED_EDGE ( 'NONE', *, *, #42708, .T. ) ;
#4331 = ORIENTED_EDGE ( 'NONE', *, *, #13855, .T. ) ;
#4332 = PLANE ( 'NONE',  #46684 ) ;
#4333 = ORIENTED_EDGE ( 'NONE', *, *, #12165, .T. ) ;
#4334 = PLANE ( 'NONE',  #11198 ) ;
#4335 = EDGE_LOOP ( 'NONE', ( #43770, #37186, #35086, #8647 ) ) ;
#4336 = DIRECTION ( 'NONE',  ( -0.005961354470445682716, -0.6427876096865404731, 0.7660212471507180654 ) ) ;
#4337 = CARTESIAN_POINT ( 'NONE',  ( -11.36370219796871339, 0.000000000000000000, 5.839968376865459554 ) ) ;
#4338 = ORIENTED_EDGE ( 'NONE', *, *, #6358, .T. ) ;
#4339 = PLANE ( 'NONE',  #51266 ) ;
#4340 = ADVANCED_FACE ( 'NONE', ( #7297 ), #25467, .F. ) ;
#4341 = ORIENTED_EDGE ( 'NONE', *, *, #47393, .T. ) ;
#4342 = EDGE_CURVE ( 'NONE', #18162, #17751, #2741, .T. ) ;
#4343 = VECTOR ( 'NONE', #9043, 1000.000000000000114 ) ;
#4344 = CARTESIAN_POINT ( 'NONE',  ( -11.40636015113596180, 0.000000000000000000, 11.32142374880780089 ) ) ;
#4345 = ORIENTED_EDGE ( 'NONE', *, *, #55262, .F. ) ;
#4346 = FACE_OUTER_BOUND ( 'NONE', #23649, .T. ) ;
#4347 = FACE_OUTER_BOUND ( 'NONE', #48451, .T. ) ;
#4348 = EDGE_CURVE ( 'NONE', #42292, #36024, #33165, .T. ) ;
#4349 = DIRECTION ( 'NONE',  ( -0.005002170337468016433, -0.7660444431189770143, 0.6427681459581293666 ) ) ;
#4350 = ORIENTED_EDGE ( 'NONE', *, *, #40743, .T. ) ;
#4351 = LINE ( 'NONE', #25929, #40163 ) ;
#4352 = ADVANCED_FACE ( 'NONE', ( #41928 ), #3030, .F. ) ;
#4353 = VECTOR ( 'NONE', #8603, 1000.000000000000114 ) ;
#4354 = CARTESIAN_POINT ( 'NONE',  ( -20.72814514249575168, 20.40220053346460460, -4.343046601173932153 ) ) ;
#4355 = PLANE ( 'NONE',  #54810 ) ;
#4356 = DIRECTION ( 'NONE',  ( 0.5449076811759707706, 0.6444004775717708799, -0.5364919789714476250 ) ) ;
#4357 = LINE ( 'NONE', #21665, #19492 ) ;
#4358 = ADVANCED_FACE ( 'NONE', ( #22553 ), #48676, .F. ) ;
#4359 = CARTESIAN_POINT ( 'NONE',  ( -15.82732154344847864, 0.000000000000000000, 8.021223877847955208 ) ) ;
#4360 = EDGE_LOOP ( 'NONE', ( #51718, #33979, #28900, #15955 ) ) ;
#4361 = CARTESIAN_POINT ( 'NONE',  ( -10.70350180978612542, 0.000000000000000000, 6.414444334970025530 ) ) ;
#4362 = PLANE ( 'NONE',  #42202 ) ;
#4363 = DIRECTION ( 'NONE',  ( 0.007781995580012663651, 0.000000000000000000, -0.9999697198139515519 ) ) ;
#4364 = ORIENTED_EDGE ( 'NONE', *, *, #34202, .F. ) ;
#4365 = CARTESIAN_POINT ( 'NONE',  ( -15.45771171113622167, -0.1191753592594177180, 7.385439155523823906 ) ) ;
#4366 = CARTESIAN_POINT ( 'NONE',  ( -17.73140113748535285, 0.000000000000000000, 13.85752530597602039 ) ) ;
#4367 = ORIENTED_EDGE ( 'NONE', *, *, #16453, .F. ) ;
#4368 = FACE_OUTER_BOUND ( 'NONE', #16584, .T. ) ;
#4369 = DIRECTION ( 'NONE',  ( -0.6427681459581293666, -0.7660444431189770143, -0.005002170337467561935 ) ) ;
#4370 = CARTESIAN_POINT ( 'NONE',  ( -14.93495759592298988, 0.000000000000000000, 12.77129166681078409 ) ) ;
#4371 = CARTESIAN_POINT ( 'NONE',  ( -67.21057658696469161, 2.000000000012947865, 0.7018102913198165371 ) ) ;
#4372 = ORIENTED_EDGE ( 'NONE', *, *, #55975, .T. ) ;
#4373 = ORIENTED_EDGE ( 'NONE', *, *, #548, .F. ) ;
#4374 = LINE ( 'NONE', #9755, #42106 ) ;
#4375 = CARTESIAN_POINT ( 'NONE',  ( -10.19707176475507815, 0.000000000000000000, 1.047730457166543783 ) ) ;
#4376 = CARTESIAN_POINT ( 'NONE',  ( -13.27065584551087163, 0.000000000000000000, 12.04557950825129176 ) ) ;
#4377 = DIRECTION ( 'NONE',  ( 0.6427681459581294776, -0.7660444431189769032, 0.005002170337467562802 ) ) ;
#4378 = DIRECTION ( 'NONE',  ( 0.5364919789714477361, 0.6444004775717706579, 0.5449076811759711036 ) ) ;
#4379 = PLANE ( 'NONE',  #43056 ) ;
#4380 = ORIENTED_EDGE ( 'NONE', *, *, #5523, .T. ) ;
#4381 = DIRECTION ( 'NONE',  ( -0.6427681459581293666, -0.7660444431189770143, -0.005002170337467561935 ) ) ;
#4382 = PLANE ( 'NONE',  #4300 ) ;
#4383 = EDGE_LOOP ( 'NONE', ( #29653, #51259, #50694, #43168 ) ) ;
#4384 = LINE ( 'NONE', #26494, #14761 ) ;
#4385 = DIRECTION ( 'NONE',  ( -0.7660212471507179544, -0.6427876096865405842, -0.005961354470445141482 ) ) ;
#4386 = CARTESIAN_POINT ( 'NONE',  ( -13.63673279712320507, -0.1191753592594197858, 12.22739664767016521 ) ) ;
#4387 = EDGE_CURVE ( 'NONE', #36809, #37046, #1781, .T. ) ;
#4388 = EDGE_CURVE ( 'NONE', #36400, #44385, #942, .T. ) ;
#4389 = EDGE_LOOP ( 'NONE', ( #6909, #4179, #56103, #38966 ) ) ;
#4390 = AXIS2_PLACEMENT_3D ( 'NONE', #31082, #40741, #22845 ) ;
#4391 = CYLINDRICAL_SURFACE ( 'NONE', #27582, 2.125000000000000000 ) ;
#4392 = ORIENTED_EDGE ( 'NONE', *, *, #44249, .T. ) ;
#4393 = EDGE_CURVE ( 'NONE', #1220, #41647, #35599, .T. ) ;
#4394 = ORIENTED_EDGE ( 'NONE', *, *, #28199, .T. ) ;
#4395 = EDGE_LOOP ( 'NONE', ( #35165, #27222, #49716, #38811 ) ) ;
#4396 = EDGE_LOOP ( 'NONE', ( #3514, #52501, #14243, #7609 ) ) ;
#4397 = FACE_OUTER_BOUND ( 'NONE', #3040, .T. ) ;
#4398 = ORIENTED_EDGE ( 'NONE', *, *, #1711, .T. ) ;
#4399 = CARTESIAN_POINT ( 'NONE',  ( -15.36885972723471561, 22.05300973765551475, -3.958603441819915414 ) ) ;
#4400 = ORIENTED_EDGE ( 'NONE', *, *, #23595, .F. ) ;
#4401 = CARTESIAN_POINT ( 'NONE',  ( -29.86274838104827367, -0.1191753592594197858, 8.381332038739175871 ) ) ;
#4402 = VERTEX_POINT ( 'NONE', #44395 ) ;
#4403 = DIRECTION ( 'NONE',  ( 0.7660212471507180654, -0.6427876096865404731, 0.005961354470445141482 ) ) ;
#4404 = ORIENTED_EDGE ( 'NONE', *, *, #89, .F. ) ;
#4405 = ADVANCED_FACE ( 'NONE', ( #36429 ), #18857, .F. ) ;
#4406 = CARTESIAN_POINT ( 'NONE',  ( -4.592488342126416434, 4.500757451777032792, 5.002252009306281444 ) ) ;
#4407 = B_SPLINE_CURVE_WITH_KNOTS ( 'NONE', 3,
 ( #45023, #27980, #32239, #53517, #40486, #10672 ),
 .UNSPECIFIED., .F., .F.,
 ( 4, 2, 4 ),
 ( 0.05059699584195882782, 0.5000000368888000146, 0.9494030779356412708 ),
 .UNSPECIFIED. ) ;
#4408 = CARTESIAN_POINT ( 'NONE',  ( -14.94916102560700821, 0.000000000000000000, 2.688082935172642962 ) ) ;
#4409 = FACE_OUTER_BOUND ( 'NONE', #32469, .T. ) ;
#4410 = PLANE ( 'NONE',  #29607 ) ;
#4411 = DIRECTION ( 'NONE',  ( 0.7660212471507180654, -0.6427876096865404731, 0.005961354470445141482 ) ) ;
#4412 = ORIENTED_EDGE ( 'NONE', *, *, #47711, .T. ) ;
#4414 = ORIENTED_EDGE ( 'NONE', *, *, #32772, .T. ) ;
#4413 = ADVANCED_FACE ( 'NONE', ( #53480 ), #53225, .F. ) ;
#4415 = CARTESIAN_POINT ( 'NONE',  ( -13.49994535134848661, 0.000000000000000000, 7.500677974135260939 ) ) ;
#4416 = DIRECTION ( 'NONE',  ( 0.7660212471507180654, -0.6427876096865404731, 0.005961354470445141482 ) ) ;
#4417 = ADVANCED_FACE ( 'NONE', ( #14580 ), #34546, .F. ) ;
#4418 = LINE ( 'NONE', #47009, #16994 ) ;
#4419 = CARTESIAN_POINT ( 'NONE',  ( -11.40636015113596180, 0.000000000000000000, 11.32142374880780089 ) ) ;
#4420 = ADVANCED_FACE ( 'NONE', ( #22813 ), #40132, .F. ) ;
#4421 = CARTESIAN_POINT ( 'NONE',  ( -1.086233639165236964, 0.000000000000000000, -2.796443541562362078 ) ) ;
#4422 = FACE_OUTER_BOUND ( 'NONE', #25383, .T. ) ;
#4423 = ORIENTED_EDGE ( 'NONE', *, *, #319, .F. ) ;
#4424 = CARTESIAN_POINT ( 'NONE',  ( -19.21524870871409618, -0.1941918491731548790, 4.464488790411954788 ) ) ;
#4425 = EDGE_CURVE ( 'NONE', #48142, #48104, #31638, .T. ) ;
#4426 = LINE ( 'NONE', #51557, #26778 ) ;
#4427 = ORIENTED_EDGE ( 'NONE', *, *, #10218, .T. ) ;
#4428 = VECTOR ( 'NONE', #18508, 1000.000000000000227 ) ;
#4429 = CARTESIAN_POINT ( 'NONE',  ( -16.02156738040070394, 0.000000000000000000, 7.281048072216421474 ) ) ;
#4430 = CARTESIAN_POINT ( 'NONE',  ( -13.47252247068494135, 0.000000000000000000, 3.976896700852591948 ) ) ;
#4431 = ADVANCED_FACE ( 'NONE', ( #27347 ), #26806, .F. ) ;
#4432 = PLANE ( 'NONE',  #34097 ) ;
#4433 = CARTESIAN_POINT ( 'NONE',  ( -27.99767448711536133, 0.000000000000000000, 7.557179307314289218 ) ) ;
#4434 = CARTESIAN_POINT ( 'NONE',  ( -21.47263955680318404, 0.000000000000000000, 5.022634149262071190 ) ) ;
#4435 = ORIENTED_EDGE ( 'NONE', *, *, #37563, .F. ) ;
#4436 = ORIENTED_EDGE ( 'NONE', *, *, #42302, .F. ) ;
#4437 = DIRECTION ( 'NONE',  ( 0.000000000000000000, -1.000000000000000000, 0.000000000000000000 ) ) ;
#4438 = DIRECTION ( 'NONE',  ( 0.005002170337468016433, -0.7660444431189770143, -0.6427681459581293666 ) ) ;
#4439 = PLANE ( 'NONE',  #19732 ) ;
#4440 = LINE ( 'NONE', #22322, #25525 ) ;
#4441 = LINE ( 'NONE', #43881, #55690 ) ;
#4442 = DIRECTION ( 'NONE',  ( -0.5449076811759708816, 0.6444004775717707689, 0.5364919789714475140 ) ) ;
#4443 = DIRECTION ( 'NONE',  ( 0.7660212471507180654, -0.6427876096865404731, 0.005961354470445141482 ) ) ;
#4444 = ORIENTED_EDGE ( 'NONE', *, *, #29952, .T. ) ;
#4445 = DIRECTION ( 'NONE',  ( 0.9999697198139515519, 0.000000000000000000, 0.007781995580013368816 ) ) ;
#4446 = CARTESIAN_POINT ( 'NONE',  ( 2.072287782118878319, 0.000000000000000000, -2.950529333540147015 ) ) ;
#4447 = ORIENTED_EDGE ( 'NONE', *, *, #27977, .T. ) ;
#4448 = DIRECTION ( 'NONE',  ( -0.005961354470445682716, -0.6427876096865404731, 0.7660212471507180654 ) ) ;
#4449 = VERTEX_POINT ( 'NONE', #10326 ) ;
#4450 = FACE_OUTER_BOUND ( 'NONE', #17507, .T. ) ;
#4451 = EDGE_CURVE ( 'NONE', #24292, #14805, #51860, .T. ) ;
#4452 = ORIENTED_EDGE ( 'NONE', *, *, #23447, .F. ) ;
#4453 = ORIENTED_EDGE ( 'NONE', *, *, #38327, .T. ) ;
#4454 = EDGE_CURVE ( 'NONE', #51315, #45422, #36769, .T. ) ;
#4455 = B_SPLINE_CURVE_WITH_KNOTS ( 'NONE', 3,
 ( #43486, #1450, #40349, #5432, #35821, #4867 ),
 .UNSPECIFIED., .F., .F.,
 ( 4, 2, 4 ),
 ( 1.387778780781430114E-17, 0.0009531277170912127008, 0.001906255434182411524 ),
 .UNSPECIFIED. ) ;
#4456 = EDGE_CURVE ( 'NONE', #45853, #47084, #13729, .T. ) ;
#4457 = EDGE_LOOP ( 'NONE', ( #9913, #22248, #14318, #18600 ) ) ;
#4458 = EDGE_LOOP ( 'NONE', ( #4807, #41929, #53330, #20915 ) ) ;
#4459 = ORIENTED_EDGE ( 'NONE', *, *, #37806, .T. ) ;
#4460 = ORIENTED_EDGE ( 'NONE', *, *, #9376, .F. ) ;
#4461 = DIRECTION ( 'NONE',  ( 0.007781995580012663651, 0.000000000000000000, -0.9999697198139515519 ) ) ;
#4462 = PLANE ( 'NONE',  #27492 ) ;
#4463 = FACE_OUTER_BOUND ( 'NONE', #9263, .T. ) ;
#4464 = EDGE_LOOP ( 'NONE', ( #14186, #33756, #40060, #26649 ) ) ;
#4465 = LINE ( 'NONE', #30601, #33098 ) ;
#4466 = VERTEX_POINT ( 'NONE', #38830 ) ;
#4467 = ORIENTED_EDGE ( 'NONE', *, *, #6960, .T. ) ;
#4468 = EDGE_CURVE ( 'NONE', #52808, #46492, #1223, .T. ) ;
#4469 = CARTESIAN_POINT ( 'NONE',  ( -21.47341775636118655, -0.1191753592594197858, 5.122631121243466090 ) ) ;
#4470 = PLANE ( 'NONE',  #18701 ) ;
#4471 = ORIENTED_EDGE ( 'NONE', *, *, #8942, .T. ) ;
#4472 = DIRECTION ( 'NONE',  ( 0.005002170337468016433, -0.7660444431189770143, -0.6427681459581293666 ) ) ;
#4473 = ORIENTED_EDGE ( 'NONE', *, *, #7377, .T. ) ;
#4474 = DIRECTION ( 'NONE',  ( 0.007781995580012663651, -3.146120232559066537E-19, -0.9999697198139514409 ) ) ;
#4475 = CARTESIAN_POINT ( 'NONE',  ( -24.26908309836554878, 0.000000000000000000, 6.108867788427308376 ) ) ;
#4476 = ADVANCED_FACE ( 'NONE', ( #48370 ), #9480, .T. ) ;
#4477 = CARTESIAN_POINT ( 'NONE',  ( -15.60102546347950536, 0.000000000000000000, 12.95077420755565356 ) ) ;
#4478 = PLANE ( 'NONE',  #473 ) ;
#4479 = CARTESIAN_POINT ( 'NONE',  ( -27.99845268667336384, -0.1191753592594197858, 7.657176279295684118 ) ) ;
#4480 = EDGE_CURVE ( 'NONE', #24312, #13470, #41539, .T. ) ;
#4481 = CARTESIAN_POINT ( 'NONE',  ( -19.24620501330758060, -0.1191753592594167188, 8.094620364256195799 ) ) ;
#4482 = DIRECTION ( 'NONE',  ( -0.9999697198139514409, -0.000000000000000000, -0.007781995580013368816 ) ) ;
#4483 = CARTESIAN_POINT ( 'NONE',  ( -68.45530293218364193, -11.55776342273651380, -6.702751532743291385 ) ) ;
#4484 = ORIENTED_EDGE ( 'NONE', *, *, #1904, .T. ) ;
#4485 = CARTESIAN_POINT ( 'NONE',  ( -55.79576865894325977, 6.773981352271770007, -1.647106450292881163 ) ) ;
#4486 = CARTESIAN_POINT ( 'NONE',  ( -11.37519841198984416, 0.000000000000000000, 7.317207189896516972 ) ) ;
#4487 = CARTESIAN_POINT ( 'NONE',  ( -19.77061338776520216, 21.24370688441071664, -4.657437592157546824 ) ) ;
#4488 = FACE_OUTER_BOUND ( 'NONE', #32078, .T. ) ;
#4489 = EDGE_CURVE ( 'NONE', #25204, #52744, #41793, .T. ) ;
#4490 = CARTESIAN_POINT ( 'NONE',  ( -19.70957090889394081, 19.54689896845012598, -4.317539206161682408 ) ) ;
#4491 = CARTESIAN_POINT ( 'NONE',  ( -13.01231602646514141, 0.000000000000000000, 4.549816259841156452 ) ) ;
#4492 = DIRECTION ( 'NONE',  ( 0.5364919789714477361, 0.6444004775717706579, 0.5449076811759711036 ) ) ;
#4493 = CARTESIAN_POINT ( 'NONE',  ( -16.29064078590028330, 0.000000000000000000, 7.848292206784967640 ) ) ;
#4494 = ITEM_DEFINED_TRANSFORMATION ( 'NONE', 'NONE', #33510,  #2610 ) ;
#4495 = VERTEX_POINT ( 'NONE', #37008 ) ;
#4496 = CARTESIAN_POINT ( 'NONE',  ( -19.52344721837093999, 19.65435753127615470, 4.305181340342182139 ) ) ;
#4497 = DIRECTION ( 'NONE',  ( 0.007781995580012663651, -3.146120232559066537E-19, -0.9999697198139514409 ) ) ;
#4498 = CARTESIAN_POINT ( 'NONE',  ( -16.81190032086591302, 0.000000000000000000, 3.212244750653343583 ) ) ;
#4499 = EDGE_CURVE ( 'NONE', #19187, #9690, #14862, .T. ) ;
#4500 = LINE ( 'NONE', #39716, #29131 ) ;
#4501 = LINE ( 'NONE', #17008, #4865 ) ;
#4502 = CARTESIAN_POINT ( 'NONE',  ( -13.73672976910459909, 0.000000000000000000, 12.22661844811216270 ) ) ;
#4503 = ADVANCED_FACE ( 'NONE', ( #46326 ), #24477, .F. ) ;
#4504 = DIRECTION ( 'NONE',  ( 0.9999697198139515519, 0.000000000000000000, 0.007781995580013368816 ) ) ;
#4505 = CARTESIAN_POINT ( 'NONE',  ( 2.072287782118878319, 0.000000000000000000, -2.950529333540147015 ) ) ;
#4506 = CARTESIAN_POINT ( 'NONE',  ( -67.70222436837769919, -9.592143523249529125, 4.605078063924984200 ) ) ;
#4507 = VERTEX_POINT ( 'NONE', #32476 ) ;
#4508 = CARTESIAN_POINT ( 'NONE',  ( -13.33515596948987714, 1.257817950434005461, 4.125442103548757622 ) ) ;
#4509 = ADVANCED_FACE ( 'NONE', ( #45788 ), #37263, .F. ) ;
#4510 = ORIENTED_EDGE ( 'NONE', *, *, #12597, .F. ) ;
#4511 = EDGE_CURVE ( 'NONE', #5292, #43677, #38586, .T. ) ;
#4512 = EDGE_CURVE ( 'NONE', #10554, #46790, #50618, .T. ) ;
#4513 = ORIENTED_EDGE ( 'NONE', *, *, #1785, .F. ) ;
#4514 = ORIENTED_EDGE ( 'NONE', *, *, #2638, .T. ) ;
#4515 = ORIENTED_EDGE ( 'NONE', *, *, #24498, .T. ) ;
#4516 = ORIENTED_EDGE ( 'NONE', *, *, #46167, .F. ) ;
#4517 = FACE_OUTER_BOUND ( 'NONE', #37004, .T. ) ;
#4518 = CARTESIAN_POINT ( 'NONE',  ( -16.81345671998191449, 0.000000000000000000, 3.412238694616132495 ) ) ;
#4519 = EDGE_CURVE ( 'NONE', #8314, #46588, #37548, .T. ) ;
#4520 = EDGE_CURVE ( 'NONE', #5827, #38038, #10873, .T. ) ;
#4521 = ORIENTED_EDGE ( 'NONE', *, *, #53652, .F. ) ;
#4522 = EDGE_CURVE ( 'NONE', #53284, #31756, #7439, .T. ) ;
#4523 = DIRECTION ( 'NONE',  ( -0.6427681459581293666, -0.7660444431189770143, -0.005002170337467561935 ) ) ;
#4524 = EDGE_LOOP ( 'NONE', ( #35276, #1445, #55737, #37988 ) ) ;
#4525 = DIRECTION ( 'NONE',  ( 0.000000000000000000, -0.000000000000000000, -1.000000000000000000 ) ) ;
#4526 = DIRECTION ( 'NONE',  ( -0.9999697198139514409, -0.000000000000000000, -0.007781995580013368816 ) ) ;
#4527 = ORIENTED_EDGE ( 'NONE', *, *, #22969, .F. ) ;
#4528 = FACE_OUTER_BOUND ( 'NONE', #15448, .T. ) ;
#4529 = ORIENTED_EDGE ( 'NONE', *, *, #8617, .F. ) ;
#4530 = DIRECTION ( 'NONE',  ( -0.6427681459581293666, -0.7660444431189770143, -0.005002170337467561935 ) ) ;
#4531 = DIRECTION ( 'NONE',  ( 0.007781995580012662783, 0.000000000000000000, -0.9999697198139514409 ) ) ;
#4532 = EDGE_LOOP ( 'NONE', ( #16575, #23388, #20917, #37832 ) ) ;
#4533 = DIRECTION ( 'NONE',  ( 0.007781995580012663651, -3.146120232559066537E-19, -0.9999697198139514409 ) ) ;
#4534 = CARTESIAN_POINT ( 'NONE',  ( -27.06708303904391144, 0.000000000000000000, 7.395095371555332697 ) ) ;
#4535 = DIRECTION ( 'NONE',  ( -0.9321478471874540261, 0.000000000000000000, 0.3620778797217457656 ) ) ;
#4536 = EDGE_LOOP ( 'NONE', ( #47272, #38177, #28158, #5649 ) ) ;
#4537 = CARTESIAN_POINT ( 'NONE',  ( -62.23823698199103660, 6.658783344088820222, -3.000000000000000000 ) ) ;
#4538 = VERTEX_POINT ( 'NONE', #6614 ) ;
#4539 = LINE ( 'NONE', #47413, #52807 ) ;
#4540 = DIRECTION ( 'NONE',  ( -0.005961354470445682716, -0.6427876096865404731, 0.7660212471507180654 ) ) ;
#4541 = CARTESIAN_POINT ( 'NONE',  ( -27.99767448711536133, 0.000000000000000000, 7.557179307314289218 ) ) ;
#4542 = PLANE ( 'NONE',  #12371 ) ;
#4543 = EDGE_CURVE ( 'NONE', #19187, #51242, #19685, .T. ) ;
#4544 = LINE ( 'NONE', #29839, #39521 ) ;
#4545 = DIRECTION ( 'NONE',  ( 0.8531650599175527594, 0.4028455766673922356, -0.3313982828793700652 ) ) ;
#4546 = PLANE ( 'NONE',  #25258 ) ;
#4547 = CARTESIAN_POINT ( 'NONE',  ( -13.25978161800689747, 1.743523803501506375, 1.776853678323026431 ) ) ;
#4548 = CARTESIAN_POINT ( 'NONE',  ( -10.74029228357944987, 0.000000000000000000, 11.14194120806293320 ) ) ;
#4549 = DIRECTION ( 'NONE',  ( 0.9999697198139515519, 0.000000000000000000, 0.007781995580013368816 ) ) ;
#4550 = EDGE_LOOP ( 'NONE', ( #55627, #25518, #33804, #3183 ) ) ;
#4551 = CARTESIAN_POINT ( 'NONE',  ( -20.54204810873173415, 0.000000000000000000, 4.860550213503115558 ) ) ;
#4552 = FACE_OUTER_BOUND ( 'NONE', #4108, .T. ) ;
#4553 = DIRECTION ( 'NONE',  ( -0.005002170337468016433, -0.7660444431189770143, 0.6427681459581293666 ) ) ;
#4554 = ADVANCED_FACE ( 'NONE', ( #20522 ), #32721, .F. ) ;
#4555 = CARTESIAN_POINT ( 'NONE',  ( -24.53374897521541698, 18.49370927080960669, -4.545578601930409413 ) ) ;
#4556 = EDGE_CURVE ( 'NONE', #55970, #15628, #40965, .T. ) ;
#4557 = DIRECTION ( 'NONE',  ( 0.005002170337468016433, -0.7660444431189770143, -0.6427681459581293666 ) ) ;
#4558 = ADVANCED_FACE ( 'NONE', ( #28768 ), #41260, .F. ) ;
#4559 = DIRECTION ( 'NONE',  ( -0.5364919789714478471, 0.6444004775717705469, -0.5449076811759709926 ) ) ;
#4560 = ORIENTED_EDGE ( 'NONE', *, *, #55040, .F. ) ;
#4561 = VECTOR ( 'NONE', #52467, 999.9999999999998863 ) ;
#4562 = ORIENTED_EDGE ( 'NONE', *, *, #21166, .F. ) ;
#4563 = LINE ( 'NONE', #39195, #29535 ) ;
#4564 = LINE ( 'NONE', #25040, #4120 ) ;
#4565 = EDGE_LOOP ( 'NONE', ( #19931, #23706, #10728, #20773 ) ) ;
#4566 = CARTESIAN_POINT ( 'NONE',  ( -10.27421835998572064, 0.000000000000000000, 10.96090226820206048 ) ) ;
#4567 = ORIENTED_EDGE ( 'NONE', *, *, #37915, .F. ) ;
#4568 = EDGE_CURVE ( 'NONE', #40584, #5725, #19387, .T. ) ;
#4569 = DIRECTION ( 'NONE',  ( 0.007781995580012662783, 0.000000000000000000, -0.9999697198139514409 ) ) ;
#4570 = VERTEX_POINT ( 'NONE', #50028 ) ;
#4571 = CARTESIAN_POINT ( 'NONE',  ( -12.97282572840506276, 4.172053068839010947, 1.587907467427786878 ) ) ;
#4572 = EDGE_CURVE ( 'NONE', #45990, #32478, #33012, .T. ) ;
#4573 = ORIENTED_EDGE ( 'NONE', *, *, #4877, .T. ) ;
#4574 = ORIENTED_EDGE ( 'NONE', *, *, #9358, .F. ) ;
#4575 = VERTEX_POINT ( 'NONE', #11140 ) ;
#4576 = CARTESIAN_POINT ( 'NONE',  ( -17.26532721389163072, 0.000000000000000000, 13.67648636611514590 ) ) ;
#4577 = DIRECTION ( 'NONE',  ( 0.000000000000000000, -1.000000000000000000, 0.000000000000000000 ) ) ;
#4578 = FACE_OUTER_BOUND ( 'NONE', #47962, .T. ) ;
#4579 = EDGE_CURVE ( 'NONE', #35206, #4870, #46073, .T. ) ;
#4580 = DIRECTION ( 'NONE',  ( 0.6427681459581294776, -0.7660444431189769032, 0.005002170337467562802 ) ) ;
#4581 = ORIENTED_EDGE ( 'NONE', *, *, #27597, .T. ) ;
#4582 = ORIENTED_EDGE ( 'NONE', *, *, #53363, .T. ) ;
#4583 = ADVANCED_FACE ( 'NONE', ( #37614 ), #28529, .F. ) ;
#4584 = ORIENTED_EDGE ( 'NONE', *, *, #9060, .T. ) ;
#4585 = DIRECTION ( 'NONE',  ( -0.6427681459581293666, -0.7660444431189770143, -0.005002170337467561935 ) ) ;
#4586 = VERTEX_POINT ( 'NONE', #42152 ) ;
#4587 = LINE ( 'NONE', #16515, #28420 ) ;
#4588 = ORIENTED_EDGE ( 'NONE', *, *, #12266, .F. ) ;
#4589 = DIRECTION ( 'NONE',  ( 0.6427681459581294776, -0.7660444431189769032, 0.005002170337467562802 ) ) ;
#4590 = CARTESIAN_POINT ( 'NONE',  ( -10.80559463571480450, -0.1191753592594190225, 6.682978866688390696 ) ) ;
#4591 = VERTEX_POINT ( 'NONE', #32784 ) ;
#4592 = CARTESIAN_POINT ( 'NONE',  ( -13.20787951780664393, 0.000000000000000000, 3.978956213504597272 ) ) ;
#4593 = VERTEX_POINT ( 'NONE', #50093 ) ;
#4594 = VECTOR ( 'NONE', #31004, 999.9999999999998863 ) ;
#4595 = DIRECTION ( 'NONE',  ( 0.000000000000000000, 0.000000000000000000, 1.000000000000000000 ) ) ;
#4596 = VERTEX_POINT ( 'NONE', #54940 ) ;
#4597 = CARTESIAN_POINT ( 'NONE',  ( 2.072287782118878319, 0.000000000000000000, -2.950529333540147015 ) ) ;
#4598 = CARTESIAN_POINT ( 'NONE',  ( -11.36813265058999889, 0.000000000000000000, 6.409272024086013708 ) ) ;
#4599 = DIRECTION ( 'NONE',  ( -0.005002170337468016433, -0.7660444431189770143, 0.6427681459581293666 ) ) ;
#4600 = EDGE_LOOP ( 'NONE', ( #20810, #41303, #5689, #28557 ) ) ;
#4601 = DIRECTION ( 'NONE',  ( 0.5449076811759707706, 0.6444004775717708799, -0.5364919789714476250 ) ) ;
#4602 = DIRECTION ( 'NONE',  ( 0.000000000000000000, -1.000000000000000000, 0.000000000000000000 ) ) ;
#4603 = CARTESIAN_POINT ( 'NONE',  ( -10.36412444188097837, -0.03739765774599676518, 0.8457230899663811252 ) ) ;
#4604 = EDGE_CURVE ( 'NONE', #40212, #48365, #46128, .T. ) ;
#4605 = LINE ( 'NONE', #48047, #35925 ) ;
#4606 = CARTESIAN_POINT ( 'NONE',  ( 2.072287782118878319, 0.000000000000000000, -2.950529333540147015 ) ) ;
#4607 = DIRECTION ( 'NONE',  ( 0.007781995580012662783, 0.000000000000000000, -0.9999697198139514409 ) ) ;
#4608 = EDGE_CURVE ( 'NONE', #49012, #1661, #2674, .T. ) ;
#4609 = FILL_AREA_STYLE ('',( #48050 ) ) ;
#4610 = EDGE_LOOP ( 'NONE', ( #6702, #32543, #4812, #11437 ) ) ;
#4611 = CARTESIAN_POINT ( 'NONE',  ( -9.342070512798265725, 0.000000000000000000, 10.59882438848031505 ) ) ;
#4612 = ADVANCED_FACE ( 'NONE', ( #45854 ), #11204, .F. ) ;
#4613 = CARTESIAN_POINT ( 'NONE',  ( -21.47419595591918906, 0.000000000000000000, 5.222628093224860102 ) ) ;
#4614 = CARTESIAN_POINT ( 'NONE',  ( -10.68913154225971418, 0.000000000000000000, 4.567895818681203757 ) ) ;
#4615 = ORIENTED_EDGE ( 'NONE', *, *, #44256, .T. ) ;
#4616 = DIRECTION ( 'NONE',  ( 0.007781995580012663651, -3.146120232559066537E-19, -0.9999697198139514409 ) ) ;
#4617 = CARTESIAN_POINT ( 'NONE',  ( 4.918891891700034158, -1.130528823225185109, 1.997863978257570228 ) ) ;
#4618 = EDGE_LOOP ( 'NONE', ( #48224, #4467, #25533, #11808, #50889 ) ) ;
#4619 = EDGE_CURVE ( 'NONE', #27886, #21134, #6977, .T. ) ;
#4620 = EDGE_CURVE ( 'NONE', #34091, #12500, #2948, .T. ) ;
#4621 = ADVANCED_FACE ( 'NONE', ( #2416 ), #7504, .F. ) ;
#4622 = CARTESIAN_POINT ( 'NONE',  ( -16.47183400971537282, 0.000000000000000000, 5.430883644159590240 ) ) ;
#4623 = VECTOR ( 'NONE', #33418, 1000.000000000000227 ) ;
#4624 = DIRECTION ( 'NONE',  ( 0.000000000000000000, -0.000000000000000000, -1.000000000000000000 ) ) ;
#4625 = FACE_OUTER_BOUND ( 'NONE', #36330, .T. ) ;
#4626 = DIRECTION ( 'NONE',  ( 0.000000000000000000, -1.000000000000000000, 0.000000000000000000 ) ) ;
#4627 = ORIENTED_EDGE ( 'NONE', *, *, #19660, .T. ) ;
#4628 = ORIENTED_EDGE ( 'NONE', *, *, #18960, .F. ) ;
#4629 = CARTESIAN_POINT ( 'NONE',  ( -56.66762604419704985, 5.055998648713356580, -3.000000000000007105 ) ) ;
#4630 = CARTESIAN_POINT ( 'NONE',  ( -24.74851972188836058, 18.25476655873277920, 4.557895469182953185 ) ) ;
#4631 = DIRECTION ( 'NONE',  ( 0.5364919789714477361, 0.6444004775717706579, 0.5449076811759711036 ) ) ;
#4632 = CARTESIAN_POINT ( 'NONE',  ( -16.53317331066696383, 0.000000000000000000, 13.31285208727739899 ) ) ;
#4633 = LINE ( 'NONE', #17704, #42784 ) ;
#4634 = VECTOR ( 'NONE', #27506, 1000.000000000000000 ) ;
#4635 = EDGE_CURVE ( 'NONE', #3505, #30167, #37904, .T. ) ;
#4636 = PLANE ( 'NONE',  #36693 ) ;
#4637 = ORIENTED_EDGE ( 'NONE', *, *, #26651, .T. ) ;
#4638 = DIRECTION ( 'NONE',  ( -1.000000000000000000, 0.000000000000000000, 0.000000000000000000 ) ) ;
#4639 = AXIS2_PLACEMENT_3D ( 'NONE', #44559, #49396, #36333 ) ;
#4640 = ADVANCED_FACE ( 'NONE', ( #6676 ), #2114, .F. ) ;
#4641 = CARTESIAN_POINT ( 'NONE',  ( -18.66354898467281132, 0.000000000000000000, 14.21960318569776582 ) ) ;
#4642 = ORIENTED_EDGE ( 'NONE', *, *, #21273, .F. ) ;
#4643 = EDGE_CURVE ( 'NONE', #47620, #19207, #7234, .T. ) ;
#4644 = CARTESIAN_POINT ( 'NONE',  ( -22.71004419446258993, -5.375054281893161701, 14.32466392724574256 ) ) ;
#4645 = DIRECTION ( 'NONE',  ( 0.9999697198139515519, 0.000000000000000000, 0.007781995580013368816 ) ) ;
#4646 = CARTESIAN_POINT ( 'NONE',  ( -16.87027461792824212, -0.1191753592594190225, 9.771361154204708299 ) ) ;
#4647 = ORIENTED_EDGE ( 'NONE', *, *, #10087, .F. ) ;
#4648 = EDGE_CURVE ( 'NONE', #3650, #47902, #19742, .T. ) ;
#4649 = CARTESIAN_POINT ( 'NONE',  ( -15.86710544311044302, 0.000000000000000000, 13.13336954653252953 ) ) ;
#4650 = EDGE_LOOP ( 'NONE', ( #27067, #1842, #2188, #36358 ) ) ;
#4651 = ORIENTED_EDGE ( 'NONE', *, *, #24419, .F. ) ;
#4652 = EDGE_LOOP ( 'NONE', ( #16229, #4076, #49345, #27637 ) ) ;
#4653 =( BOUNDED_SURFACE ( )  B_SPLINE_SURFACE ( 3, 2, ( 
 ( #2393, #19719, #37043 ),
 ( #54345, #51208, #4073 ),
 ( #16279, #33600, #34724 ),
 ( #25113, #25373, #34195 ),
 ( #38733, #8620, #51507 ),
 ( #42674, #29917, #52041 ),
 ( #17397, #13156, #3775 ),
 ( #8323, #21405, #20562 ),
 ( #25641, #21096, #38424 ),
 ( #43280, #42969, #47216 ),
 ( #12600, #4371, #55750 ),
 ( #56045, #30494, #17138 ),
 ( #25951, #21681, #46662 ),
 ( #7786, #7479, #51758 ),
 ( #46962, #12012, #55189 ),
 ( #42421, #50910, #29663 ),
 ( #38995, #16864, #47508 ),
 ( #37885, #34448, #24803 ),
 ( #29350, #42123, #30190 ),
 ( #3229, #12868, #12323 ),
 ( #3512, #8063, #20821 ),
 ( #38139, #61, #55457 ),
 ( #16556, #33892, #354 ),
 ( #18828, #22234, #9161 ) ),
 .UNSPECIFIED., .F., .F., .F. ) 
 B_SPLINE_SURFACE_WITH_KNOTS ( ( 4, 2, 2, 2, 2, 2, 2, 2, 2, 2, 2, 4 ),
 ( 3, 3 ),
 ( 0.008994972463978564287, 0.01138926720843922921, 0.01258641458066956167, 0.01378356195289989587, 0.01617785669736056253, 0.01857215144182122746, 0.02096644618628189238, 0.02336074093074255731, 0.02575503567520322223, 0.02695218304743355470, 0.02755075673354872093, 0.02814933041966388716 ),
 ( 0.000000000000000000, 1.000000000000000000 ),
 .UNSPECIFIED. ) 
 GEOMETRIC_REPRESENTATION_ITEM ( )  RATIONAL_B_SPLINE_SURFACE ( (
 ( 1.000000000000000000, 0.7302382283600404866, 1.000000000000000000),
 ( 1.000000000000000000, 0.7302057701444414350, 1.000000000000000000),
 ( 1.000000000000000000, 0.7302261543189000337, 1.000000000000000000),
 ( 1.000000000000000000, 0.7302340627759330571, 1.000000000000000000),
 ( 1.000000000000000000, 0.7302358193534487230, 1.000000000000000000),
 ( 1.000000000000000000, 0.7302356584982084842, 1.000000000000000000),
 ( 1.000000000000000000, 0.7302336981036621211, 1.000000000000000000),
 ( 1.000000000000000000, 0.7302244465159644093, 1.000000000000000000),
 ( 1.000000000000000000, 0.7302382397051314644, 1.000000000000000000),
 ( 1.000000000000000000, 0.7302438375851851848, 1.000000000000000000),
 ( 1.000000000000000000, 0.7302379409314863068, 1.000000000000000000),
 ( 1.000000000000000000, 0.7302249128351889773, 1.000000000000000000),
 ( 1.000000000000000000, 0.7302266904876862919, 1.000000000000000000),
 ( 1.000000000000000000, 0.7302305284562681242, 1.000000000000000000),
 ( 1.000000000000000000, 0.7302278475313366268, 1.000000000000000000),
 ( 1.000000000000000000, 0.7302208473858853299, 1.000000000000000000),
 ( 1.000000000000000000, 0.7302205818823860328, 1.000000000000000000),
 ( 1.000000000000000000, 0.7302413824363716000, 1.000000000000000000),
 ( 1.000000000000000000, 0.7302489349993748213, 1.000000000000000000),
 ( 1.000000000000000000, 0.7302381596253557650, 1.000000000000000000),
 ( 1.000000000000000000, 0.7302138215221798401, 1.000000000000000000),
 ( 1.000000000000000000, 0.7302588551337141354, 1.000000000000000000),
 ( 1.000000000000000000, 0.7302821861416568527, 1.000000000000000000),
 ( 1.000000000000000000, 0.7303030204721981944, 1.000000000000000000) ) ) 
 REPRESENTATION_ITEM ( '' )  SURFACE ( )  );
#4654 = VERTEX_POINT ( 'NONE', #54364 ) ;
#4655 = DIRECTION ( 'NONE',  ( 0.005002170337468016433, -0.7660444431189770143, -0.6427681459581293666 ) ) ;
#4656 = PRODUCT ( 'Swivel Catch Post', 'Swivel Catch Post', '', ( #13009 ) ) ;
#4657 = ORIENTED_EDGE ( 'NONE', *, *, #54244, .F. ) ;
#4658 = LINE ( 'NONE', #43829, #31280 ) ;
#4659 = VECTOR ( 'NONE', #15050, 999.9999999999998863 ) ;
#4660 = AXIS2_PLACEMENT_3D ( 'NONE', #21217, #55571, #56151 ) ;
#4661 = ORIENTED_EDGE ( 'NONE', *, *, #29292, .F. ) ;
#4662 = CARTESIAN_POINT ( 'NONE',  ( -16.01042127810387683, -4.079838673713161334, 9.596633394776388215 ) ) ;
#4663 = ORIENTED_EDGE ( 'NONE', *, *, #53798, .T. ) ;
#4664 = CARTESIAN_POINT ( 'NONE',  ( -10.94028622754223967, 0.000000000000000000, 11.14038480894692995 ) ) ;
#4665 = ORIENTED_EDGE ( 'NONE', *, *, #6546, .T. ) ;
#4666 = PLANE ( 'NONE',  #18415 ) ;
#4667 = CARTESIAN_POINT ( 'NONE',  ( -18.67697421479882181, -0.1191753592594197858, 4.036397482078229793 ) ) ;
#4668 = LINE ( 'NONE', #38773, #52162 ) ;
#4669 = LINE ( 'NONE', #35612, #16915 ) ;
#4670 = DIRECTION ( 'NONE',  ( -0.005961354470445682716, -0.6427876096865404731, 0.7660212471507180654 ) ) ;
#4671 = ORIENTED_EDGE ( 'NONE', *, *, #17504, .T. ) ;
#4672 = ORIENTED_EDGE ( 'NONE', *, *, #31453, .F. ) ;
#4673 = LINE ( 'NONE', #51549, #55780 ) ;
#4674 = PLANE ( 'NONE',  #374 ) ;
#4675 = EDGE_CURVE ( 'NONE', #15181, #18631, #20584, .T. ) ;
#4676 = AXIS2_PLACEMENT_3D ( 'NONE', #36363, #18483, #52833 ) ;
#4677 = PLANE ( 'NONE',  #37867 ) ;
#4678 = LINE ( 'NONE', #40154, #55719 ) ;
#4679 = LINE ( 'NONE', #17451, #39450 ) ;
#4680 = CARTESIAN_POINT ( 'NONE',  ( -15.03495456790438389, -0.1191753592594197858, 12.77051346725278158 ) ) ;
#4681 = ORIENTED_EDGE ( 'NONE', *, *, #19211, .F. ) ;
#4682 = DIRECTION ( 'NONE',  ( 0.9999697198139515519, 0.000000000000000000, 0.007781995580013368816 ) ) ;
#4683 = CARTESIAN_POINT ( 'NONE',  ( -10.86613305818024244, 0.000000000000000000, 1.611861793503084783 ) ) ;
#4684 = EDGE_LOOP ( 'NONE', ( #28834, #20802, #50716, #30370 ) ) ;
#4685 = EDGE_CURVE ( 'NONE', #29674, #19075, #29083, .T. ) ;
#4686 = ADVANCED_FACE ( 'NONE', ( #55212 ), #20283, .F. ) ;
#4687 = EDGE_CURVE ( 'NONE', #41210, #44810, #23704, .T. ) ;
#4688 = PLANE ( 'NONE',  #54263 ) ;
#4689 = CARTESIAN_POINT ( 'NONE',  ( -18.81513686845778111, 0.000000000000000000, 7.997972008123892529 ) ) ;
#4690 = DIRECTION ( 'NONE',  ( -0.6427681459581293666, -0.7660444431189770143, -0.005002170337467561935 ) ) ;
#4691 = EDGE_CURVE ( 'NONE', #51537, #46161, #15215, .T. ) ;
#4692 = DIRECTION ( 'NONE',  ( -0.6427681459581293666, -0.7660444431189770143, -0.005002170337467561935 ) ) ;
#4693 = DIRECTION ( 'NONE',  ( 0.000000000000000000, -0.000000000000000000, -1.000000000000000000 ) ) ;
#4694 = ORIENTED_EDGE ( 'NONE', *, *, #37182, .T. ) ;
#4695 = ORIENTED_EDGE ( 'NONE', *, *, #8334, .T. ) ;
#4696 = DIRECTION ( 'NONE',  ( 0.9999697198139515519, 0.000000000000000000, 0.007781995580013368816 ) ) ;
#4697 = CARTESIAN_POINT ( 'NONE',  ( -26.13493519185646008, 0.000000000000000000, 7.033017491833586377 ) ) ;
#4698 = DIRECTION ( 'NONE',  ( 0.005002170337468016433, -0.7660444431189770143, -0.6427681459581293666 ) ) ;
#4699 = VECTOR ( 'NONE', #6389, 1000.000000000000000 ) ;
#4700 = VECTOR ( 'NONE', #6355, 1000.000000000000114 ) ;
#4701 = CARTESIAN_POINT ( 'NONE',  ( -22.04728230093569152, 19.65758605842115969, -4.422151119964278010 ) ) ;
#4702 = DIRECTION ( 'NONE',  ( -0.7660212471507179544, -0.6427876096865405842, -0.005961354470445141482 ) ) ;
#4703 = PLANE ( 'NONE',  #4709 ) ;
#4704 = LINE ( 'NONE', #440, #23859 ) ;
#4706 = EDGE_CURVE ( 'NONE', #32268, #14910, #51236, .T. ) ;
#4705 = ORIENTED_EDGE ( 'NONE', *, *, #25445, .F. ) ;
#4707 = DIRECTION ( 'NONE',  ( 0.6246952433987893460, 0.7422098413412802076, -0.2426528472758539279 ) ) ;
#4708 = CARTESIAN_POINT ( 'NONE',  ( -63.56784591066751489, 8.775889882925216767, 5.000000000000000000 ) ) ;
#4709 = AXIS2_PLACEMENT_3D ( 'NONE', #22024, #17783, #26559 ) ;
#4710 = ADVANCED_FACE ( 'NONE', ( #82 ), #13467, .F. ) ;
#4711 = EDGE_LOOP ( 'NONE', ( #20363, #4716, #10512, #3937 ) ) ;
#4712 = LINE ( 'NONE', #449, #11980 ) ;
#4713 = ORIENTED_EDGE ( 'NONE', *, *, #21220, .T. ) ;
#4714 = DIRECTION ( 'NONE',  ( -0.7660212471507179544, -0.6427876096865405842, -0.005961354470445141482 ) ) ;
#4715 = FACE_OUTER_BOUND ( 'NONE', #54681, .T. ) ;
#4716 = ORIENTED_EDGE ( 'NONE', *, *, #35208, .F. ) ;
#4717 = EDGE_CURVE ( 'NONE', #30652, #9548, #38448, .T. ) ;
#4718 = AXIS2_PLACEMENT_3D ( 'NONE', #553, #17585, #30913 ) ;
#4719 = ORIENTED_EDGE ( 'NONE', *, *, #20424, .T. ) ;
#4720 = ADVANCED_FACE ( 'NONE', ( #55776 ), #4391, .F. ) ;
#4721 = VECTOR ( 'NONE', #41544, 1000.000000000000227 ) ;
#4722 = ORIENTED_EDGE ( 'NONE', *, *, #1156, .T. ) ;
#4723 = VERTEX_POINT ( 'NONE', #42991 ) ;
#4724 = EDGE_LOOP ( 'NONE', ( #46716, #23607, #27045, #41861 ) ) ;
#4725 = EDGE_LOOP ( 'NONE', ( #21949, #25511, #26549, #4961 ) ) ;
#4726 = CARTESIAN_POINT ( 'NONE',  ( -11.16945636101648809, 0.000000000000000000, 6.580144182496990624 ) ) ;
#4727 = LINE ( 'NONE', #25751, #19299 ) ;
#4728 = CARTESIAN_POINT ( 'NONE',  ( -16.99924723426068951, 0.000000000000000000, 13.49389102713827171 ) ) ;
#4729 = ORIENTED_EDGE ( 'NONE', *, *, #45073, .F. ) ;
#4730 = CARTESIAN_POINT ( 'NONE',  ( -17.39116798849241974, 0.000000000000000000, 4.146406951555302811 ) ) ;
#4731 = VERTEX_POINT ( 'NONE', #34748 ) ;
#4732 = EDGE_LOOP ( 'NONE', ( #36213, #20385, #16789, #18805 ) ) ;
#4733 = CARTESIAN_POINT ( 'NONE',  ( -16.98309541363131814, 4.981562823951510843, 11.65372539905892069 ) ) ;
#4734 = FACE_OUTER_BOUND ( 'NONE', #19166, .T. ) ;
#4735 = CARTESIAN_POINT ( 'NONE',  ( -66.74342152241241877, -11.36145478494482042, -7.448289400635804469 ) ) ;
#4736 = AXIS2_PLACEMENT_3D ( 'NONE', #39028, #4403, #17739 ) ;
#4737 = ORIENTED_EDGE ( 'NONE', *, *, #55921, .F. ) ;
#4738 = FACE_OUTER_BOUND ( 'NONE', #20647, .T. ) ;
#4739 = VERTEX_POINT ( 'NONE', #8646 ) ;
#4740 = VECTOR ( 'NONE', #4378, 999.9999999999998863 ) ;
#4741 = VECTOR ( 'NONE', #54260, 1000.000000000000227 ) ;
#4742 = DIRECTION ( 'NONE',  ( 0.005002170337468016433, -0.7660444431189770143, -0.6427681459581293666 ) ) ;
#4743 = DIRECTION ( 'NONE',  ( 0.9999697198139515519, 0.000000000000000000, 0.007781995580013368816 ) ) ;
#4744 = CARTESIAN_POINT ( 'NONE',  ( -14.94760462649100496, 0.000000000000000000, 2.488088991209854051 ) ) ;
#4745 = AXIS2_PLACEMENT_3D ( 'NONE', #29991, #26040, #16950 ) ;
#4746 = VECTOR ( 'NONE', #52021, 1000.000000000000227 ) ;
#4747 = DIRECTION ( 'NONE',  ( 0.9999697198139515519, 0.000000000000000000, 0.007781995580013368816 ) ) ;
#4748 = LINE ( 'NONE', #52174, #24116 ) ;
#4749 = DIRECTION ( 'NONE',  ( -0.005961354470445682716, -0.6427876096865404731, 0.7660212471507180654 ) ) ;
#4750 = DIRECTION ( 'NONE',  ( 0.000000000000000000, -1.000000000000000000, 0.000000000000000000 ) ) ;
#4751 = CARTESIAN_POINT ( 'NONE',  ( 0.1285714285714296967, 2.000000000000000000, 5.998622290806041590 ) ) ;
#4752 = ORIENTED_EDGE ( 'NONE', *, *, #55010, .F. ) ;
#4753 = CARTESIAN_POINT ( 'NONE',  ( -11.09208034454450775, 1.905425754524005200, 4.316990091452962197 ) ) ;
#4754 = ADVANCED_FACE ( 'NONE', ( #16889 ), #8346, .F. ) ;
#4755 = CARTESIAN_POINT ( 'NONE',  ( -30.79411802867772607, 0.000000000000000000, 8.643412946479525516 ) ) ;
#4756 = CARTESIAN_POINT ( 'NONE',  ( -14.01701317841955508, 0.000000000000000000, 2.326005055450897085 ) ) ;
#4757 = LINE ( 'NONE', #38565, #22675 ) ;
#4758 = VECTOR ( 'NONE', #32489, 1000.000000000000227 ) ;
#4759 = CARTESIAN_POINT ( 'NONE',  ( -19.95056665410288943, 19.40776001008019236, -4.333296610429257179 ) ) ;
#4760 = FACE_OUTER_BOUND ( 'NONE', #19363, .T. ) ;
#4761 = EDGE_CURVE ( 'NONE', #6528, #16795, #51529, .T. ) ;
#4762 = EDGE_CURVE ( 'NONE', #17219, #12564, #4102, .T. ) ;
#4763 = CARTESIAN_POINT ( 'NONE',  ( -21.47419595591918906, 0.000000000000000000, 5.222628093224860102 ) ) ;
#4764 = DIRECTION ( 'NONE',  ( 0.9999697198139515519, 0.000000000000000000, 0.007781995580013368816 ) ) ;
#4765 = ORIENTED_EDGE ( 'NONE', *, *, #13222, .F. ) ;
#4766 = PLANE ( 'NONE',  #34785 ) ;
#4767 = FACE_OUTER_BOUND ( 'NONE', #9387, .T. ) ;
#4768 = DIRECTION ( 'NONE',  ( -0.7660212471507179544, -0.6427876096865405842, -0.005961354470445141482 ) ) ;
#4769 = CARTESIAN_POINT ( 'NONE',  ( -12.13851405436063047, 0.000000000000000000, 11.68505802764555135 ) ) ;
#4770 = CARTESIAN_POINT ( 'NONE',  ( -17.77262100021681945, -5.051250379848161387, 11.87538371510229673 ) ) ;
#4771 = VECTOR ( 'NONE', #1406, 1000.000000000000227 ) ;
#4772 = CARTESIAN_POINT ( 'NONE',  ( -1.086233639165236964, 0.000000000000000000, -2.796443541562362078 ) ) ;
#4773 = DIRECTION ( 'NONE',  ( 0.007781995580012663651, -3.146120232559066537E-19, -0.9999697198139514409 ) ) ;
#4774 = LINE ( 'NONE', #39429, #11461 ) ;
#4775 = AXIS2_PLACEMENT_3D ( 'NONE', #34481, #35334, #18270 ) ;
#4776 = CARTESIAN_POINT ( 'NONE',  ( -16.79925329029790149, 0.000000000000000000, 13.49544742625427496 ) ) ;
#4777 = VECTOR ( 'NONE', #3079, 999.9999999999998863 ) ;
#4778 = AXIS2_PLACEMENT_3D ( 'NONE', #11542, #24866, #50705 ) ;
#4779 = EDGE_LOOP ( 'NONE', ( #37352, #48207, #16588, #21709 ) ) ;
#4780 = ADVANCED_FACE ( 'NONE', ( #25976 ), #378, .F. ) ;
#4781 = VECTOR ( 'NONE', #14007, 999.9999999999998863 ) ;
#4782 = EDGE_LOOP ( 'NONE', ( #24536, #15010, #279, #31129 ) ) ;
#4783 = EDGE_LOOP ( 'NONE', ( #24569, #29689, #34119, #52291 ) ) ;
#4784 = VECTOR ( 'NONE', #45135, 1000.000000000000227 ) ;
#4785 = ORIENTED_EDGE ( 'NONE', *, *, #44025, .F. ) ;
#4786 = EDGE_CURVE ( 'NONE', #48904, #36106, #7815, .T. ) ;
#4787 = ORIENTED_EDGE ( 'NONE', *, *, #11387, .T. ) ;
#4788 = PLANE ( 'NONE',  #52303 ) ;
#4789 = DIRECTION ( 'NONE',  ( -0.9999697198139514409, -0.000000000000000000, -0.007781995580013368816 ) ) ;
#4790 = VERTEX_POINT ( 'NONE', #3532 ) ;
#4791 = ORIENTED_EDGE ( 'NONE', *, *, #38882, .F. ) ;
#4792 = EDGE_CURVE ( 'NONE', #25448, #49293, #43544, .T. ) ;
#4793 = AXIS2_PLACEMENT_3D ( 'NONE', #46562, #7676, #4280 ) ;
#4794 = AXIS2_PLACEMENT_3D ( 'NONE', #51459, #17346, #4580 ) ;
#4795 = PLANE ( 'NONE',  #49356 ) ;
#4796 = ORIENTED_EDGE ( 'NONE', *, *, #48274, .F. ) ;
#4797 = FACE_OUTER_BOUND ( 'NONE', #4115, .T. ) ;
#4798 = CARTESIAN_POINT ( 'NONE',  ( -9.290790399115168796, 0.000000000000000000, 4.009439906764677097 ) ) ;
#4799 = ORIENTED_EDGE ( 'NONE', *, *, #39261, .F. ) ;
#4800 = CARTESIAN_POINT ( 'NONE',  ( -18.66354898467281132, 0.000000000000000000, 14.21960318569776582 ) ) ;
#4801 = VECTOR ( 'NONE', #759, 1000.000000000000114 ) ;
#4802 = ORIENTED_EDGE ( 'NONE', *, *, #26406, .F. ) ;
#4803 = CARTESIAN_POINT ( 'NONE',  ( -5.619483069058131441, 5.495567360717212857, 5.401171638134291797 ) ) ;
#4804 = VECTOR ( 'NONE', #26216, 1000.000000000000227 ) ;
#4805 = PLANE ( 'NONE',  #55405 ) ;
#4806 = CARTESIAN_POINT ( 'NONE',  ( -15.88130887279446490, 0.000000000000000000, 3.050160814894388839 ) ) ;
#4807 = ORIENTED_EDGE ( 'NONE', *, *, #35426, .F. ) ;
#4808 = DIRECTION ( 'NONE',  ( 0.005961354470445682716, -0.6427876096865404731, -0.7660212471507180654 ) ) ;
#4809 = CARTESIAN_POINT ( 'NONE',  ( -19.08354877797473037, -4.403642575758160760, 11.32175784747634673 ) ) ;
#4810 = DIRECTION ( 'NONE',  ( -0.7660212471507179544, -0.6427876096865405842, -0.005961354470445141482 ) ) ;
#4811 = VECTOR ( 'NONE', #9109, 1000.000000000000114 ) ;
#4812 = ORIENTED_EDGE ( 'NONE', *, *, #35245, .T. ) ;
#4813 = DIRECTION ( 'NONE',  ( 0.007781995580012663651, 0.000000000000000000, -0.9999697198139515519 ) ) ;
#4814 = ADVANCED_FACE ( 'NONE', ( #47533 ), #42698, .F. ) ;
#4815 = ORIENTED_EDGE ( 'NONE', *, *, #5590, .F. ) ;
#4816 = VECTOR ( 'NONE', #45377, 1000.000000000000227 ) ;
#4817 = AXIS2_PLACEMENT_3D ( 'NONE', #6504, #40310, #6244 ) ;
#4818 = LINE ( 'NONE', #36319, #30121 ) ;
#4819 = DIRECTION ( 'NONE',  ( 0.005961354470445682716, -0.6427876096865404731, -0.7660212471507180654 ) ) ;
#4820 = CARTESIAN_POINT ( 'NONE',  ( 2.072287782118878319, 0.000000000000000000, -2.950529333540147015 ) ) ;
#4821 = DIRECTION ( 'NONE',  ( 0.007781995580012662783, 0.000000000000000000, -0.9999697198139514409 ) ) ;
#4822 = CARTESIAN_POINT ( 'NONE',  ( -15.50102849149811135, -0.1191753592594197858, 12.95155240711365430 ) ) ;
#4823 = CARTESIAN_POINT ( 'NONE',  ( -12.53330886209764117, 0.000000000000000000, 2.706883655320341919 ) ) ;
#4824 = ADVANCED_FACE ( 'NONE', ( #46982 ), #38163, .F. ) ;
#4825 = CARTESIAN_POINT ( 'NONE',  ( -21.47263955680318404, 0.000000000000000000, 5.022634149262071190 ) ) ;
#4826 = VECTOR ( 'NONE', #12553, 999.9999999999998863 ) ;
#4827 = LINE ( 'NONE', #13621, #53775 ) ;
#4828 = VECTOR ( 'NONE', #47803, 999.9999999999998863 ) ;
#4829 = DIRECTION ( 'NONE',  ( 0.000000000000000000, -0.000000000000000000, -1.000000000000000000 ) ) ;
#4830 = VERTEX_POINT ( 'NONE', #8083 ) ;
#4831 = DIRECTION ( 'NONE',  ( 0.5449076811759707706, 0.6444004775717708799, -0.5364919789714476250 ) ) ;
#4832 = CARTESIAN_POINT ( 'NONE',  ( -17.68586913081282219, 0.000000000000000000, 8.006760230775915588 ) ) ;
#4833 = LINE ( 'NONE', #46959, #31389 ) ;
#4834 = CARTESIAN_POINT ( 'NONE',  ( -20.08902568218405449, -0.6798977022406558213, 4.662888621968888536 ) ) ;
#4835 = VECTOR ( 'NONE', #33509, 1000.000000000000227 ) ;
#4836 = CIRCLE ( 'NONE', #42891, 3.457106781186553235 ) ;
#4837 = CARTESIAN_POINT ( 'NONE',  ( -1.086233639165236964, 0.000000000000000000, -2.796443541562362078 ) ) ;
#4838 = PLANE ( 'NONE',  #35619 ) ;
#4839 = EDGE_CURVE ( 'NONE', #27103, #49013, #33304, .T. ) ;
#4840 = ORIENTED_EDGE ( 'NONE', *, *, #46193, .F. ) ;
#4841 = EDGE_LOOP ( 'NONE', ( #27717, #13397, #38909, #40421 ) ) ;
#4842 = LINE ( 'NONE', #34121, #1434 ) ;
#4843 = CARTESIAN_POINT ( 'NONE',  ( -26.13337879274045505, 0.000000000000000000, 6.833023547870798353 ) ) ;
#4844 = ORIENTED_EDGE ( 'NONE', *, *, #52200, .T. ) ;
#4845 = VECTOR ( 'NONE', #12573, 1000.000000000000227 ) ;
#4846 = LINE ( 'NONE', #4566, #45649 ) ;
#4847 = ORIENTED_EDGE ( 'NONE', *, *, #54362, .F. ) ;
#4848 = FACE_OUTER_BOUND ( 'NONE', #48453, .T. ) ;
#4849 = AXIS2_PLACEMENT_3D ( 'NONE', #55133, #24455, #11688 ) ;
#4850 = VERTEX_POINT ( 'NONE', #52365 ) ;
#4851 = DIRECTION ( 'NONE',  ( -0.6427681459581293666, -0.7660444431189770143, -0.005002170337467561935 ) ) ;
#4852 = EDGE_LOOP ( 'NONE', ( #39303, #3889, #32640 ) ) ;
#4853 = ORIENTED_EDGE ( 'NONE', *, *, #14983, .F. ) ;
#4854 = ORIENTED_EDGE ( 'NONE', *, *, #11241, .F. ) ;
#4855 = DIRECTION ( 'NONE',  ( 0.9999697198139515519, 0.000000000000000000, 0.007781995580013368816 ) ) ;
#4856 = AXIS2_PLACEMENT_3D ( 'NONE', #39915, #5296, #13785 ) ;
#4857 = DIRECTION ( 'NONE',  ( 0.000000000000000000, -0.000000000000000000, -1.000000000000000000 ) ) ;
#4858 = LINE ( 'NONE', #26716, #13975 ) ;
#4859 = VECTOR ( 'NONE', #32127, 999.9999999999998863 ) ;
#4860 = AXIS2_PLACEMENT_3D ( 'NONE', #26091, #55899, #34318 ) ;
#4861 = DIRECTION ( 'NONE',  ( -0.005961354470445682716, -0.6427876096865404731, 0.7660212471507180654 ) ) ;
#4862 = ORIENTED_EDGE ( 'NONE', *, *, #891, .T. ) ;
#4863 = EDGE_CURVE ( 'NONE', #39017, #19141, #55478, .T. ) ;
#4864 = ORIENTED_EDGE ( 'NONE', *, *, #12599, .T. ) ;
#4865 = VECTOR ( 'NONE', #34584, 1000.000000000000227 ) ;
#4866 = VECTOR ( 'NONE', #22457, 1000.000000000000114 ) ;
#4867 = CARTESIAN_POINT ( 'NONE',  ( -69.11692417668358246, -9.015782624321049710, -7.493102809087829108 ) ) ;
#4868 = ORIENTED_EDGE ( 'NONE', *, *, #12708, .F. ) ;
#4869 = FACE_OUTER_BOUND ( 'NONE', #20593, .T. ) ;
#4870 = VERTEX_POINT ( 'NONE', #16581 ) ;
#4871 = DIRECTION ( 'NONE',  ( 0.007781995580012663651, 0.000000000000000000, -0.9999697198139515519 ) ) ;
#4872 = DIRECTION ( 'NONE',  ( 0.005002170337468016433, -0.7660444431189770143, -0.6427681459581293666 ) ) ;
#4873 = EDGE_CURVE ( 'NONE', #16497, #34987, #12889, .T. ) ;
#4874 = ORIENTED_EDGE ( 'NONE', *, *, #10852, .T. ) ;
#4875 = CARTESIAN_POINT ( 'NONE',  ( -14.94916102560700821, 0.000000000000000000, 2.688082935172642962 ) ) ;
#4876 = ORIENTED_EDGE ( 'NONE', *, *, #37121, .F. ) ;
#4877 = EDGE_CURVE ( 'NONE', #19674, #12574, #27079, .T. ) ;
#4878 = EDGE_CURVE ( 'NONE', #33225, #39974, #9185, .T. ) ;
#4879 = FACE_OUTER_BOUND ( 'NONE', #54378, .T. ) ;
#4880 = VECTOR ( 'NONE', #25983, 999.9999999999998863 ) ;
#4881 = ORIENTED_EDGE ( 'NONE', *, *, #28199, .F. ) ;
#4882 = FACE_OUTER_BOUND ( 'NONE', #32398, .T. ) ;
#4883 = LINE ( 'NONE', #35837, #18432 ) ;
#4884 = LINE ( 'NONE', #9419, #3797 ) ;
#4885 = EDGE_CURVE ( 'NONE', #26046, #12964, #18548, .T. ) ;
#4886 = EDGE_LOOP ( 'NONE', ( #14796, #43143, #51428, #32221 ) ) ;
#4887 = VECTOR ( 'NONE', #16681, 1000.000000000000000 ) ;
#4888 = PLANE ( 'NONE',  #44699 ) ;
#4889 = ADVANCED_FACE ( 'NONE', ( #31884 ), #5774, .F. ) ;
#4890 = CARTESIAN_POINT ( 'NONE',  ( 2.072287782118878319, 0.000000000000000000, -2.950529333540147015 ) ) ;
#4891 = CARTESIAN_POINT ( 'NONE',  ( -17.06507362766180691, 0.000000000000000000, 3.410280553659843505 ) ) ;
#4892 = AXIS2_PLACEMENT_3D ( 'NONE', #46012, #11649, #37469 ) ;
#4893 = CARTESIAN_POINT ( 'NONE',  ( -13.60491223078244616, -0.1191753592594181482, 8.138522209111389571 ) ) ;
#4894 = DIRECTION ( 'NONE',  ( 0.7660212471507180654, -0.6427876096865404731, 0.005961354470445141482 ) ) ;
#4895 = ADVANCED_FACE ( 'NONE', ( #48934 ), #14568, .F. ) ;
#4896 = DIRECTION ( 'NONE',  ( 0.9999697198139515519, 0.000000000000000000, 0.007781995580013368816 ) ) ;
#4897 = ORIENTED_EDGE ( 'NONE', *, *, #39111, .T. ) ;
#4898 = DIRECTION ( 'NONE',  ( -0.7660212471507179544, -0.6427876096865405842, -0.005961354470445141482 ) ) ;
#4899 = PLANE ( 'NONE',  #19536 ) ;
#4900 = FACE_OUTER_BOUND ( 'NONE', #19248, .T. ) ;
#4901 = EDGE_LOOP ( 'NONE', ( #10034, #23064, #8167, #23110, #42832 ) ) ;
#4902 = VECTOR ( 'NONE', #36997, 999.9999999999998863 ) ;
#4903 = PLANE ( 'NONE',  #32028 ) ;
#4904 = PLANE ( 'NONE',  #1865 ) ;
#4905 = ORIENTED_EDGE ( 'NONE', *, *, #48509, .F. ) ;
#4906 = VECTOR ( 'NONE', #23868, 1000.000000000000114 ) ;
#4907 = EDGE_CURVE ( 'NONE', #29013, #27017, #13720, .T. ) ;
#4908 = PLANE ( 'NONE',  #7132 ) ;
#4909 = PLANE ( 'NONE',  #3064 ) ;
#4910 = LINE ( 'NONE', #39568, #42288 ) ;
#4911 = DIRECTION ( 'NONE',  ( 0.000000000000000000, -0.000000000000000000, -1.000000000000000000 ) ) ;
#4912 = ADVANCED_FACE ( 'NONE', ( #36418 ), #36167, .F. ) ;
#4913 = ORIENTED_EDGE ( 'NONE', *, *, #4480, .F. ) ;
#4914 = VECTOR ( 'NONE', #21751, 1000.000000000000227 ) ;
#4915 = AXIS2_PLACEMENT_3D ( 'NONE', #48127, #18898, #31674 ) ;
#4916 = ORIENTED_EDGE ( 'NONE', *, *, #5344, .T. ) ;
#4917 = CARTESIAN_POINT ( 'NONE',  ( 0.2239497891030729493, -1.668917571073590622, 5.998622290806042479 ) ) ;
#4918 = DIRECTION ( 'NONE',  ( -0.7660212471507179544, -0.6427876096865405842, -0.005961354470445141482 ) ) ;
#4919 = DIRECTION ( 'NONE',  ( -0.7660212471507179544, -0.6427876096865405842, -0.005961354470445141482 ) ) ;
#4920 = DIRECTION ( 'NONE',  ( 0.005961354470445682716, -0.6427876096865404731, -0.7660212471507180654 ) ) ;
#4921 = LINE ( 'NONE', #22244, #2886 ) ;
#4922 = CARTESIAN_POINT ( 'NONE',  ( -10.66458271510145117, 0.000000000000000000, 1.413424248656298676 ) ) ;
#4923 = ORIENTED_EDGE ( 'NONE', *, *, #5709, .T. ) ;
#4924 = CARTESIAN_POINT ( 'NONE',  ( -12.92677208044202253, 5.143464774974012776, 10.34382034707842912 ) ) ;
#4925 = VECTOR ( 'NONE', #52090, 999.9999999999998863 ) ;
#4926 = LINE ( 'NONE', #12614, #26954 ) ;
#4927 = EDGE_LOOP ( 'NONE', ( #9077, #36170 ) ) ;
#4928 = VECTOR ( 'NONE', #41244, 999.9999999999998863 ) ;
#4929 = DIRECTION ( 'NONE',  ( -0.005002170337468016433, -0.7660444431189770143, 0.6427681459581293666 ) ) ;
#4930 = LINE ( 'NONE', #14008, #21371 ) ;
#4931 = VECTOR ( 'NONE', #34246, 999.9999999999998863 ) ;
#4932 = DIRECTION ( 'NONE',  ( -0.7660212471507179544, -0.6427876096865405842, -0.005961354470445141482 ) ) ;
#4933 = ORIENTED_EDGE ( 'NONE', *, *, #33996, .T. ) ;
#4934 = CARTESIAN_POINT ( 'NONE',  ( -32.65919192261063841, -0.1191753592594197858, 9.467565677904410393 ) ) ;
#4935 = EDGE_CURVE ( 'NONE', #27147, #19740, #22803, .T. ) ;
#4936 = ORIENTED_EDGE ( 'NONE', *, *, #15714, .T. ) ;
#4937 = ORIENTED_EDGE ( 'NONE', *, *, #11703, .T. ) ;
#4938 = ORIENTED_EDGE ( 'NONE', *, *, #33034, .T. ) ;
#4939 = VERTEX_POINT ( 'NONE', #1213 ) ;
#4940 = VECTOR ( 'NONE', #55020, 1000.000000000000227 ) ;
#4941 = DIRECTION ( 'NONE',  ( 0.005002170337468016433, -0.7660444431189770143, -0.6427681459581293666 ) ) ;
#4943 = ADVANCED_FACE ( 'NONE', ( #1771 ), #40423, .F. ) ;
#4942 = ORIENTED_EDGE ( 'NONE', *, *, #45650, .F. ) ;
#4944 = CARTESIAN_POINT ( 'NONE',  ( -20.15831888576414244, 4.333955019861509328, 11.82425529087645977 ) ) ;
#4945 = ADVANCED_FACE ( 'NONE', ( #23385 ), #17999, .F. ) ;
#4946 = AXIS2_PLACEMENT_3D ( 'NONE', #39401, #31458, #18090 ) ;
#4947 = ORIENTED_EDGE ( 'NONE', *, *, #3587, .T. ) ;
#4948 = CARTESIAN_POINT ( 'NONE',  ( -13.05847201118137768, 0.9340140483890039258, 3.486551290014034965 ) ) ;
#4949 = ORIENTED_EDGE ( 'NONE', *, *, #47919, .T. ) ;
#4950 = FACE_OUTER_BOUND ( 'NONE', #48058, .T. ) ;
#4951 = ORIENTED_EDGE ( 'NONE', *, *, #38855, .T. ) ;
#4952 = EDGE_CURVE ( 'NONE', #6678, #15287, #53214, .T. ) ;
#4953 = AXIS2_PLACEMENT_3D ( 'NONE', #13454, #30506, #35310 ) ;
#4954 = VECTOR ( 'NONE', #38998, 1000.000000000000114 ) ;
#4955 = DIRECTION ( 'NONE',  ( -0.7660212471507179544, -0.6427876096865405842, -0.005961354470445141482 ) ) ;
#4956 = CARTESIAN_POINT ( 'NONE',  ( -19.72010057970841146, 0.000000000000000000, 4.866946799230784215 ) ) ;
#4957 = PLANE ( 'NONE',  #27692 ) ;
#4958 = CARTESIAN_POINT ( 'NONE',  ( -9.493658396583240844, 0.000000000000000000, 4.377193210906439980 ) ) ;
#4959 = CARTESIAN_POINT ( 'NONE',  ( -10.94028622754223967, 0.000000000000000000, 11.14038480894692995 ) ) ;
#4960 = ORIENTED_EDGE ( 'NONE', *, *, #9307, .F. ) ;
#4961 = ORIENTED_EDGE ( 'NONE', *, *, #51856, .F. ) ;
#4962 = EDGE_CURVE ( 'NONE', #1446, #37525, #53732, .T. ) ;
#4963 = CARTESIAN_POINT ( 'NONE',  ( -12.33850799832341849, 0.000000000000000000, 11.68350162852954632 ) ) ;
#4964 = DIRECTION ( 'NONE',  ( 0.6427681459581294776, -0.7660444431189769032, 0.005002170337467562802 ) ) ;
#4965 = ADVANCED_FACE ( 'NONE', ( #31626 ), #31037, .F. ) ;
#4966 = FACE_OUTER_BOUND ( 'NONE', #30441, .T. ) ;
#4967 = VECTOR ( 'NONE', #52196, 999.9999999999998863 ) ;
#4968 = PLANE ( 'NONE',  #51177 ) ;
#4969 = VECTOR ( 'NONE', #16187, 1000.000000000000000 ) ;
#4970 = DIRECTION ( 'NONE',  ( 0.007781995580012663651, 0.000000000000000000, -0.9999697198139515519 ) ) ;
#4971 = LINE ( 'NONE', #48704, #15071 ) ;
#4972 = ORIENTED_EDGE ( 'NONE', *, *, #44268, .T. ) ;
#4973 = DIRECTION ( 'NONE',  ( 0.9659258262890692004, -0.2588190451025176864, 0.000000000000000000 ) ) ;
#4974 = CARTESIAN_POINT ( 'NONE',  ( -16.53317331066696383, 0.000000000000000000, 13.31285208727739899 ) ) ;
#4975 = VECTOR ( 'NONE', #14528, 1000.000000000000227 ) ;
#4976 = ORIENTED_EDGE ( 'NONE', *, *, #6151, .T. ) ;
#4977 = EDGE_CURVE ( 'NONE', #8089, #36178, #9469, .T. ) ;
#4978 = CARTESIAN_POINT ( 'NONE',  ( -13.63673279712320507, -0.1191753592594197858, 12.22739664767016521 ) ) ;
#4979 = DIRECTION ( 'NONE',  ( 0.5449076811759707706, 0.6444004775717708799, -0.5364919789714476250 ) ) ;
#4980 = VECTOR ( 'NONE', #22755, 999.9999999999998863 ) ;
#4981 = LINE ( 'NONE', #48712, #23240 ) ;
#4982 = FACE_OUTER_BOUND ( 'NONE', #24546, .T. ) ;
#4983 = DIRECTION ( 'NONE',  ( -0.005961354470445682716, -0.6427876096865404731, 0.7660212471507180654 ) ) ;
#4984 = ORIENTED_EDGE ( 'NONE', *, *, #12178, .F. ) ;
#4985 = VECTOR ( 'NONE', #10632, 1000.000000000000114 ) ;
#4986 = VECTOR ( 'NONE', #48627, 1000.000000000000227 ) ;
#4987 = EDGE_LOOP ( 'NONE', ( #430, #2685, #2467, #17533 ) ) ;
#4988 = AXIS2_PLACEMENT_3D ( 'NONE', #30147, #42077, #17352 ) ;
#4989 = LINE ( 'NONE', #39646, #1248 ) ;
#4990 = LINE ( 'NONE', #35366, #52188 ) ;
#4991 = DIRECTION ( 'NONE',  ( 0.000000000000000000, -0.000000000000000000, -1.000000000000000000 ) ) ;
#4992 = AXIS2_PLACEMENT_3D ( 'NONE', #49734, #24178, #45733 ) ;
#4993 = DIRECTION ( 'NONE',  ( 0.5449076811759707706, 0.6444004775717708799, -0.5364919789714476250 ) ) ;
#4994 = CARTESIAN_POINT ( 'NONE',  ( -12.75054712709212623, 0.000000000000000000, 4.921185475750926130 ) ) ;
#4995 = LINE ( 'NONE', #22325, #3762 ) ;
#4996 = CARTESIAN_POINT ( 'NONE',  ( -13.27065584551087163, 0.000000000000000000, 12.04557950825129176 ) ) ;
#4997 = VECTOR ( 'NONE', #23690, 1000.000000000000000 ) ;
#4998 = DIRECTION ( 'NONE',  ( -0.7660212471507179544, -0.6427876096865405842, -0.005961354470445141482 ) ) ;
#4999 = VECTOR ( 'NONE', #34499, 1000.000000000000000 ) ;
#5000 = FACE_OUTER_BOUND ( 'NONE', #32329, .T. ) ;
#5001 =( BOUNDED_CURVE ( )  B_SPLINE_CURVE ( 2, ( #41086, #22935, #10981 ),
 .UNSPECIFIED., .F., .F. ) 
 B_SPLINE_CURVE_WITH_KNOTS ( ( 3, 3 ),
 ( 0.6158339227882835276, 0.6249778499672641319 ),
 .UNSPECIFIED. ) 
 CURVE ( )  GEOMETRIC_REPRESENTATION_ITEM ( )  RATIONAL_B_SPLINE_CURVE ( ( 0.8614131787543850560, 0.8620336302495723579, 0.8627030601714029689 ) ) 
 REPRESENTATION_ITEM ( '' )  );
#5002 = ORIENTED_EDGE ( 'NONE', *, *, #5251, .T. ) ;
#5003 = CARTESIAN_POINT ( 'NONE',  ( -15.87975247367846166, 0.000000000000000000, 2.850166870931599927 ) ) ;
#5004 = ORIENTED_EDGE ( 'NONE', *, *, #10381, .T. ) ;
#5005 = PLANE ( 'NONE',  #20472 ) ;
#5006 = ADVANCED_FACE ( 'NONE', ( #35588 ), #5232, .F. ) ;
#5007 = CARTESIAN_POINT ( 'NONE',  ( -19.60834386242827776, 0.000000000000000000, 4.298478389818581213 ) ) ;
#5008 = ORIENTED_EDGE ( 'NONE', *, *, #53310, .F. ) ;
#5009 = ADVANCED_FACE ( 'NONE', ( #14013 ), #31341, .F. ) ;
#5010 = VERTEX_POINT ( 'NONE', #15394 ) ;
#5011 = VECTOR ( 'NONE', #37889, 1000.000000000000227 ) ;
#5012 = ORIENTED_EDGE ( 'NONE', *, *, #46994, .T. ) ;
#5013 = VERTEX_POINT ( 'NONE', #23635 ) ;
#5014 = ORIENTED_EDGE ( 'NONE', *, *, #38271, .F. ) ;
#5015 = VECTOR ( 'NONE', #27422, 999.9999999999998863 ) ;
#5016 = EDGE_CURVE ( 'NONE', #2953, #18999, #19375, .T. ) ;
#5017 = ORIENTED_EDGE ( 'NONE', *, *, #54598, .F. ) ;
#5018 = LINE ( 'NONE', #22351, #37457 ) ;
#5019 = CARTESIAN_POINT ( 'NONE',  ( -14.85437466704310516, -5.536956232915666298, 2.474606801569680492 ) ) ;
#5020 = VECTOR ( 'NONE', #52256, 1000.000000000000000 ) ;
#5021 = EDGE_CURVE ( 'NONE', #7467, #10997, #46315, .T. ) ;
#5022 = EDGE_CURVE ( 'NONE', #33373, #44514, #45484, .T. ) ;
#5023 = EDGE_CURVE ( 'NONE', #547, #23151, #3174, .T. ) ;
#5024 = ORIENTED_EDGE ( 'NONE', *, *, #29108, .T. ) ;
#5025 = CARTESIAN_POINT ( 'NONE',  ( -13.14168322917842069, -0.1191753592594198830, 8.323049635317726569 ) ) ;
#5026 = VERTEX_POINT ( 'NONE', #36711 ) ;
#5027 = AXIS2_PLACEMENT_3D ( 'NONE', #34431, #12303, #51740 ) ;
#5028 = EDGE_LOOP ( 'NONE', ( #49887, #43223, #54034, #13700 ) ) ;
#5029 = AXIS2_PLACEMENT_3D ( 'NONE', #48032, #22199, #8587 ) ;
#5030 = AXIS2_PLACEMENT_3D ( 'NONE', #14325, #36177, #40438 ) ;
#5031 = DIRECTION ( 'NONE',  ( -0.9999697198139514409, -0.000000000000000000, -0.007781995580013368816 ) ) ;
#5032 = DIRECTION ( 'NONE',  ( 0.007781995580012662783, 0.000000000000000000, -0.9999697198139514409 ) ) ;
#5033 = VECTOR ( 'NONE', #30539, 1000.000000000000227 ) ;
#5034 = CARTESIAN_POINT ( 'NONE',  ( -67.31362796205407051, -11.38444644600729738, -7.460487485314824418 ) ) ;
#5035 = ORIENTED_EDGE ( 'NONE', *, *, #19421, .T. ) ;
#5036 = CARTESIAN_POINT ( 'NONE',  ( -9.110551994824897193, -1.000000000000000000, 3.538847790438064411 ) ) ;
#5037 = VERTEX_POINT ( 'NONE', #32177 ) ;
#5038 = CIRCLE ( 'NONE', #36775, 3.000000000000001332 ) ;
#5039 = VECTOR ( 'NONE', #3958, 1000.000000000000227 ) ;
#5040 = ADVANCED_FACE ( 'NONE', ( #24467 ), #54554, .F. ) ;
#5041 = DIRECTION ( 'NONE',  ( -0.6427681459581293666, -0.7660444431189770143, -0.005002170337467561935 ) ) ;
#5042 = VECTOR ( 'NONE', #29861, 1000.000000000000227 ) ;
#5043 = ADVANCED_FACE ( 'NONE', ( #36999 ), #20509, .F. ) ;
#5044 = PLANE ( 'NONE',  #55089 ) ;
#5045 = CIRCLE ( 'NONE', #15888, 0.5000000000000004441 ) ;
#5046 = DIRECTION ( 'NONE',  ( -0.5449076811759708816, 0.6444004775717707689, 0.5364919789714475140 ) ) ;
#5047 = CARTESIAN_POINT ( 'NONE',  ( -18.39746900504187010, 0.000000000000000000, 14.03700784672088808 ) ) ;
#5048 = DIRECTION ( 'NONE',  ( 0.9999697198139515519, 0.000000000000000000, 0.007781995580013368816 ) ) ;
#5049 = ADVANCED_FACE ( 'NONE', ( #50607 ), #46482, .T. ) ;
#5050 = CARTESIAN_POINT ( 'NONE',  ( -21.47419595591918906, 0.000000000000000000, 5.222628093224860102 ) ) ;
#5051 = CARTESIAN_POINT ( 'NONE',  ( -14.01623497886155256, -0.1191753592594197858, 2.226008083469502630 ) ) ;
#5052 = VERTEX_POINT ( 'NONE', #11432 ) ;
#5053 = LINE ( 'NONE', #14670, #13852 ) ;
#5054 = ADVANCED_FACE ( 'NONE', ( #7428 ), #42069, .F. ) ;
#5055 = LINE ( 'NONE', #5594, #3845 ) ;
#5056 = LINE ( 'NONE', #30627, #23269 ) ;
#5057 = DIRECTION ( 'NONE',  ( 0.7660212471507180654, -0.6427876096865404731, 0.005961354470445141482 ) ) ;
#5058 = CARTESIAN_POINT ( 'NONE',  ( -37.15891100857655971, 9.472517764717013122, -4.937199669358084186 ) ) ;
#5059 = DIRECTION ( 'NONE',  ( -0.005002170337468016433, -0.7660444431189770143, 0.6427681459581293666 ) ) ;
#5060 = EDGE_CURVE ( 'NONE', #873, #34138, #46061, .T. ) ;
#5061 = DIRECTION ( 'NONE',  ( 0.9999697198139515519, 0.000000000000000000, 0.007781995580013368816 ) ) ;
#5062 = AXIS2_PLACEMENT_3D ( 'NONE', #33287, #29004, #17328 ) ;
#5063 = DIRECTION ( 'NONE',  ( -0.9999697198139514409, -0.000000000000000000, -0.007781995580013368816 ) ) ;
#5064 = VECTOR ( 'NONE', #12049, 999.9999999999998863 ) ;
#5065 = ORIENTED_EDGE ( 'NONE', *, *, #26541, .T. ) ;
#5066 = CARTESIAN_POINT ( 'NONE',  ( -14.04080859257070912, -0.1191753592594186895, 4.441809264765737453 ) ) ;
#5067 = FACE_OUTER_BOUND ( 'NONE', #9366, .T. ) ;
#5068 = LINE ( 'NONE', #51897, #35441 ) ;
#5069 = VECTOR ( 'NONE', #55446, 1000.000000000000114 ) ;
#5070 = LINE ( 'NONE', #13315, #53614 ) ;
#5071 = AXIS2_PLACEMENT_3D ( 'NONE', #37494, #32431, #49459 ) ;
#5072 = LINE ( 'NONE', #48493, #50248 ) ;
#5073 = LINE ( 'NONE', #23974, #30461 ) ;
#5074 = CARTESIAN_POINT ( 'NONE',  ( -17.74404816805336793, 0.000000000000000000, 3.574322630375089460 ) ) ;
#5075 = AXIS2_PLACEMENT_3D ( 'NONE', #26732, #21904, #34689 ) ;
#5076 = CARTESIAN_POINT ( 'NONE',  ( -14.60179020832990204, 0.000000000000000000, 3.968108478200570666 ) ) ;
#5077 = VECTOR ( 'NONE', #49831, 999.9999999999998863 ) ;
#5078 = DIRECTION ( 'NONE',  ( -0.9999697198139514409, -0.000000000000000000, -0.007781995580013368816 ) ) ;
#5079 = VECTOR ( 'NONE', #35946, 1000.000000000000227 ) ;
#5080 = ORIENTED_EDGE ( 'NONE', *, *, #14001, .F. ) ;
#5081 = VECTOR ( 'NONE', #41348, 1000.000000000000227 ) ;
#5082 = AXIS2_PLACEMENT_3D ( 'NONE', #20958, #21249, #30056 ) ;
#5083 = VECTOR ( 'NONE', #39661, 1000.000000000000227 ) ;
#5084 = VERTEX_POINT ( 'NONE', #20202 ) ;
#5085 = VECTOR ( 'NONE', #43649, 1000.000000000000114 ) ;
#5086 = EDGE_LOOP ( 'NONE', ( #37843, #20900, #27083, #46358, #51235, #17479, #25512 ) ) ;
#5087 = VERTEX_POINT ( 'NONE', #23917 ) ;
#5088 = ORIENTED_EDGE ( 'NONE', *, *, #24847, .F. ) ;
#5089 = DIRECTION ( 'NONE',  ( -0.5364919789714478471, 0.6444004775717705469, -0.5449076811759709926 ) ) ;
#5090 = DIRECTION ( 'NONE',  ( 0.000000000000000000, 1.000000000000000000, 0.000000000000000000 ) ) ;
#5091 = EDGE_CURVE ( 'NONE', #50886, #29241, #54300, .T. ) ;
#5092 = EDGE_CURVE ( 'NONE', #40865, #15204, #2038, .T. ) ;
#5093 = ORIENTED_EDGE ( 'NONE', *, *, #2810, .T. ) ;
#5094 = ORIENTED_EDGE ( 'NONE', *, *, #23221, .F. ) ;
#5095 = ADVANCED_FACE ( 'NONE', ( #50019 ), #11701, .F. ) ;
#5096 = AXIS2_PLACEMENT_3D ( 'NONE', #6807, #29739, #46755 ) ;
#5097 = DIRECTION ( 'NONE',  ( 0.7660212471507180654, -0.6427876096865404731, 0.005961354470445141482 ) ) ;
#5098 = ORIENTED_EDGE ( 'NONE', *, *, #35815, .T. ) ;
#5099 = DIRECTION ( 'NONE',  ( -0.7660212471507179544, -0.6427876096865405842, -0.005961354470445141482 ) ) ;
#5100 = DIRECTION ( 'NONE',  ( 0.9999697198139515519, 0.000000000000000000, 0.007781995580013368816 ) ) ;
#5101 = ORIENTED_EDGE ( 'NONE', *, *, #22730, .F. ) ;
#5102 = AXIS2_PLACEMENT_3D ( 'NONE', #16328, #7848, #55509 ) ;
#5103 = CARTESIAN_POINT ( 'NONE',  ( -11.67244013076689946, 0.000000000000000000, 11.50401908778467863 ) ) ;
#5104 = EDGE_LOOP ( 'NONE', ( #29800, #7473, #29320, #10867 ) ) ;
#5105 = LINE ( 'NONE', #39743, #25526 ) ;
#5106 = VECTOR ( 'NONE', #41436, 1000.000000000000000 ) ;
#5107 = LINE ( 'NONE', #38112, #30270 ) ;
#5108 = CARTESIAN_POINT ( 'NONE',  ( -17.20267025855076426, 0.000000000000000000, 5.625202163702363478 ) ) ;
#5109 = LINE ( 'NONE', #35465, #53247 ) ;
#5110 = VECTOR ( 'NONE', #30685, 999.9999999999998863 ) ;
#5111 = AXIS2_PLACEMENT_3D ( 'NONE', #52015, #12575, #8297 ) ;
#5112 = ORIENTED_EDGE ( 'NONE', *, *, #49843, .T. ) ;
#5113 = CARTESIAN_POINT ( 'NONE',  ( -11.87243407472968926, 0.000000000000000000, 11.50246268866867361 ) ) ;
#5114 = FACE_OUTER_BOUND ( 'NONE', #8974, .T. ) ;
#5115 = FACE_OUTER_BOUND ( 'NONE', #17806, .T. ) ;
#5116 = ORIENTED_EDGE ( 'NONE', *, *, #40879, .F. ) ;
#5117 = CARTESIAN_POINT ( 'NONE',  ( -15.34412267118641715, 0.000000000000000000, 5.639665810774401322 ) ) ;
#5118 = ORIENTED_EDGE ( 'NONE', *, *, #42816, .F. ) ;
#5119 = AXIS2_PLACEMENT_3D ( 'NONE', #11619, #15569, #45980 ) ;
#5120 = AXIS2_PLACEMENT_3D ( 'NONE', #42653, #22131, #42397 ) ;
#5121 = LINE ( 'NONE', #572, #2046 ) ;
#5122 = PLANE ( 'NONE',  #41407 ) ;
#5123 = CARTESIAN_POINT ( 'NONE',  ( -14.01623497886155256, -0.1191753592594197858, 2.226008083469502630 ) ) ;
#5124 = CARTESIAN_POINT ( 'NONE',  ( -15.08367142620268098, 0.000000000000000000, 6.180350785979147332 ) ) ;
#5125 = CARTESIAN_POINT ( 'NONE',  ( -11.83564360093636658, 0.000000000000000000, 6.774965815575766825 ) ) ;
#5126 = ADVANCED_FACE ( 'NONE', ( #6334 ), #27928, .F. ) ;
#5127 = DIRECTION ( 'NONE',  ( 0.005961354470445682716, -0.6427876096865404731, -0.7660212471507180654 ) ) ;
#5128 = CARTESIAN_POINT ( 'NONE',  ( -21.93567466420777379, 19.99370817364452790, -4.408991681665293427 ) ) ;
#5129 = VECTOR ( 'NONE', #24464, 999.9999999999998863 ) ;
#5130 = VECTOR ( 'NONE', #9816, 1000.000000000000227 ) ;
#5131 = LINE ( 'NONE', #43709, #51056 ) ;
#5132 = EDGE_CURVE ( 'NONE', #39753, #44131, #45233, .T. ) ;
#5133 = CARTESIAN_POINT ( 'NONE',  ( -14.20280369269832832, 0.000000000000000000, 12.40765738797303719 ) ) ;
#5134 = VERTEX_POINT ( 'NONE', #6901 ) ;
#5135 = DIRECTION ( 'NONE',  ( 0.007781995580012663651, 0.000000000000000000, -0.9999697198139515519 ) ) ;
#5136 = LINE ( 'NONE', #39766, #33285 ) ;
#5138 = ADVANCED_FACE ( 'NONE', ( #42917 ), #43229, .F. ) ;
#5137 = FACE_OUTER_BOUND ( 'NONE', #19379, .T. ) ;
#5139 = DIRECTION ( 'NONE',  ( 0.9932609354084158682, 0.1139014070068027351, -0.02142857142857155367 ) ) ;
#5140 = ADVANCED_FACE ( 'NONE', ( #8868 ), #42631, .F. ) ;
#5141 = CARTESIAN_POINT ( 'NONE',  ( -11.77243710274829525, -0.1191753592594197858, 11.50324088822667612 ) ) ;
#5142 = PLANE ( 'NONE',  #34197 ) ;
#5143 = LINE ( 'NONE', #43724, #1144 ) ;
#5144 = AXIS2_PLACEMENT_3D ( 'NONE', #24175, #45447, #53691 ) ;
#5145 = EDGE_LOOP ( 'NONE', ( #14642, #22516, #34299, #53745 ) ) ;
#5146 = ORIENTED_EDGE ( 'NONE', *, *, #20846, .T. ) ;
#5147 = DIRECTION ( 'NONE',  ( 0.5449076811759707706, 0.6444004775717708799, -0.5364919789714476250 ) ) ;
#5148 = PRODUCT_DEFINITION_SHAPE ( 'NONE', 'NONE',  #37453 ) ;
#5149 = CARTESIAN_POINT ( 'NONE',  ( -12.60458797795435615, 0.000000000000000000, 11.86609696750642229 ) ) ;
#5150 = VECTOR ( 'NONE', #18510, 1000.000000000000227 ) ;
#5151 = EDGE_LOOP ( 'NONE', ( #53537, #52965, #38342, #36972 ) ) ;
#5152 = LINE ( 'NONE', #48007, #10475 ) ;
#5153 = VECTOR ( 'NONE', #32017, 999.9999999999998863 ) ;
#5154 = ORIENTED_EDGE ( 'NONE', *, *, #47091, .T. ) ;
#5155 = DIRECTION ( 'NONE',  ( -0.000000000000000000, -0.000000000000000000, 1.000000000000000000 ) ) ;
#5156 = VECTOR ( 'NONE', #47930, 999.9999999999998863 ) ;
#5157 = ORIENTED_EDGE ( 'NONE', *, *, #45855, .T. ) ;
#5158 = VERTEX_POINT ( 'NONE', #51994 ) ;
#5159 = ORIENTED_EDGE ( 'NONE', *, *, #20970, .T. ) ;
#5160 = CARTESIAN_POINT ( 'NONE',  ( -8.940786546353891140, -0.1117717739994061044, 6.691278700656821066 ) ) ;
#5161 = DIRECTION ( 'NONE',  ( 0.6246952433987894571, -0.7422098413412800966, -0.2426528472758541777 ) ) ;
#5162 = DIRECTION ( 'NONE',  ( 0.6427681459581294776, -0.7660444431189769032, 0.005002170337467562802 ) ) ;
#5163 = ADVANCED_FACE ( 'NONE', ( #43480 ), #12265, .F. ) ;
#5164 = AXIS2_PLACEMENT_3D ( 'NONE', #46484, #20378, #37720 ) ;
#5165 = CARTESIAN_POINT ( 'NONE',  ( -32.65841372305263235, 0.000000000000000000, 9.367568705923016381 ) ) ;
#5166 = ORIENTED_EDGE ( 'NONE', *, *, #34783, .F. ) ;
#5167 = ORIENTED_EDGE ( 'NONE', *, *, #34885, .F. ) ;
#5168 = EDGE_CURVE ( 'NONE', #55683, #51210, #21637, .T. ) ;
#5169 = EDGE_CURVE ( 'NONE', #39497, #29979, #21044, .T. ) ;
#5170 = VECTOR ( 'NONE', #16436, 1000.000000000000227 ) ;
#5171 = VECTOR ( 'NONE', #35864, 1000.000000000000227 ) ;
#5172 = LINE ( 'NONE', #13409, #8261 ) ;
#5173 = EDGE_LOOP ( 'NONE', ( #45810, #49233, #40598, #47149 ) ) ;
#5174 = DIRECTION ( 'NONE',  ( -0.6427681459581293666, -0.7660444431189770143, -0.005002170337467561935 ) ) ;
#5175 = ORIENTED_EDGE ( 'NONE', *, *, #23296, .F. ) ;
#5176 = LINE ( 'NONE', #30727, #26944 ) ;
#5177 = DIRECTION ( 'NONE',  ( 0.000000000000000000, -0.000000000000000000, -1.000000000000000000 ) ) ;
#5178 = EDGE_LOOP ( 'NONE', ( #35111, #37001, #4562, #13465 ) ) ;
#5179 = FACE_OUTER_BOUND ( 'NONE', #52698, .T. ) ;
#5180 = EDGE_LOOP ( 'NONE', ( #26217, #26167, #30151, #24634 ) ) ;
#5181 = AXIS2_PLACEMENT_3D ( 'NONE', #40356, #22490, #13119 ) ;
#5182 = EDGE_CURVE ( 'NONE', #29996, #49857, #51709, .T. ) ;
#5183 = CARTESIAN_POINT ( 'NONE',  ( -17.74560456716937296, 0.000000000000000000, 3.774316574337878372 ) ) ;
#5184 = ORIENTED_EDGE ( 'NONE', *, *, #45461, .F. ) ;
#5185 = DIRECTION ( 'NONE',  ( 0.6427681459581294776, -0.7660444431189769032, 0.005002170337467562802 ) ) ;
#5186 = CARTESIAN_POINT ( 'NONE',  ( -15.55693048355961672, 0.000000000000000000, 7.284663983984430935 ) ) ;
#5187 = DIRECTION ( 'NONE',  ( 0.005961354470445682716, -0.6427876096865404731, -0.7660212471507180654 ) ) ;
#5188 = ORIENTED_EDGE ( 'NONE', *, *, #50318, .T. ) ;
#5189 = CARTESIAN_POINT ( 'NONE',  ( -13.72166355981337738, -1.975113310420658852, 2.148264778013123877 ) ) ;
#5190 = LINE ( 'NONE', #22505, #13819 ) ;
#5191 = AXIS2_PLACEMENT_3D ( 'NONE', #25128, #42434, #37310 ) ;
#5192 = LINE ( 'NONE', #1735, #2236 ) ;
#5193 = DIRECTION ( 'NONE',  ( -1.000000000000000000, 0.000000000000000000, 0.000000000000000000 ) ) ;
#5194 = PLANE ( 'NONE',  #31289 ) ;
#5195 = CARTESIAN_POINT ( 'NONE',  ( -24.26908309836554878, 0.000000000000000000, 6.108867788427308376 ) ) ;
#5196 = VECTOR ( 'NONE', #716, 1000.000000000000000 ) ;
#5197 = DIRECTION ( 'NONE',  ( 0.6427681459581294776, -0.7660444431189769032, 0.005002170337467562802 ) ) ;
#5198 = EDGE_LOOP ( 'NONE', ( #37033, #31982, #40882, #49241 ) ) ;
#5199 = DIRECTION ( 'NONE',  ( 0.7660212471507180654, -0.6427876096865404731, 0.005961354470445141482 ) ) ;
#5200 = DIRECTION ( 'NONE',  ( -0.5449076811759708816, 0.6444004775717707689, 0.5364919789714475140 ) ) ;
#5201 = DIRECTION ( 'NONE',  ( 0.9999697198139515519, 0.000000000000000000, 0.007781995580013368816 ) ) ;
#5202 = EDGE_LOOP ( 'NONE', ( #2056, #40033, #32232, #42776, #31641 ) ) ;
#5203 = FACE_OUTER_BOUND ( 'NONE', #55401, .T. ) ;
#5204 = CARTESIAN_POINT ( 'NONE',  ( -23.33693525117809386, 0.000000000000000000, 5.746789908705562944 ) ) ;
#5205 = ORIENTED_EDGE ( 'NONE', *, *, #9048, .F. ) ;
#5206 = DIRECTION ( 'NONE',  ( -0.5364919789714478471, 0.6444004775717705469, -0.5449076811759709926 ) ) ;
#5207 = VECTOR ( 'NONE', #11790, 999.9999999999998863 ) ;
#5208 = EDGE_CURVE ( 'NONE', #10857, #25116, #29870, .T. ) ;
#5209 = PLANE ( 'NONE',  #3966 ) ;
#5210 = DIRECTION ( 'NONE',  ( 0.6427681459581294776, -0.7660444431189769032, 0.005002170337467562802 ) ) ;
#5211 = DIRECTION ( 'NONE',  ( 0.007781995580012663651, 0.000000000000000000, -0.9999697198139515519 ) ) ;
#5212 = ORIENTED_EDGE ( 'NONE', *, *, #42571, .T. ) ;
#5213 = ORIENTED_EDGE ( 'NONE', *, *, #54497, .T. ) ;
#5214 = CARTESIAN_POINT ( 'NONE',  ( -14.00280974873554030, 0.000000000000000000, 12.40921378708904044 ) ) ;
#5215 = DIRECTION ( 'NONE',  ( 0.005002170337468016433, -0.7660444431189770143, -0.6427681459581293666 ) ) ;
#5216 = CARTESIAN_POINT ( 'NONE',  ( -66.84137242167658144, 1.999999999999978018, 6.312544413184001613 ) ) ;
#5217 = ADVANCED_FACE ( 'NONE', ( #55145 ), #16507, .F. ) ;
#5218 = LINE ( 'NONE', #48068, #53810 ) ;
#5219 = DIRECTION ( 'NONE',  ( -0.5449076811759708816, 0.6444004775717707689, 0.5364919789714475140 ) ) ;
#5220 = PLANE ( 'NONE',  #4953 ) ;
#5222 = ADVANCED_FACE ( 'NONE', ( #38377 ), #8015, .F. ) ;
#5221 = ORIENTED_EDGE ( 'NONE', *, *, #11737, .F. ) ;
#5223 = CARTESIAN_POINT ( 'NONE',  ( -11.67244013076689946, 0.000000000000000000, 11.50401908778467863 ) ) ;
#5224 = EDGE_CURVE ( 'NONE', #3767, #7042, #11960, .T. ) ;
#5225 = CARTESIAN_POINT ( 'NONE',  ( 4.848100717410752658, 0.000000000000000000, 2.061810099490657411 ) ) ;
#5226 = EDGE_LOOP ( 'NONE', ( #52178, #26962, #6543, #15584 ) ) ;
#5227 = PLANE ( 'NONE',  #265 ) ;
#5228 = EDGE_CURVE ( 'NONE', #30507, #31662, #25901, .T. ) ;
#5229 = CARTESIAN_POINT ( 'NONE',  ( -14.93495759592298988, 0.000000000000000000, 12.77129166681078409 ) ) ;
#5230 = DIRECTION ( 'NONE',  ( 0.007781995580012663651, 0.000000000000000000, -0.9999697198139515519 ) ) ;
#5231 = ORIENTED_EDGE ( 'NONE', *, *, #20545, .T. ) ;
#5232 = PLANE ( 'NONE',  #233 ) ;
#5233 = ADVANCED_FACE ( 'NONE', ( #46610 ), #3727, .F. ) ;
#5234 = ORIENTED_EDGE ( 'NONE', *, *, #27983, .T. ) ;
#5235 = EDGE_CURVE ( 'NONE', #33148, #13801, #42373, .T. ) ;
#5236 = ORIENTED_EDGE ( 'NONE', *, *, #18610, .T. ) ;
#5237 = VECTOR ( 'NONE', #26029, 999.9999999999998863 ) ;
#5238 = ORIENTED_EDGE ( 'NONE', *, *, #730, .F. ) ;
#5239 = ORIENTED_EDGE ( 'NONE', *, *, #32639, .T. ) ;
#5240 = FACE_OUTER_BOUND ( 'NONE', #8591, .T. ) ;
#5241 = EDGE_LOOP ( 'NONE', ( #47600, #15520, #23028, #38428 ) ) ;
#5242 = DIRECTION ( 'NONE',  ( -0.9983709377222389492, -0.05705673239519657575, 0.000000000000000000 ) ) ;
#5243 = DIRECTION ( 'NONE',  ( 0.007781995580012663651, -3.146120232559066537E-19, -0.9999697198139514409 ) ) ;
#5244 = EDGE_CURVE ( 'NONE', #38808, #44862, #47168, .T. ) ;
#5245 = AXIS2_PLACEMENT_3D ( 'NONE', #32677, #32965, #24179 ) ;
#5246 = ORIENTED_EDGE ( 'NONE', *, *, #5360, .T. ) ;
#5247 = LINE ( 'NONE', #39304, #54899 ) ;
#5248 = ORIENTED_EDGE ( 'NONE', *, *, #44490, .T. ) ;
#5249 = PLANE ( 'NONE',  #35628 ) ;
#5250 = ORIENTED_EDGE ( 'NONE', *, *, #21287, .F. ) ;
#5251 = EDGE_CURVE ( 'NONE', #33592, #45853, #3463, .T. ) ;
#5252 = LINE ( 'NONE', #22559, #38270 ) ;
#5253 = DIRECTION ( 'NONE',  ( -0.9999697198139514409, -0.000000000000000000, -0.007781995580013368816 ) ) ;
#5254 = FACE_OUTER_BOUND ( 'NONE', #45192, .T. ) ;
#5255 = CARTESIAN_POINT ( 'NONE',  ( -23.33849165029409889, 0.000000000000000000, 5.946783852668351855 ) ) ;
#5256 = DIRECTION ( 'NONE',  ( 0.7660212471507180654, -0.6427876096865404731, 0.005961354470445141482 ) ) ;
#5257 = LINE ( 'NONE', #31367, #18370 ) ;
#5258 = ORIENTED_EDGE ( 'NONE', *, *, #53760, .T. ) ;
#5259 = ORIENTED_EDGE ( 'NONE', *, *, #14393, .T. ) ;
#5260 = CARTESIAN_POINT ( 'NONE',  ( -12.30734625917730085, 0.000000000000000000, 7.679285069618262405 ) ) ;
#5261 = DIRECTION ( 'NONE',  ( 0.005961354470445682716, -0.6427876096865404731, -0.7660212471507180654 ) ) ;
#5262 = CARTESIAN_POINT ( 'NONE',  ( -11.87243407472968926, 0.000000000000000000, 11.50246268866867361 ) ) ;
#5263 = DIRECTION ( 'NONE',  ( 0.007781995580012662783, 0.000000000000000000, -0.9999697198139514409 ) ) ;
#5264 = EDGE_LOOP ( 'NONE', ( #3833, #43863, #8611, #53821 ) ) ;
#5265 = DIRECTION ( 'NONE',  ( -1.000000000000000000, 0.000000000000000000, 0.000000000000000000 ) ) ;
#5266 = CARTESIAN_POINT ( 'NONE',  ( -28.93060053386082231, -0.1191753592594197858, 8.019254159017428663 ) ) ;
#5267 = EDGE_LOOP ( 'NONE', ( #11711, #23640, #37389, #37561 ) ) ;
#5268 = CARTESIAN_POINT ( 'NONE',  ( -9.442067484779661513, -0.1191753592594197858, 10.59804618892231254 ) ) ;
#5269 = CARTESIAN_POINT ( 'NONE',  ( -14.63783524950929404, 0.000000000000000000, 8.599818861256533609 ) ) ;
#5270 = ORIENTED_EDGE ( 'NONE', *, *, #51039, .T. ) ;
#5271 = CARTESIAN_POINT ( 'NONE',  ( -66.83595559056652746, -8.754112661980432364, 2.678990660366957322 ) ) ;
#5272 = CARTESIAN_POINT ( 'NONE',  ( -17.44488905577733817, -5.213152330870661544, 12.01379018200878512 ) ) ;
#5273 = ADVANCED_FACE ( 'NONE', ( #25326 ), #25590, .F. ) ;
#5274 = CARTESIAN_POINT ( 'NONE',  ( -10.41431002974956321, 0.000000000000000000, 3.262032277597125773 ) ) ;
#5275 = CARTESIAN_POINT ( 'NONE',  ( -56.20083583094844926, 4.876814673940706335, 2.999999999999993339 ) ) ;
#5276 = LINE ( 'NONE', #22587, #40110 ) ;
#5277 = VERTEX_POINT ( 'NONE', #17 ) ;
#5278 = ORIENTED_EDGE ( 'NONE', *, *, #44157, .F. ) ;
#5279 = CARTESIAN_POINT ( 'NONE',  ( -10.47421230394850866, 0.000000000000000000, 10.95934586908605723 ) ) ;
#5280 = CARTESIAN_POINT ( 'NONE',  ( -15.88130887279446490, 0.000000000000000000, 3.050160814894388839 ) ) ;
#5281 = CARTESIAN_POINT ( 'NONE',  ( -19.32961685222932147, 0.000000000000000000, 14.39908572644263351 ) ) ;
#5282 = EDGE_CURVE ( 'NONE', #34792, #24768, #39210, .T. ) ;
#5283 = VECTOR ( 'NONE', #25710, 999.9999999999998863 ) ;
#5284 = FACE_OUTER_BOUND ( 'NONE', #10109, .T. ) ;
#5285 = DIRECTION ( 'NONE',  ( 0.5364919789714477361, 0.6444004775717706579, 0.5449076811759711036 ) ) ;
#5286 = ORIENTED_EDGE ( 'NONE', *, *, #44268, .F. ) ;
#5287 = LINE ( 'NONE', #40490, #9244 ) ;
#5288 = LINE ( 'NONE', #43350, #12062 ) ;
#5289 = EDGE_CURVE ( 'NONE', #25391, #40382, #30966, .T. ) ;
#5290 = PLANE ( 'NONE',  #18715 ) ;
#5291 = DIRECTION ( 'NONE',  ( -0.005961354470445682716, -0.6427876096865404731, 0.7660212471507180654 ) ) ;
#5292 = VERTEX_POINT ( 'NONE', #22183 ) ;
#5293 = FACE_OUTER_BOUND ( 'NONE', #53876, .T. ) ;
#5294 = EDGE_LOOP ( 'NONE', ( #32492, #21844, #14852, #50467 ) ) ;
#5295 = DIRECTION ( 'NONE',  ( 0.5449076811759707706, 0.6444004775717708799, -0.5364919789714476250 ) ) ;
#5296 = DIRECTION ( 'NONE',  ( -0.005961354470445682716, -0.6427876096865404731, 0.7660212471507180654 ) ) ;
#5297 = ORIENTED_EDGE ( 'NONE', *, *, #29418, .F. ) ;
#5298 = LINE ( 'NONE', #22610, #52621 ) ;
#5299 = EDGE_CURVE ( 'NONE', #36106, #1914, #31562, .T. ) ;
#5300 = ORIENTED_EDGE ( 'NONE', *, *, #21017, .T. ) ;
#5301 = ADVANCED_FACE ( 'NONE', ( #40343 ), #44586, .F. ) ;
#5302 = ORIENTED_EDGE ( 'NONE', *, *, #44378, .T. ) ;
#5303 = ORIENTED_EDGE ( 'NONE', *, *, #17504, .F. ) ;
#5304 = CARTESIAN_POINT ( 'NONE',  ( -27.99845268667336384, -0.1191753592594197858, 7.657176279295684118 ) ) ;
#5305 = VERTEX_POINT ( 'NONE', #14505 ) ;
#5306 = ORIENTED_EDGE ( 'NONE', *, *, #46940, .T. ) ;
#5307 = CARTESIAN_POINT ( 'NONE',  ( -19.42910703681909368, 21.15220053346460816, -4.255330291692488665 ) ) ;
#5308 = DIRECTION ( 'NONE',  ( 0.5364919789714477361, 0.6444004775717706579, 0.5449076811759711036 ) ) ;
#5309 = VERTEX_POINT ( 'NONE', #10240 ) ;
#5310 = ADVANCED_FACE ( 'NONE', ( #35518 ), #34984, .F. ) ;
#5311 = ORIENTED_EDGE ( 'NONE', *, *, #38030, .F. ) ;
#5312 = FACE_OUTER_BOUND ( 'NONE', #23302, .T. ) ;
#5313 = ORIENTED_EDGE ( 'NONE', *, *, #47830, .F. ) ;
#5314 = EDGE_LOOP ( 'NONE', ( #28668, #49703, #13798, #28861 ) ) ;
#5315 = ADVANCED_FACE ( 'NONE', ( #9399 ), #48588, .F. ) ;
#5316 = DIRECTION ( 'NONE',  ( 0.5364919789714477361, 0.6444004775717706579, 0.5449076811759711036 ) ) ;
#5317 = DIRECTION ( 'NONE',  ( 0.000000000000000000, -0.000000000000000000, -1.000000000000000000 ) ) ;
#5318 = FACE_OUTER_BOUND ( 'NONE', #10834, .T. ) ;
#5319 = CARTESIAN_POINT ( 'NONE',  ( -21.29465867747552110, 2.391131607591507446, 9.077144048833369894 ) ) ;
#5320 = ORIENTED_EDGE ( 'NONE', *, *, #13526, .F. ) ;
#5321 = LINE ( 'NONE', #44221, #11950 ) ;
#5322 = ORIENTED_EDGE ( 'NONE', *, *, #40791, .F. ) ;
#5323 = VECTOR ( 'NONE', #24870, 999.9999999999998863 ) ;
#5324 = PLANE ( 'NONE',  #38401 ) ;
#5325 = DIRECTION ( 'NONE',  ( 0.000000000000000000, -1.000000000000000000, 0.000000000000000000 ) ) ;
#5326 = CARTESIAN_POINT ( 'NONE',  ( -14.10280672071693431, -0.1191753592594197858, 12.40843558753103792 ) ) ;
#5327 = DIRECTION ( 'NONE',  ( -0.9999697198139514409, -0.000000000000000000, -0.007781995580013368816 ) ) ;
#5328 = LINE ( 'NONE', #43637, #33968 ) ;
#5329 = CARTESIAN_POINT ( 'NONE',  ( -6.132980432523989833, 5.992972315187304666, 5.600631452548297418 ) ) ;
#5330 = CARTESIAN_POINT ( 'NONE',  ( -13.11153479888853468, -0.1191753592594190225, 4.449041088301757263 ) ) ;
#5331 = VERTEX_POINT ( 'NONE', #35816 ) ;
#5332 = LINE ( 'NONE', #27757, #22004 ) ;
#5333 = EDGE_CURVE ( 'NONE', #50963, #24424, #26717, .T. ) ;
#5334 = DIRECTION ( 'NONE',  ( 0.9999697198139515519, 0.000000000000000000, 0.007781995580013368816 ) ) ;
#5335 = PLANE ( 'NONE',  #52289 ) ;
#5336 = LINE ( 'NONE', #14967, #19062 ) ;
#5337 = EDGE_CURVE ( 'NONE', #21088, #41034, #613, .T. ) ;
#5338 = CARTESIAN_POINT ( 'NONE',  ( -19.68509517508318751, 19.56103003995438883, -4.315923200200658449 ) ) ;
#5339 = DIRECTION ( 'NONE',  ( -0.5364919789714478471, 0.6444004775717705469, -0.5449076811759709926 ) ) ;
#5340 = LINE ( 'NONE', #22084, #45891 ) ;
#5341 = CARTESIAN_POINT ( 'NONE',  ( -17.54698502803930893, -4.241740624735659715, 10.45919562112636747 ) ) ;
#5342 = ADVANCED_FACE ( 'NONE', ( #14249 ), #23027, .F. ) ;
#5343 = VERTEX_POINT ( 'NONE', #35262 ) ;
#5344 = EDGE_CURVE ( 'NONE', #20170, #13159, #52556, .T. ) ;
#5345 = DIRECTION ( 'NONE',  ( -0.5364919789714478471, 0.6444004775717705469, -0.5449076811759709926 ) ) ;
#5346 = DIRECTION ( 'NONE',  ( 0.000000000000000000, -1.000000000000000000, 0.000000000000000000 ) ) ;
#5347 = DIRECTION ( 'NONE',  ( -0.7660212471507179544, -0.6427876096865405842, -0.005961354470445141482 ) ) ;
#5348 = EDGE_CURVE ( 'NONE', #41657, #34394, #30719, .T. ) ;
#5349 = EDGE_CURVE ( 'NONE', #55849, #12500, #48022, .T. ) ;
#5350 = EDGE_CURVE ( 'NONE', #16795, #25477, #26429, .T. ) ;
#5351 = CARTESIAN_POINT ( 'NONE',  ( -67.50702643244157741, 2.000000000000000000, -7.448289400635801805 ) ) ;
#5352 = CARTESIAN_POINT ( 'NONE',  ( -9.300968958747018789, 0.000000000000000000, 5.317362960500759961 ) ) ;
#5353 = DIRECTION ( 'NONE',  ( 0.007781995580012663651, 0.000000000000000000, -0.9999697198139515519 ) ) ;
#5354 = CARTESIAN_POINT ( 'NONE',  ( -16.81267852042391198, -0.1191753592594197858, 3.312241722634738039 ) ) ;
#5355 = FACE_OUTER_BOUND ( 'NONE', #8662, .T. ) ;
#5356 = DIRECTION ( 'NONE',  ( 0.5364919789714477361, 0.6444004775717706579, 0.5449076811759711036 ) ) ;
#5357 = VECTOR ( 'NONE', #6039, 1000.000000000000227 ) ;
#5358 = ORIENTED_EDGE ( 'NONE', *, *, #46368, .F. ) ;
#5359 = EDGE_CURVE ( 'NONE', #22392, #11173, #52824, .T. ) ;
#5360 = EDGE_CURVE ( 'NONE', #32296, #33683, #13936, .T. ) ;
#5361 = ORIENTED_EDGE ( 'NONE', *, *, #31135, .F. ) ;
#5362 = ORIENTED_EDGE ( 'NONE', *, *, #34330, .T. ) ;
#5363 = ORIENTED_EDGE ( 'NONE', *, *, #38203, .F. ) ;
#5364 = ADVANCED_FACE ( 'NONE', ( #18786 ), #31262, .F. ) ;
#5365 = ORIENTED_EDGE ( 'NONE', *, *, #12607, .T. ) ;
#5366 = CARTESIAN_POINT ( 'NONE',  ( -16.76234344414121580, 0.000000000000000000, 8.752611460827463219 ) ) ;
#5367 = DIRECTION ( 'NONE',  ( 0.7660212471507180654, -0.6427876096865404731, 0.005961354470445141482 ) ) ;
#5368 = EDGE_CURVE ( 'NONE', #50886, #40382, #18474, .T. ) ;
#5369 = ORIENTED_EDGE ( 'NONE', *, *, #31371, .F. ) ;
#5370 = VERTEX_POINT ( 'NONE', #7581 ) ;
#5371 = FACE_OUTER_BOUND ( 'NONE', #49986, .T. ) ;
#5372 = ORIENTED_EDGE ( 'NONE', *, *, #44379, .F. ) ;
#5373 = FACE_OUTER_BOUND ( 'NONE', #42581, .T. ) ;
#5374 = CARTESIAN_POINT ( 'NONE',  ( -15.35639454250681801, -3.917936722690662954, 2.721263568740423189 ) ) ;
#5375 = VERTEX_POINT ( 'NONE', #55553 ) ;
#5376 = DIRECTION ( 'NONE',  ( 0.005002170337468016433, -0.7660444431189770143, -0.6427681459581293666 ) ) ;
#5377 = ORIENTED_EDGE ( 'NONE', *, *, #35224, .F. ) ;
#5378 = CARTESIAN_POINT ( 'NONE',  ( 2.072287782118878319, 0.000000000000000000, -2.950529333540147015 ) ) ;
#5379 = DIRECTION ( 'NONE',  ( -0.3620778797217456546, 0.000000000000000000, -0.9321478471874540261 ) ) ;
#5380 = CARTESIAN_POINT ( 'NONE',  ( -20.75985484760730060, 4.010151117816511679, 4.617819545835347483 ) ) ;
#5381 = CARTESIAN_POINT ( 'NONE',  ( -17.74560456716937296, 0.000000000000000000, 3.774316574337878372 ) ) ;
#5382 = ORIENTED_EDGE ( 'NONE', *, *, #29011, .T. ) ;
#5383 = CARTESIAN_POINT ( 'NONE',  ( -11.97215022127920392, -1.003701604285657911, 1.499687502927729010 ) ) ;
#5384 = CARTESIAN_POINT ( 'NONE',  ( -9.298094905241734764, 0.000000000000000000, 4.948053257242996494 ) ) ;
#5385 = DIRECTION ( 'NONE',  ( 0.7660212471507180654, -0.6427876096865404731, 0.005961354470445141482 ) ) ;
#5386 = ORIENTED_EDGE ( 'NONE', *, *, #6314, .F. ) ;
#5387 = DIRECTION ( 'NONE',  ( 0.5364919789714477361, 0.6444004775717706579, 0.5449076811759711036 ) ) ;
#5388 = ORIENTED_EDGE ( 'NONE', *, *, #28680, .F. ) ;
#5389 = PRESENTATION_LAYER_ASSIGNMENT (  '', '', ( #10817 ) ) ;
#5390 = DIRECTION ( 'NONE',  ( -0.5364919789714478471, 0.6444004775717705469, -0.5449076811759709926 ) ) ;
#5391 = FACE_OUTER_BOUND ( 'NONE', #5553, .T. ) ;
#5392 = CARTESIAN_POINT ( 'NONE',  ( -23.33771345073609638, -0.1191753592594197858, 5.846786880686956955 ) ) ;
#5393 = CARTESIAN_POINT ( 'NONE',  ( -16.33317936670417225, 0.000000000000000000, 13.31440848639340224 ) ) ;
#5394 = PLANE ( 'NONE',  #55846 ) ;
#5395 = DIRECTION ( 'NONE',  ( -0.005002170337468016433, -0.7660444431189770143, 0.6427681459581293666 ) ) ;
#5396 = DIRECTION ( 'NONE',  ( 0.6427681459581294776, -0.7660444431189769032, 0.005002170337467562802 ) ) ;
#5397 = DIRECTION ( 'NONE',  ( -0.005002170337468016433, -0.7660444431189770143, 0.6427681459581293666 ) ) ;
#5398 =( NAMED_UNIT ( * ) SI_UNIT ( $, .STERADIAN. ) SOLID_ANGLE_UNIT ( ) );
#5399 = LINE ( 'NONE', #22708, #27806 ) ;
#5400 = EDGE_LOOP ( 'NONE', ( #6954, #33903, #48942, #54106 ) ) ;
#5401 = DIRECTION ( 'NONE',  ( 0.007781995580012663651, 0.000000000000000000, -0.9999697198139515519 ) ) ;
#5402 = DIRECTION ( 'NONE',  ( 0.007781995580012663651, 0.000000000000000000, -0.9999697198139515519 ) ) ;
#5403 = PLANE ( 'NONE',  #35410 ) ;
#5404 = DIRECTION ( 'NONE',  ( -0.5364919789714478471, 0.6444004775717705469, -0.5449076811759709926 ) ) ;
#5405 = EDGE_CURVE ( 'NONE', #47531, #51306, #16660, .T. ) ;
#5406 = EDGE_CURVE ( 'NONE', #6150, #27710, #3336, .T. ) ;
#5407 = DIRECTION ( 'NONE',  ( 0.9999697198139515519, 0.000000000000000000, 0.007781995580013368816 ) ) ;
#5408 = EDGE_CURVE ( 'NONE', #18340, #54304, #11829, .T. ) ;
#5409 = FACE_OUTER_BOUND ( 'NONE', #3659, .T. ) ;
#5410 = DIRECTION ( 'NONE',  ( 0.6427681459581294776, -0.7660444431189769032, 0.005002170337467562802 ) ) ;
#5411 = ORIENTED_EDGE ( 'NONE', *, *, #47305, .T. ) ;
#5412 = VERTEX_POINT ( 'NONE', #32854 ) ;
#5413 = DIRECTION ( 'NONE',  ( 0.9997703818010067467, 0.000000000000000000, 0.02142857142857158143 ) ) ;
#5414 = CARTESIAN_POINT ( 'NONE',  ( -15.13495153988577968, 0.000000000000000000, 12.76973526769478084 ) ) ;
#5415 = ORIENTED_EDGE ( 'NONE', *, *, #19914, .F. ) ;
#5416 = DIRECTION ( 'NONE',  ( -0.005961354470445682716, -0.6427876096865404731, 0.7660212471507180654 ) ) ;
#5417 = ORIENTED_EDGE ( 'NONE', *, *, #22124, .T. ) ;
#5418 = DIRECTION ( 'NONE',  ( 0.3313982828793700097, 0.4028455766673916805, 0.8531650599175528704 ) ) ;
#5419 = EDGE_CURVE ( 'NONE', #26758, #9638, #20656, .T. ) ;
#5420 = ORIENTED_EDGE ( 'NONE', *, *, #22951, .T. ) ;
#5421 = ORIENTED_EDGE ( 'NONE', *, *, #52601, .F. ) ;
#5422 = ORIENTED_EDGE ( 'NONE', *, *, #3492, .T. ) ;
#5423 = EDGE_CURVE ( 'NONE', #11807, #36151, #4836, .T. ) ;
#5424 = CARTESIAN_POINT ( 'NONE',  ( -10.74029228357944987, 0.000000000000000000, 11.14194120806293320 ) ) ;
#5425 = CARTESIAN_POINT ( 'NONE',  ( -13.53673582514181106, 0.000000000000000000, 12.22817484722816772 ) ) ;
#5426 = DIRECTION ( 'NONE',  ( -0.7660212471507179544, -0.6427876096865405842, -0.005961354470445141482 ) ) ;
#5427 = EDGE_CURVE ( 'NONE', #33190, #36986, #24907, .T. ) ;
#5428 = CARTESIAN_POINT ( 'NONE',  ( -26.13493519185646008, 0.000000000000000000, 7.033017491833586377 ) ) ;
#5429 = ORIENTED_EDGE ( 'NONE', *, *, #4088, .F. ) ;
#5430 = ORIENTED_EDGE ( 'NONE', *, *, #54776, .F. ) ;
#5431 = ADVANCED_FACE ( 'NONE', ( #55278 ), #16112, .F. ) ;
#5432 = CARTESIAN_POINT ( 'NONE',  ( -68.54375487892276908, -9.299823415457391107, -7.481591365497658686 ) ) ;
#5433 = ORIENTED_EDGE ( 'NONE', *, *, #55489, .T. ) ;
#5434 = CARTESIAN_POINT ( 'NONE',  ( -18.67775241435682432, 0.000000000000000000, 4.136394454059623804 ) ) ;
#5435 = ORIENTED_EDGE ( 'NONE', *, *, #29401, .T. ) ;
#5436 = CARTESIAN_POINT ( 'NONE',  ( -15.20077793328688820, 0.000000000000000000, 2.686124794216351308 ) ) ;
#5437 = PLANE ( 'NONE',  #20353 ) ;
#5438 = ORIENTED_EDGE ( 'NONE', *, *, #53652, .T. ) ;
#5439 = LINE ( 'NONE', #27286, #3231 ) ;
#5440 = EDGE_LOOP ( 'NONE', ( #39725, #46621, #23708, #19308 ) ) ;
#5441 = CARTESIAN_POINT ( 'NONE',  ( -17.18728735815524544, 3.038739411681508518, 8.544536277294087157 ) ) ;
#5442 = ORIENTED_EDGE ( 'NONE', *, *, #18135, .F. ) ;
#5443 = DIRECTION ( 'NONE',  ( -0.7660212471507179544, -0.6427876096865405842, -0.005961354470445141482 ) ) ;
#5444 = CARTESIAN_POINT ( 'NONE',  ( -15.88130887279446490, 0.000000000000000000, 3.050160814894388839 ) ) ;
#5445 = CARTESIAN_POINT ( 'NONE',  ( -16.79925329029790149, 0.000000000000000000, 13.49544742625427496 ) ) ;
#5446 = EDGE_LOOP ( 'NONE', ( #45412, #6756, #35669, #45940 ) ) ;
#5447 = LINE ( 'NONE', #40661, #3803 ) ;
#5448 = LINE ( 'NONE', #23054, #31271 ) ;
#5449 = CARTESIAN_POINT ( 'NONE',  ( -15.52399824061222589, 0.000000000000000000, 3.052941488854047591 ) ) ;
#5450 = CARTESIAN_POINT ( 'NONE',  ( -21.47419595591918906, 0.000000000000000000, 5.222628093224860102 ) ) ;
#5451 = LINE ( 'NONE', #898, #36094 ) ;
#5452 = VECTOR ( 'NONE', #49321, 1000.000000000000114 ) ;
#5453 = CARTESIAN_POINT ( 'NONE',  ( -64.66143966744172644, -11.12270517324659735, 1.620203490756831677 ) ) ;
#5454 = ORIENTED_EDGE ( 'NONE', *, *, #49173, .F. ) ;
#5455 = LINE ( 'NONE', #27600, #9866 ) ;
#5456 = DIRECTION ( 'NONE',  ( -0.5449076811759708816, 0.6444004775717707689, 0.5364919789714475140 ) ) ;
#5457 = CARTESIAN_POINT ( 'NONE',  ( -9.485036236067394100, 0.000000000000000000, 3.269264101133144695 ) ) ;
#5458 = ORIENTED_EDGE ( 'NONE', *, *, #44379, .T. ) ;
#5459 = DIRECTION ( 'NONE',  ( 0.6427681459581294776, -0.7660444431189769032, 0.005002170337467562802 ) ) ;
#5460 = CARTESIAN_POINT ( 'NONE',  ( -16.06709938707323460, 0.000000000000000000, 13.13181314741652628 ) ) ;
#5461 = EDGE_LOOP ( 'NONE', ( #977, #16102, #10393, #24899 ) ) ;
#5462 = ADVANCED_FACE ( 'NONE', ( #28893 ), #12430, .F. ) ;
#5463 = FACE_OUTER_BOUND ( 'NONE', #27212, .T. ) ;
#5464 = CARTESIAN_POINT ( 'NONE',  ( -11.12303075984975109, 1.419719901456505617, 0.9571981204249864206 ) ) ;
#5465 = EDGE_CURVE ( 'NONE', #9189, #4538, #41921, .T. ) ;
#5466 = EDGE_CURVE ( 'NONE', #39497, #1446, #47049, .T. ) ;
#5467 = CARTESIAN_POINT ( 'NONE',  ( -14.46888367232926420, 0.000000000000000000, 12.59025272694991315 ) ) ;
#5468 = DIRECTION ( 'NONE',  ( 0.005961354470445682716, -0.6427876096865404731, -0.7660212471507180654 ) ) ;
#5469 = ORIENTED_EDGE ( 'NONE', *, *, #8754, .F. ) ;
#5470 = ORIENTED_EDGE ( 'NONE', *, *, #35942, .T. ) ;
#5471 = CARTESIAN_POINT ( 'NONE',  ( -20.44450923172429668, 1.419719901456506728, 4.577976917642439858 ) ) ;
#5472 = CARTESIAN_POINT ( 'NONE',  ( -20.54126990917373874, -0.1191753592594138877, 4.760553241521714440 ) ) ;
#5473 = DIRECTION ( 'NONE',  ( 0.007781995580012663651, -3.146120232559066537E-19, -0.9999697198139514409 ) ) ;
#5474 = DIRECTION ( 'NONE',  ( 0.005002170337468016433, -0.7660444431189770143, -0.6427681459581293666 ) ) ;
#5475 = PLANE ( 'NONE',  #28315 ) ;
#5476 = PLANE ( 'NONE',  #51195 ) ;
#5477 = ORIENTED_EDGE ( 'NONE', *, *, #55930, .F. ) ;
#5478 = DIRECTION ( 'NONE',  ( 0.7660212471507180654, -0.6427876096865404731, 0.005961354470445141482 ) ) ;
#5479 = DIRECTION ( 'NONE',  ( 0.005961354470445682716, -0.6427876096865404731, -0.7660212471507180654 ) ) ;
#5480 = ORIENTED_EDGE ( 'NONE', *, *, #21309, .F. ) ;
#5481 = DIRECTION ( 'NONE',  ( 0.005002170337468016433, -0.7660444431189770143, -0.6427681459581293666 ) ) ;
#5482 = LINE ( 'NONE', #47826, #24081 ) ;
#5483 = LINE ( 'NONE', #40118, #49284 ) ;
#5484 = ORIENTED_EDGE ( 'NONE', *, *, #29952, .F. ) ;
#5485 = DIRECTION ( 'NONE',  ( -0.6427681459581293666, -0.7660444431189770143, -0.005002170337467561935 ) ) ;
#5486 = ORIENTED_EDGE ( 'NONE', *, *, #30197, .T. ) ;
#5487 = EDGE_CURVE ( 'NONE', #46187, #40733, #46772, .T. ) ;
#5488 = AXIS2_PLACEMENT_3D ( 'NONE', #48906, #33955, #22229 ) ;
#5489 = EDGE_LOOP ( 'NONE', ( #39206, #54488 ) ) ;
#5490 = VERTEX_POINT ( 'NONE', #50476 ) ;
#5491 = ADVANCED_FACE ( 'NONE', ( #55019 ), #3602, .F. ) ;
#5492 = EDGE_LOOP ( 'NONE', ( #11348, #53541, #24500, #55607 ) ) ;
#5493 = PLANE ( 'NONE',  #32091 ) ;
#5494 = EDGE_CURVE ( 'NONE', #52808, #44596, #2487, .T. ) ;
#5495 = ORIENTED_EDGE ( 'NONE', *, *, #35313, .F. ) ;
#5496 = DIRECTION ( 'NONE',  ( -0.7660212471507179544, -0.6427876096865405842, -0.005961354470445141482 ) ) ;
#5497 = CARTESIAN_POINT ( 'NONE',  ( -23.33849165029409889, 0.000000000000000000, 5.946783852668351855 ) ) ;
#5498 = EDGE_LOOP ( 'NONE', ( #34651, #3347, #4109, #3386 ) ) ;
#5499 = CARTESIAN_POINT ( 'NONE',  ( -15.73389624039720580, 0.000000000000000000, 9.329953200799501190 ) ) ;
#5500 = EDGE_CURVE ( 'NONE', #21894, #4790, #2734, .T. ) ;
#5501 = VERTEX_POINT ( 'NONE', #11278 ) ;
#5502 = DIRECTION ( 'NONE',  ( 0.9999697198139515519, 0.000000000000000000, 0.007781995580013368816 ) ) ;
#5503 = VERTEX_POINT ( 'NONE', #28610 ) ;
#5504 = DIRECTION ( 'NONE',  ( 0.005961354470445682716, -0.6427876096865404731, -0.7660212471507180654 ) ) ;
#5505 = PLANE ( 'NONE',  #25678 ) ;
#5506 = LINE ( 'NONE', #44145, #23236 ) ;
#5507 = DIRECTION ( 'NONE',  ( 0.9999697198139515519, 0.000000000000000000, 0.007781995580013368816 ) ) ;
#5508 = DIRECTION ( 'NONE',  ( 0.005961354470445682716, -0.6427876096865404731, -0.7660212471507180654 ) ) ;
#5509 = PRESENTATION_STYLE_ASSIGNMENT (( #48956 ) ) ;
#5510 = ORIENTED_EDGE ( 'NONE', *, *, #1356, .F. ) ;
#5511 = ORIENTED_EDGE ( 'NONE', *, *, #51380, .T. ) ;
#5512 = AXIS2_PLACEMENT_3D ( 'NONE', #10734, #41384, #11562 ) ;
#5513 = PLANE ( 'NONE',  #20984 ) ;
#5514 = LINE ( 'NONE', #40730, #34852 ) ;
#5515 = EDGE_CURVE ( 'NONE', #6270, #24207, #45935, .T. ) ;
#5516 = DIRECTION ( 'NONE',  ( 0.5449076811759707706, 0.6444004775717708799, -0.5364919789714476250 ) ) ;
#5517 = CARTESIAN_POINT ( 'NONE',  ( -18.67619601524082285, 0.000000000000000000, 3.936400510096834893 ) ) ;
#5518 = ORIENTED_EDGE ( 'NONE', *, *, #28799, .F. ) ;
#5519 = DIRECTION ( 'NONE',  ( -0.6427681459581293666, -0.7660444431189770143, -0.005002170337467561935 ) ) ;
#5520 = CARTESIAN_POINT ( 'NONE',  ( -15.88130887279446490, 0.000000000000000000, 3.050160814894388839 ) ) ;
#5521 = ORIENTED_EDGE ( 'NONE', *, *, #30632, .T. ) ;
#5522 = FACE_OUTER_BOUND ( 'NONE', #43462, .T. ) ;
#5523 = EDGE_CURVE ( 'NONE', #26368, #6316, #41649, .T. ) ;
#5524 = LINE ( 'NONE', #31387, #11328 ) ;
#5525 = ORIENTED_EDGE ( 'NONE', *, *, #46707, .T. ) ;
#5526 = DIRECTION ( 'NONE',  ( 0.007781995580012663651, -3.146120232559066537E-19, -0.9999697198139514409 ) ) ;
#5527 = DIRECTION ( 'NONE',  ( 0.5449076811759707706, 0.6444004775717708799, -0.5364919789714476250 ) ) ;
#5528 = AXIS2_PLACEMENT_3D ( 'NONE', #19623, #54255, #28405 ) ;
#5529 = EDGE_CURVE ( 'NONE', #5490, #52907, #7291, .T. ) ;
#5530 = CARTESIAN_POINT ( 'NONE',  ( -13.07066190154808361, 0.000000000000000000, 12.04713590736729678 ) ) ;
#5531 = EDGE_CURVE ( 'NONE', #42246, #41830, #38523, .T. ) ;
#5532 = CARTESIAN_POINT ( 'NONE',  ( 2.072287782118878319, 0.000000000000000000, -2.950529333540147015 ) ) ;
#5533 = VECTOR ( 'NONE', #3641, 999.9999999999998863 ) ;
#5534 = LINE ( 'NONE', #31671, #6587 ) ;
#5535 = VERTEX_POINT ( 'NONE', #21769 ) ;
#5536 = ORIENTED_EDGE ( 'NONE', *, *, #51283, .F. ) ;
#5537 = DIRECTION ( 'NONE',  ( -0.005961354470445682716, -0.6427876096865404731, 0.7660212471507180654 ) ) ;
#5538 = PLANE ( 'NONE',  #9554 ) ;
#5539 = DIRECTION ( 'NONE',  ( -0.6427681459581293666, -0.7660444431189770143, -0.005002170337467561935 ) ) ;
#5540 = CARTESIAN_POINT ( 'NONE',  ( -15.89935617993504913, -0.1191753592594213540, 4.427345617693702273 ) ) ;
#5541 = CARTESIAN_POINT ( 'NONE',  ( -12.13851405436063047, 0.000000000000000000, 11.68505802764555135 ) ) ;
#5542 = ORIENTED_EDGE ( 'NONE', *, *, #47970, .T. ) ;
#5543 = CARTESIAN_POINT ( 'NONE',  ( -14.23203706048740713, 24.44140541789180787, -3.724779944465314241 ) ) ;
#5544 = DIRECTION ( 'NONE',  ( 0.005002170337468016433, -0.7660444431189770143, -0.6427681459581293666 ) ) ;
#5545 = EDGE_CURVE ( 'NONE', #7363, #29459, #30847, .T. ) ;
#5546 = PLANE ( 'NONE',  #23255 ) ;
#5547 = CARTESIAN_POINT ( 'NONE',  ( -20.39013098992649020, 20.88602823003513365, -4.312947112340340006 ) ) ;
#5548 = EDGE_LOOP ( 'NONE', ( #13659, #55595, #11651, #54303 ) ) ;
#5549 = DIRECTION ( 'NONE',  ( 0.3313982828793700097, 0.4028455766673915694, 0.8531650599175529814 ) ) ;
#5550 = ORIENTED_EDGE ( 'NONE', *, *, #2270, .F. ) ;
#5551 = DIRECTION ( 'NONE',  ( -0.6427681459581293666, -0.7660444431189770143, -0.005002170337467561935 ) ) ;
#5552 = CARTESIAN_POINT ( 'NONE',  ( -19.60834386242827776, 0.000000000000000000, 4.298478389818581213 ) ) ;
#5553 = EDGE_LOOP ( 'NONE', ( #27049, #14418, #43549, #2197 ) ) ;
#5554 = AXIS2_PLACEMENT_3D ( 'NONE', #20105, #46823, #16154 ) ;
#5555 = AXIS2_PLACEMENT_3D ( 'NONE', #7309, #55037, #45647 ) ;
#5556 = CARTESIAN_POINT ( 'NONE',  ( -10.37421533196711465, -0.1191753592594197858, 10.96012406864405975 ) ) ;
#5557 = ORIENTED_EDGE ( 'NONE', *, *, #22662, .T. ) ;
#5558 = ORIENTED_EDGE ( 'NONE', *, *, #23447, .T. ) ;
#5559 = ORIENTED_EDGE ( 'NONE', *, *, #27794, .T. ) ;
#5560 = CARTESIAN_POINT ( 'NONE',  ( -38.30474801573077315, 10.54301926775796439, 4.960515765732081306 ) ) ;
#5561 = ORIENTED_EDGE ( 'NONE', *, *, #53550, .F. ) ;
#5562 = ORIENTED_EDGE ( 'NONE', *, *, #20447, .F. ) ;
#5563 = DIRECTION ( 'NONE',  ( 0.000000000000000000, -0.000000000000000000, -1.000000000000000000 ) ) ;
#5564 = DIRECTION ( 'NONE',  ( 0.5364919789714477361, 0.6444004775717706579, 0.5449076811759711036 ) ) ;
#5565 = ORIENTED_EDGE ( 'NONE', *, *, #23424, .T. ) ;
#5566 = ORIENTED_EDGE ( 'NONE', *, *, #46147, .T. ) ;
#5567 = DIRECTION ( 'NONE',  ( -0.5449076811759708816, 0.6444004775717707689, 0.5364919789714475140 ) ) ;
#5568 = ADVANCED_FACE ( 'NONE', ( #56134 ), #38825, .F. ) ;
#5569 = ORIENTED_EDGE ( 'NONE', *, *, #23443, .F. ) ;
#5570 = VERTEX_POINT ( 'NONE', #4185 ) ;
#5571 = VECTOR ( 'NONE', #16742, 999.9999999999998863 ) ;
#5572 = DIRECTION ( 'NONE',  ( 0.7660212471507180654, -0.6427876096865404731, 0.005961354470445141482 ) ) ;
#5573 = DIRECTION ( 'NONE',  ( 0.7660212471507180654, -0.6427876096865404731, 0.005961354470445141482 ) ) ;
#5574 = CARTESIAN_POINT ( 'NONE',  ( -11.73486842939697006, -0.1191753592594185784, 6.675747043152371774 ) ) ;
#5575 = PLANE ( 'NONE',  #23242 ) ;
#5576 = ORIENTED_EDGE ( 'NONE', *, *, #36228, .F. ) ;
#5577 = DIRECTION ( 'NONE',  ( -0.9999697198139514409, -0.000000000000000000, -0.007781995580013368816 ) ) ;
#5578 = ORIENTED_EDGE ( 'NONE', *, *, #31690, .T. ) ;
#5579 = EDGE_CURVE ( 'NONE', #12964, #18005, #51852, .T. ) ;
#5580 = DIRECTION ( 'NONE',  ( 0.5364919789714477361, 0.6444004775717706579, 0.5449076811759711036 ) ) ;
#5581 = EDGE_CURVE ( 'NONE', #19391, #51083, #12691, .T. ) ;
#5582 = ADVANCED_FACE ( 'NONE', ( #34540 ), #4462, .F. ) ;
#5583 = DIRECTION ( 'NONE',  ( -0.6427681459581293666, -0.7660444431189770143, -0.005002170337467561935 ) ) ;
#5584 = DIRECTION ( 'NONE',  ( 0.007781995580012663651, 0.000000000000000000, -0.9999697198139515519 ) ) ;
#5585 = CARTESIAN_POINT ( 'NONE',  ( -14.66887761629205222, 0.000000000000000000, 12.58869632783390990 ) ) ;
#5586 = DIRECTION ( 'NONE',  ( 0.5364919789714477361, 0.6444004775717706579, 0.5449076811759711036 ) ) ;
#5587 = LINE ( 'NONE', #36266, #48586 ) ;
#5588 = ORIENTED_EDGE ( 'NONE', *, *, #53311, .F. ) ;
#5589 = PLANE ( 'NONE',  #40164 ) ;
#5590 = EDGE_CURVE ( 'NONE', #13391, #30427, #47314, .T. ) ;
#5591 = ORIENTED_EDGE ( 'NONE', *, *, #52151, .F. ) ;
#5592 = VECTOR ( 'NONE', #35722, 1000.000000000000000 ) ;
#5593 = AXIS2_PLACEMENT_3D ( 'NONE', #23122, #53755, #37021 ) ;
#5594 = CARTESIAN_POINT ( 'NONE',  ( -9.110551994824897193, 0.000000000000000000, 3.538847790438064411 ) ) ;
#5595 = LINE ( 'NONE', #22919, #39616 ) ;
#5596 = EDGE_CURVE ( 'NONE', #30427, #10301, #18069, .T. ) ;
#5597 = LINE ( 'NONE', #40548, #49871 ) ;
#5598 = LINE ( 'NONE', #48481, #486 ) ;
#5599 = ADVANCED_FACE ( 'NONE', ( #13533 ), #31122, .F. ) ;
#5600 = CARTESIAN_POINT ( 'NONE',  ( -16.89084389517911688, -4.079838673713163111, 3.312130287550314911 ) ) ;
#5601 = CARTESIAN_POINT ( 'NONE',  ( -69.18604761972393646, -0.9999999999995238253, 6.394134653913046584 ) ) ;
#5602 = VECTOR ( 'NONE', #33868, 1000.000000000000227 ) ;
#5603 = ORIENTED_EDGE ( 'NONE', *, *, #22061, .T. ) ;
#5604 = CARTESIAN_POINT ( 'NONE',  ( -45.77156441860526570, 4.499999999999973355, 5.000000000000000000 ) ) ;
#5605 = DIRECTION ( 'NONE',  ( 0.005002170337468016433, -0.7660444431189770143, -0.6427681459581293666 ) ) ;
#5606 = CARTESIAN_POINT ( 'NONE',  ( -13.08330893211609869, 0.000000000000000000, 1.763933231766363630 ) ) ;
#5607 = EDGE_CURVE ( 'NONE', #17276, #904, #43902, .T. ) ;
#5608 = CARTESIAN_POINT ( 'NONE',  ( -68.99560423633737116, 1.595632167476292107, -7.480194822499073304 ) ) ;
#5609 = LINE ( 'NONE', #28299, #11265 ) ;
#5610 = PLANE ( 'NONE',  #26845 ) ;
#5611 = DIRECTION ( 'NONE',  ( 0.7660212471507180654, -0.6427876096865404731, 0.005961354470445141482 ) ) ;
#5612 = VECTOR ( 'NONE', #38111, 1000.000000000000227 ) ;
#5613 = EDGE_CURVE ( 'NONE', #36877, #12432, #4727, .T. ) ;
#5614 = CARTESIAN_POINT ( 'NONE',  ( -17.67592931590769112, 0.000000000000000000, 6.729515361707646193 ) ) ;
#5615 = DIRECTION ( 'NONE',  ( 0.5449076811759707706, 0.6444004775717708799, -0.5364919789714476250 ) ) ;
#5616 = VERTEX_POINT ( 'NONE', #34836 ) ;
#5617 = ORIENTED_EDGE ( 'NONE', *, *, #28588, .T. ) ;
#5618 = ORIENTED_EDGE ( 'NONE', *, *, #30492, .T. ) ;
#5619 = ORIENTED_EDGE ( 'NONE', *, *, #8471, .T. ) ;
#5620 = ORIENTED_EDGE ( 'NONE', *, *, #39320, .F. ) ;
#5621 = CARTESIAN_POINT ( 'NONE',  ( -12.33850799832341849, 0.000000000000000000, 11.68350162852954632 ) ) ;
#5622 = DIRECTION ( 'NONE',  ( -0.005961354470445682716, -0.6427876096865404731, 0.7660212471507180654 ) ) ;
#5623 = AXIS2_PLACEMENT_3D ( 'NONE', #16163, #37761, #42828 ) ;
#5624 = VECTOR ( 'NONE', #36125, 999.9999999999998863 ) ;
#5625 = ORIENTED_EDGE ( 'NONE', *, *, #44018, .F. ) ;
#5626 = EDGE_LOOP ( 'NONE', ( #12270, #18429, #24845, #18973 ) ) ;
#5627 = EDGE_CURVE ( 'NONE', #31317, #43546, #12969, .T. ) ;
#5629 = EDGE_CURVE ( 'NONE', #33244, #48860, #30297, .T. ) ;
#5628 = ORIENTED_EDGE ( 'NONE', *, *, #11680, .T. ) ;
#5630 = VECTOR ( 'NONE', #33261, 1000.000000000000227 ) ;
#5631 = CARTESIAN_POINT ( 'NONE',  ( -15.40103151951671734, 0.000000000000000000, 12.95233060667165681 ) ) ;
#5632 = DIRECTION ( 'NONE',  ( 0.007781995580012662783, 0.000000000000000000, -0.9999697198139514409 ) ) ;
#5633 = PLANE ( 'NONE',  #41355 ) ;
#5634 = ORIENTED_EDGE ( 'NONE', *, *, #26433, .T. ) ;
#5635 = CARTESIAN_POINT ( 'NONE',  ( -26.13337879274045505, 0.000000000000000000, 6.833023547870798353 ) ) ;
#5636 = ADVANCED_FACE ( 'NONE', ( #8734 ), #26053, .F. ) ;
#5637 = EDGE_CURVE ( 'NONE', #54774, #53284, #5018, .T. ) ;
#5638 = ORIENTED_EDGE ( 'NONE', *, *, #39578, .T. ) ;
#5639 = LINE ( 'NONE', #36057, #43643 ) ;
#5640 = VECTOR ( 'NONE', #55290, 1000.000000000000114 ) ;
#5641 = CARTESIAN_POINT ( 'NONE',  ( -20.73421763976967114, -3.108426967578159950, 4.836020290795394416 ) ) ;
#5642 = ADVANCED_FACE ( 'NONE', ( #42769 ), #8421, .F. ) ;
#5643 = PLANE ( 'NONE',  #3726 ) ;
#5644 = PLANE ( 'NONE',  #13348 ) ;
#5645 = VERTEX_POINT ( 'NONE', #34285 ) ;
#5646 = LINE ( 'NONE', #35467, #17661 ) ;
#5647 = CARTESIAN_POINT ( 'NONE',  ( -32.65841372305263235, 0.000000000000000000, 9.367568705923016381 ) ) ;
#5648 = CARTESIAN_POINT ( 'NONE',  ( -17.83139810946674686, -0.1191753592594197858, 13.85674710641801788 ) ) ;
#5649 = ORIENTED_EDGE ( 'NONE', *, *, #3679, .F. ) ;
#5650 = DIRECTION ( 'NONE',  ( -0.7660212471507179544, -0.6427876096865405842, -0.005961354470445141482 ) ) ;
#5651 = VERTEX_POINT ( 'NONE', #51593 ) ;
#5652 = DIRECTION ( 'NONE',  ( -0.5364919789714478471, 0.6444004775717705469, -0.5449076811759709926 ) ) ;
#5653 = PLANE ( 'NONE',  #50415 ) ;
#5654 = CARTESIAN_POINT ( 'NONE',  ( -13.27065584551087163, 0.000000000000000000, 12.04557950825129176 ) ) ;
#5655 = EDGE_CURVE ( 'NONE', #27148, #20460, #49006, .T. ) ;
#5656 = LINE ( 'NONE', #40858, #9653 ) ;
#5657 = TOROIDAL_SURFACE ( 'NONE', #31069, 3.457106781186553235, 0.2500000000000000000 ) ;
#5658 = CARTESIAN_POINT ( 'NONE',  ( -15.40103151951671734, 0.000000000000000000, 12.95233060667165681 ) ) ;
#5659 = FACE_OUTER_BOUND ( 'NONE', #3493, .T. ) ;
#5660 = DIRECTION ( 'NONE',  ( -0.7660212471507179544, -0.6427876096865405842, -0.005961354470445141482 ) ) ;
#5661 = EDGE_CURVE ( 'NONE', #45510, #52307, #53819, .T. ) ;
#5662 = PLANE ( 'NONE',  #38420 ) ;
#5663 =( NAMED_UNIT ( * ) SI_UNIT ( $, .STERADIAN. ) SOLID_ANGLE_UNIT ( ) );
#5664 = ADVANCED_FACE ( 'NONE', ( #32265 ), #1845, .F. ) ;
#5665 = FACE_OUTER_BOUND ( 'NONE', #7153, .T. ) ;
#5666 = VERTEX_POINT ( 'NONE', #48448 ) ;
#5667 = AXIS2_PLACEMENT_3D ( 'NONE', #33359, #30205, #12879 ) ;
#5668 = LINE ( 'NONE', #40612, #36611 ) ;
#5669 = CARTESIAN_POINT ( 'NONE',  ( -10.69332325015427543, 0.000000000000000000, 5.106521281233943554 ) ) ;
#5670 = CARTESIAN_POINT ( 'NONE',  ( -23.33849165029409889, 0.000000000000000000, 5.946783852668351855 ) ) ;
#5671 = CARTESIAN_POINT ( 'NONE',  ( 0.4518049228021103203, -3.655895688227122076, 5.998622290806040702 ) ) ;
#5672 = VECTOR ( 'NONE', #52739, 1000.000000000000227 ) ;
#5673 = EDGE_CURVE ( 'NONE', #28952, #36269, #41036, .T. ) ;
#5674 = VECTOR ( 'NONE', #51415, 999.9999999999998863 ) ;
#5675 = LINE ( 'NONE', #54217, #33672 ) ;
#5676 = DIRECTION ( 'NONE',  ( 0.005002170337468016433, -0.7660444431189770143, -0.6427681459581293666 ) ) ;
#5677 = DIRECTION ( 'NONE',  ( 0.9999697198139515519, 0.000000000000000000, 0.007781995580013368816 ) ) ;
#5678 = ORIENTED_EDGE ( 'NONE', *, *, #32768, .T. ) ;
#5679 = VECTOR ( 'NONE', #6739, 999.9999999999998863 ) ;
#5680 = VECTOR ( 'NONE', #24317, 1000.000000000000227 ) ;
#5681 = ORIENTED_EDGE ( 'NONE', *, *, #46260, .T. ) ;
#5682 = LINE ( 'NONE', #36629, #26861 ) ;
#5683 = DIRECTION ( 'NONE',  ( 0.007781995580012662783, 0.000000000000000000, -0.9999697198139514409 ) ) ;
#5684 = EDGE_LOOP ( 'NONE', ( #19261, #32006, #1364, #35597 ) ) ;
#5685 = DIRECTION ( 'NONE',  ( -0.005961354470445682716, -0.6427876096865404731, 0.7660212471507180654 ) ) ;
#5686 = VECTOR ( 'NONE', #20611, 1000.000000000000227 ) ;
#5687 = ORIENTED_EDGE ( 'NONE', *, *, #3415, .F. ) ;
#5688 = LINE ( 'NONE', #36932, #35674 ) ;
#5689 = ORIENTED_EDGE ( 'NONE', *, *, #50119, .T. ) ;
#5690 = VERTEX_POINT ( 'NONE', #49585 ) ;
#5691 = ORIENTED_EDGE ( 'NONE', *, *, #6022, .T. ) ;
#5692 = DIRECTION ( 'NONE',  ( 0.007781995580012663651, 0.000000000000000000, -0.9999697198139515519 ) ) ;
#5693 = LINE ( 'NONE', #53136, #4197 ) ;
#5694 = CARTESIAN_POINT ( 'NONE',  ( -17.74404816805336793, 0.000000000000000000, 3.574322630375089460 ) ) ;
#5695 = EDGE_CURVE ( 'NONE', #35896, #40396, #13626, .T. ) ;
#5696 = VECTOR ( 'NONE', #40835, 1000.000000000000000 ) ;
#5697 = DIRECTION ( 'NONE',  ( 0.9999697198139515519, 0.000000000000000000, 0.007781995580013368816 ) ) ;
#5698 = ORIENTED_EDGE ( 'NONE', *, *, #29171, .F. ) ;
#5700 = ORIENTED_EDGE ( 'NONE', *, *, #18864, .F. ) ;
#5699 = ADVANCED_FACE ( 'NONE', ( #14389 ), #31431, .F. ) ;
#5701 = VECTOR ( 'NONE', #28362, 1000.000000000000227 ) ;
#5702 = LINE ( 'NONE', #52830, #25491 ) ;
#5703 = VERTEX_POINT ( 'NONE', #44206 ) ;
#5704 = VECTOR ( 'NONE', #41707, 999.9999999999998863 ) ;
#5705 = DIRECTION ( 'NONE',  ( 0.005002170337468016433, -0.7660444431189770143, -0.6427681459581293666 ) ) ;
#5706 = VERTEX_POINT ( 'NONE', #39924 ) ;
#5707 = LINE ( 'NONE', #21901, #51424 ) ;
#5708 = DIRECTION ( 'NONE',  ( -0.5364919789714478471, 0.6444004775717705469, -0.5449076811759709926 ) ) ;
#5709 = EDGE_CURVE ( 'NONE', #21014, #24397, #2125, .T. ) ;
#5710 = EDGE_CURVE ( 'NONE', #35896, #41243, #40512, .T. ) ;
#5711 = EDGE_CURVE ( 'NONE', #54087, #19187, #10399, .T. ) ;
#5712 = VECTOR ( 'NONE', #18052, 999.9999999999998863 ) ;
#5713 = AXIS2_PLACEMENT_3D ( 'NONE', #19490, #37655, #37935 ) ;
#5714 = ORIENTED_EDGE ( 'NONE', *, *, #19360, .T. ) ;
#5715 = LINE ( 'NONE', #44597, #2287 ) ;
#5716 = EDGE_LOOP ( 'NONE', ( #35266, #10739, #43199, #14261 ) ) ;
#5717 = EDGE_CURVE ( 'NONE', #50946, #45163, #28001, .T. ) ;
#5718 = VECTOR ( 'NONE', #31620, 1000.000000000000227 ) ;
#5719 = CARTESIAN_POINT ( 'NONE',  ( -17.67018120889713018, 0.000000000000000000, 5.990895955192118372 ) ) ;
#5720 = AXIS2_PLACEMENT_3D ( 'NONE', #34953, #8537, #21863 ) ;
#5721 = EDGE_LOOP ( 'NONE', ( #34108, #16188, #51, #38760 ) ) ;
#5722 = DIRECTION ( 'NONE',  ( 0.007781995580012662783, 0.000000000000000000, -0.9999697198139514409 ) ) ;
#5723 = LINE ( 'NONE', #9984, #54696 ) ;
#5724 = LINE ( 'NONE', #13956, #1069 ) ;
#5725 = VERTEX_POINT ( 'NONE', #1005 ) ;
#5726 = DIRECTION ( 'NONE',  ( 0.007781995580012662783, 0.000000000000000000, -0.9999697198139514409 ) ) ;
#5727 = DIRECTION ( 'NONE',  ( 0.000000000000000000, -1.000000000000000000, 0.000000000000000000 ) ) ;
#5728 = AXIS2_PLACEMENT_3D ( 'NONE', #12213, #21594, #50042 ) ;
#5729 = FACE_OUTER_BOUND ( 'NONE', #46000, .T. ) ;
#5730 = VECTOR ( 'NONE', #40205, 1000.000000000000000 ) ;
#5731 = CARTESIAN_POINT ( 'NONE',  ( -10.41874048237084693, 0.000000000000000000, 3.831335924817679484 ) ) ;
#5732 = CARTESIAN_POINT ( 'NONE',  ( -50.02554558092695913, 3.776013638374817294, 5.000000000000000000 ) ) ;
#5733 = EDGE_CURVE ( 'NONE', #27927, #31034, #19461, .T. ) ;
#5734 = CARTESIAN_POINT ( 'NONE',  ( -65.67591093208449138, -11.23903885787223267, -5.460169066039067154 ) ) ;
#5735 = EDGE_LOOP ( 'NONE', ( #35507, #862, #29776, #12547 ) ) ;
#5736 = DIRECTION ( 'NONE',  ( -0.6427681459581293666, -0.7660444431189770143, -0.005002170337467561935 ) ) ;
#5737 = LINE ( 'NONE', #13972, #23164 ) ;
#5738 = ADVANCED_FACE ( 'NONE', ( #31701 ), #6409, .F. ) ;
#5739 = CARTESIAN_POINT ( 'NONE',  ( -65.60880995838058993, 5.724587470723463412E-14, -0.7600040867678790057 ) ) ;
#5740 = ORIENTED_EDGE ( 'NONE', *, *, #13032, .F. ) ;
#5741 = CARTESIAN_POINT ( 'NONE',  ( -8.599902753822396662, -0.1191753592594186617, 4.853483721896219016 ) ) ;
#5742 = LINE ( 'NONE', #17688, #28176 ) ;
#5743 = APPLICATION_CONTEXT ( 'automotive_design' ) ;
#5744 = VERTEX_POINT ( 'NONE', #54117 ) ;
#5745 = AXIS2_PLACEMENT_3D ( 'NONE', #46996, #12636, #38465 ) ;
#5746 = FACE_OUTER_BOUND ( 'NONE', #55715, .T. ) ;
#5747 = EDGE_CURVE ( 'NONE', #12432, #53402, #27152, .T. ) ;
#5748 = CARTESIAN_POINT ( 'NONE',  ( -9.750021733713985839, 1.198032013860655054, 1.892571191312284906 ) ) ;
#5749 = VECTOR ( 'NONE', #47155, 999.9999999999998863 ) ;
#5750 = CARTESIAN_POINT ( 'NONE',  ( -19.26408584338317098, 0.000000000000000000, 5.978491820772086740 ) ) ;
#5751 = EDGE_CURVE ( 'NONE', #34091, #23582, #44742, .T. ) ;
#5752 = PLANE ( 'NONE',  #1100 ) ;
#5753 = VERTEX_POINT ( 'NONE', #9848 ) ;
#5754 = ORIENTED_EDGE ( 'NONE', *, *, #35787, .T. ) ;
#5755 = CARTESIAN_POINT ( 'NONE',  ( -20.54126990917373519, -0.1191753592594197858, 4.760553241521720658 ) ) ;
#5756 = VECTOR ( 'NONE', #13716, 1000.000000000000227 ) ;
#5757 = DIRECTION ( 'NONE',  ( -0.005961354470445682716, -0.6427876096865404731, 0.7660212471507180654 ) ) ;
#5758 = AXIS2_PLACEMENT_3D ( 'NONE', #44985, #31062, #44404 ) ;
#5759 = CARTESIAN_POINT ( 'NONE',  ( -11.87243407472968926, 0.000000000000000000, 11.50246268866867361 ) ) ;
#5760 = AXIS2_PLACEMENT_3D ( 'NONE', #35935, #14350, #49238 ) ;
#5761 = DIRECTION ( 'NONE',  ( -0.005002170337468016433, -0.7660444431189770143, 0.6427681459581293666 ) ) ;
#5762 = ORIENTED_EDGE ( 'NONE', *, *, #17362, .T. ) ;
#5763 = CARTESIAN_POINT ( 'NONE',  ( -9.039200059374007168, 0.000000000000000000, 5.688732176410531416 ) ) ;
#5764 = EDGE_LOOP ( 'NONE', ( #29127, #53218, #8128, #13175 ) ) ;
#5765 = DIRECTION ( 'NONE',  ( -0.5364919789714478471, 0.6444004775717705469, -0.5449076811759709926 ) ) ;
#5766 = VECTOR ( 'NONE', #32105, 999.9999999999998863 ) ;
#5767 = DIRECTION ( 'NONE',  ( -0.5449076811759708816, 0.6444004775717707689, 0.5364919789714475140 ) ) ;
#5768 = VECTOR ( 'NONE', #29789, 1000.000000000000114 ) ;
#5769 = VERTEX_POINT ( 'NONE', #45309 ) ;
#5770 = PLANE ( 'NONE',  #36522 ) ;
#5771 = FACE_OUTER_BOUND ( 'NONE', #18979, .T. ) ;
#5772 = DIRECTION ( 'NONE',  ( 0.007781995580012663651, -3.146120232559066537E-19, -0.9999697198139514409 ) ) ;
#5773 = EDGE_LOOP ( 'NONE', ( #1122, #2809, #26018, #17365 ) ) ;
#5774 = PLANE ( 'NONE',  #46618 ) ;
#5775 = ORIENTED_EDGE ( 'NONE', *, *, #21982, .T. ) ;
#5776 = ORIENTED_EDGE ( 'NONE', *, *, #33851, .F. ) ;
#5777 = ORIENTED_EDGE ( 'NONE', *, *, #36764, .T. ) ;
#5778 = FACE_OUTER_BOUND ( 'NONE', #16646, .T. ) ;
#5779 = VECTOR ( 'NONE', #25335, 999.9999999999998863 ) ;
#5780 = ORIENTED_EDGE ( 'NONE', *, *, #40899, .T. ) ;
#5781 = CARTESIAN_POINT ( 'NONE',  ( -69.66347483736342383, -8.676648739292067702, -7.503912900124009688 ) ) ;
#5782 = VERTEX_POINT ( 'NONE', #22882 ) ;
#5783 = VECTOR ( 'NONE', #49906, 999.9999999999998863 ) ;
#5784 = DIRECTION ( 'NONE',  ( 0.007781995580012663651, -3.146120232559066537E-19, -0.9999697198139514409 ) ) ;
#5785 = DIRECTION ( 'NONE',  ( -0.6427681459581293666, -0.7660444431189770143, -0.005002170337467561935 ) ) ;
#5786 = ADVANCED_FACE ( 'NONE', ( #44460 ), #53542, .F. ) ;
#5787 = EDGE_CURVE ( 'NONE', #16268, #48488, #6158, .T. ) ;
#5788 = ORIENTED_EDGE ( 'NONE', *, *, #51919, .F. ) ;
#5789 = ORIENTED_EDGE ( 'NONE', *, *, #8043, .T. ) ;
#5790 = DIRECTION ( 'NONE',  ( -0.7660212471507179544, -0.6427876096865405842, -0.005961354470445141482 ) ) ;
#5791 = AXIS2_PLACEMENT_3D ( 'NONE', #38307, #28694, #45709 ) ;
#5792 = ORIENTED_EDGE ( 'NONE', *, *, #36954, .F. ) ;
#5793 = EDGE_CURVE ( 'NONE', #44937, #28121, #3538, .T. ) ;
#5794 = DIRECTION ( 'NONE',  ( 0.007781995580012663651, -3.146120232559066537E-19, -0.9999697198139514409 ) ) ;
#5795 = LINE ( 'NONE', #18573, #11156 ) ;
#5796 = FACE_OUTER_BOUND ( 'NONE', #1460, .T. ) ;
#5797 = CARTESIAN_POINT ( 'NONE',  ( -14.94760462649100496, 0.000000000000000000, 2.488088991209854051 ) ) ;
#5798 = LINE ( 'NONE', #53240, #4237 ) ;
#5799 = AXIS2_PLACEMENT_3D ( 'NONE', #37189, #32928, #27864 ) ;
#5800 = PLANE ( 'NONE',  #5593 ) ;
#5801 = DIRECTION ( 'NONE',  ( -0.6427681459581293666, -0.7660444431189770143, -0.005002170337467561935 ) ) ;
#5802 = VERTEX_POINT ( 'NONE', #11517 ) ;
#5803 = VECTOR ( 'NONE', #47710, 1000.000000000000227 ) ;
#5804 = ORIENTED_EDGE ( 'NONE', *, *, #9478, .F. ) ;
#5805 = LINE ( 'NONE', #18283, #6530 ) ;
#5806 = DIRECTION ( 'NONE',  ( 0.5449076811759707706, 0.6444004775717708799, -0.5364919789714476250 ) ) ;
#5807 = DIRECTION ( 'NONE',  ( 0.3535533905932752297, -0.6123724356957952475, -0.7071067811865462405 ) ) ;
#5808 = AXIS2_PLACEMENT_3D ( 'NONE', #26768, #9750, #4369 ) ;
#5809 = VECTOR ( 'NONE', #41899, 1000.000000000000000 ) ;
#5810 = CARTESIAN_POINT ( 'NONE',  ( -14.59642022908046499, -2.460819163488160655, 2.472553415555822198 ) ) ;
#5811 = ORIENTED_EDGE ( 'NONE', *, *, #54283, .T. ) ;
#5812 = DIRECTION ( 'NONE',  ( 0.7660212471507180654, -0.6427876096865404731, 0.005961354470445141482 ) ) ;
#5813 = CARTESIAN_POINT ( 'NONE',  ( -70.01399353402076997, 0.005543651780989746099, -7.502022462329923869 ) ) ;
#5814 = ORIENTED_EDGE ( 'NONE', *, *, #30730, .F. ) ;
#5815 = CARTESIAN_POINT ( 'NONE',  ( 2.072287782118878319, 0.000000000000000000, -2.950529333540147015 ) ) ;
#5816 = CARTESIAN_POINT ( 'NONE',  ( -27.13299098042555002, 16.99303619941258603, -4.657414165320978405 ) ) ;
#5817 = VERTEX_POINT ( 'NONE', #11771 ) ;
#5818 = DIRECTION ( 'NONE',  ( 0.005002170337468016433, -0.7660444431189770143, -0.6427681459581293666 ) ) ;
#5819 = DIRECTION ( 'NONE',  ( 0.000000000000000000, 0.000000000000000000, 1.000000000000000000 ) ) ;
#5820 = LINE ( 'NONE', #3226, #32284 ) ;
#5821 = EDGE_CURVE ( 'NONE', #11647, #2600, #16308, .T. ) ;
#5822 = CARTESIAN_POINT ( 'NONE',  ( -15.60102546347950536, 0.000000000000000000, 12.95077420755565356 ) ) ;
#5823 = DIRECTION ( 'NONE',  ( 0.6427681459581294776, -0.7660444431189769032, 0.005002170337467562802 ) ) ;
#5824 = EDGE_LOOP ( 'NONE', ( #8863, #29999, #13723, #22333 ) ) ;
#5825 = VECTOR ( 'NONE', #44119, 999.9999999999998863 ) ;
#5826 = ADVANCED_FACE ( 'NONE', ( #19749 ), #45567, .F. ) ;
#5827 = VERTEX_POINT ( 'NONE', #2680 ) ;
#5828 = DIRECTION ( 'NONE',  ( -0.7660212471507179544, -0.6427876096865405842, -0.005961354470445141482 ) ) ;
#5829 = CARTESIAN_POINT ( 'NONE',  ( -18.66354898467281132, 0.000000000000000000, 14.21960318569776582 ) ) ;
#5830 = CARTESIAN_POINT ( 'NONE',  ( -22.40634380310664397, 0.000000000000000000, 5.584705972946605534 ) ) ;
#5831 = ADVANCED_FACE ( 'NONE', ( #24290 ), #55219, .F. ) ;
#5832 = AXIS2_PLACEMENT_3D ( 'NONE', #10889, #32494, #20542 ) ;
#5833 = CARTESIAN_POINT ( 'NONE',  ( -15.51406735044831997, -5.213152330870665097, 2.741184882836876113 ) ) ;
#5834 = ADVANCED_FACE ( 'NONE', ( #54949 ), #16053, .F. ) ;
#5835 = DIRECTION ( 'NONE',  ( 0.007781995580012663651, 0.000000000000000000, -0.9999697198139515519 ) ) ;
#5836 = AXIS2_PLACEMENT_3D ( 'NONE', #26311, #26062, #51330 ) ;
#5837 = ORIENTED_EDGE ( 'NONE', *, *, #26390, .F. ) ;
#5838 = CARTESIAN_POINT ( 'NONE',  ( -13.83440620147302269, 24.67097770138186874, -3.662372917584403087 ) ) ;
#5839 = FACE_OUTER_BOUND ( 'NONE', #31708, .T. ) ;
#5840 = DIRECTION ( 'NONE',  ( 0.007781995580012662783, 0.000000000000000000, -0.9999697198139514409 ) ) ;
#5841 = CARTESIAN_POINT ( 'NONE',  ( -16.89925026227929195, -0.1191753592594197858, 13.49466922669627422 ) ) ;
#5842 = ORIENTED_EDGE ( 'NONE', *, *, #42512, .T. ) ;
#5843 = VECTOR ( 'NONE', #33761, 1000.000000000000227 ) ;
#5844 = DIRECTION ( 'NONE',  ( 0.7660212471507180654, -0.6427876096865404731, 0.005961354470445141482 ) ) ;
#5845 = ORIENTED_EDGE ( 'NONE', *, *, #17009, .T. ) ;
#5846 = FACE_OUTER_BOUND ( 'NONE', #25240, .T. ) ;
#5847 = FACE_OUTER_BOUND ( 'NONE', #24098, .T. ) ;
#5848 = VECTOR ( 'NONE', #33716, 1000.000000000000227 ) ;
#5849 = VERTEX_POINT ( 'NONE', #20291 ) ;
#5850 = DIRECTION ( 'NONE',  ( -0.5364919789714478471, 0.6444004775717705469, -0.5449076811759709926 ) ) ;
#5851 = EDGE_LOOP ( 'NONE', ( #10953, #52318, #1061, #49540 ) ) ;
#5852 = CIRCLE ( 'NONE', #10392, 2.750000000000001776 ) ;
#5853 = ORIENTED_EDGE ( 'NONE', *, *, #39892, .F. ) ;
#5854 = ORIENTED_EDGE ( 'NONE', *, *, #26539, .F. ) ;
#5855 = CARTESIAN_POINT ( 'NONE',  ( -27.06708303904391144, 0.000000000000000000, 7.395095371555332697 ) ) ;
#5856 = AXIS2_PLACEMENT_3D ( 'NONE', #20019, #29708, #29399 ) ;
#5857 = VERTEX_POINT ( 'NONE', #12043 ) ;
#5858 = ORIENTED_EDGE ( 'NONE', *, *, #31690, .F. ) ;
#5859 = CARTESIAN_POINT ( 'NONE',  ( -12.70458494993575194, -0.1191753592594197858, 11.86531876794841978 ) ) ;
#5860 = EDGE_CURVE ( 'NONE', #2010, #8607, #33378, .T. ) ;
#5861 = DIRECTION ( 'NONE',  ( 0.6427681459581294776, -0.7660444431189769032, 0.005002170337467562802 ) ) ;
#5862 = ORIENTED_EDGE ( 'NONE', *, *, #37251, .T. ) ;
#5863 = EDGE_CURVE ( 'NONE', #23769, #30544, #42448, .T. ) ;
#5864 = ORIENTED_EDGE ( 'NONE', *, *, #50563, .T. ) ;
#5865 = DIRECTION ( 'NONE',  ( -0.5364919789714478471, 0.6444004775717705469, -0.5449076811759709926 ) ) ;
#5866 = ORIENTED_EDGE ( 'NONE', *, *, #34558, .T. ) ;
#5867 = EDGE_LOOP ( 'NONE', ( #55251, #10809, #23707, #39370 ) ) ;
#5868 = ADVANCED_FACE ( 'NONE', ( #7241 ), #20594, .F. ) ;
#5869 = EDGE_CURVE ( 'NONE', #2187, #17736, #50939, .T. ) ;
#5870 = VECTOR ( 'NONE', #14657, 1000.000000000000227 ) ;
#5871 = DIRECTION ( 'NONE',  ( -0.6427681459581293666, -0.7660444431189770143, -0.005002170337467561935 ) ) ;
#5872 = VECTOR ( 'NONE', #26184, 999.9999999999998863 ) ;
#5873 = CARTESIAN_POINT ( 'NONE',  ( 5.057731014323088026, -1.114607557371864122, 2.289010529401726668 ) ) ;
#5874 = DIRECTION ( 'NONE',  ( -0.9999697198139514409, -0.000000000000000000, -0.007781995580013368816 ) ) ;
#5875 = DIRECTION ( 'NONE',  ( 0.6427681459581294776, -0.7660444431189769032, 0.005002170337467562802 ) ) ;
#5876 = ORIENTED_EDGE ( 'NONE', *, *, #31751, .F. ) ;
#5877 = PLANE ( 'NONE',  #55491 ) ;
#5878 = VECTOR ( 'NONE', #50572, 999.9999999999998863 ) ;
#5879 = ORIENTED_EDGE ( 'NONE', *, *, #33488, .F. ) ;
#5880 = DIRECTION ( 'NONE',  ( 0.007781995580012663651, 0.000000000000000000, -0.9999697198139515519 ) ) ;
#5881 = EDGE_CURVE ( 'NONE', #50938, #6281, #29382, .T. ) ;
#5882 = CARTESIAN_POINT ( 'NONE',  ( -25.20200914511100265, -0.1191753592594197858, 6.570942640130446932 ) ) ;
#5883 = AXIS2_PLACEMENT_3D ( 'NONE', #22070, #13290, #48468 ) ;
#5884 = CARTESIAN_POINT ( 'NONE',  ( -69.89574092751220746, 0.1327608315404790740, 7.370754069753728821 ) ) ;
#5885 = DIRECTION ( 'NONE',  ( 0.005961354470445682716, -0.6427876096865404731, -0.7660212471507180654 ) ) ;
#5886 = CARTESIAN_POINT ( 'NONE',  ( -17.74560456716937296, 0.000000000000000000, 3.774316574337878372 ) ) ;
#5887 = VECTOR ( 'NONE', #47175, 1000.000000000000114 ) ;
#5888 = CARTESIAN_POINT ( 'NONE',  ( -11.10260204233550496, -0.5179957512181551094, 1.844678686450966332 ) ) ;
#5889 = ORIENTED_EDGE ( 'NONE', *, *, #97, .F. ) ;
#5890 = CARTESIAN_POINT ( 'NONE',  ( 2.072287782118878319, 0.000000000000000000, -2.950529333540147015 ) ) ;
#5891 = EDGE_LOOP ( 'NONE', ( #11041, #52070, #11588, #11052 ) ) ;
#5892 = VECTOR ( 'NONE', #39817, 1000.000000000000227 ) ;
#5893 = CARTESIAN_POINT ( 'NONE',  ( -21.46924666352205335, 3.686347215771509145, 11.27062942325050976 ) ) ;
#5894 = DIRECTION ( 'NONE',  ( 0.5449076811759707706, 0.6444004775717708799, -0.5364919789714476250 ) ) ;
#5895 = PLANE ( 'NONE',  #20882 ) ;
#5896 = CARTESIAN_POINT ( 'NONE',  ( -20.10958161055168247, -0.1191753592594196887, 5.871908949099878150 ) ) ;
#5897 = DIRECTION ( 'NONE',  ( 0.9321478471874540261, 0.000000000000000000, -0.3620778797217457101 ) ) ;
#5898 = VECTOR ( 'NONE', #41313, 999.9999999999998863 ) ;
#5899 = CARTESIAN_POINT ( 'NONE',  ( -70.39747693292142117, -1.183819181302419339E-15, -9.299316846403151260 ) ) ;
#5900 = VECTOR ( 'NONE', #21996, 1000.000000000000000 ) ;
#5901 = ORIENTED_EDGE ( 'NONE', *, *, #7231, .T. ) ;
#5902 = DIRECTION ( 'NONE',  ( -0.9999697198139514409, -0.000000000000000000, -0.007781995580013368816 ) ) ;
#5903 = CARTESIAN_POINT ( 'NONE',  ( -22.40478740399063895, 0.000000000000000000, 5.384712028983816623 ) ) ;
#5904 = CARTESIAN_POINT ( 'NONE',  ( -19.35113876198915861, 0.000000000000000000, 7.824474703863986136 ) ) ;
#5905 = CARTESIAN_POINT ( 'NONE',  ( -68.87092941434458737, 1.666157950113242636, -7.477522605581019555 ) ) ;
#5906 = EDGE_CURVE ( 'NONE', #37913, #9089, #41860, .T. ) ;
#5907 = DIRECTION ( 'NONE',  ( 0.5449076811759707706, 0.6444004775717708799, -0.5364919789714476250 ) ) ;
#5908 = DIRECTION ( 'NONE',  ( 0.6427681459581294776, -0.7660444431189769032, 0.005002170337467562802 ) ) ;
#5909 = AXIS2_PLACEMENT_3D ( 'NONE', #8779, #13572, #5605 ) ;
#5910 = FACE_OUTER_BOUND ( 'NONE', #5492, .T. ) ;
#5911 = CARTESIAN_POINT ( 'NONE',  ( -14.93495759592298988, 0.000000000000000000, 12.77129166681078409 ) ) ;
#5912 = VECTOR ( 'NONE', #47570, 1000.000000000000000 ) ;
#5913 = EDGE_CURVE ( 'NONE', #24516, #48984, #32792, .T. ) ;
#5914 = VERTEX_POINT ( 'NONE', #28253 ) ;
#5915 = AXIS2_PLACEMENT_3D ( 'NONE', #22440, #9927, #30675 ) ;
#5916 = EDGE_CURVE ( 'NONE', #5706, #50902, #49840, .T. ) ;
#5917 = EDGE_CURVE ( 'NONE', #19489, #6417, #50100, .T. ) ;
#5918 = VERTEX_POINT ( 'NONE', #6685 ) ;
#5919 = EDGE_LOOP ( 'NONE', ( #34905, #12353, #43617, #11943 ) ) ;
#5920 = AXIS2_PLACEMENT_3D ( 'NONE', #27353, #31899, #10875 ) ;
#5921 = VECTOR ( 'NONE', #37574, 1000.000000000000227 ) ;
#5922 = ORIENTED_EDGE ( 'NONE', *, *, #35503, .T. ) ;
#5923 = VECTOR ( 'NONE', #27905, 999.9999999999998863 ) ;
#5924 = VERTEX_POINT ( 'NONE', #24542 ) ;
#5925 = DIRECTION ( 'NONE',  ( 0.007781995580012663651, 0.000000000000000000, -0.9999697198139515519 ) ) ;
#5926 = EDGE_CURVE ( 'NONE', #18779, #21631, #8828, .T. ) ;
#5927 = CARTESIAN_POINT ( 'NONE',  ( -56.38001980572109062, 4.410024460692103077, -3.000000000000007105 ) ) ;
#5928 = AXIS2_PLACEMENT_3D ( 'NONE', #44296, #53097, #40307 ) ;
#5930 = ADVANCED_FACE ( 'NONE', ( #37621 ), #38456, .F. ) ;
#5929 = ORIENTED_EDGE ( 'NONE', *, *, #17543, .F. ) ;
#5931 = VERTEX_POINT ( 'NONE', #30525 ) ;
#5932 = ORIENTED_EDGE ( 'NONE', *, *, #10297, .T. ) ;
#5933 = ADVANCED_FACE ( 'NONE', ( #17424 ), #39022, .F. ) ;
#5934 = AXIS2_PLACEMENT_3D ( 'NONE', #23567, #40883, #23834 ) ;
#5935 = AXIS2_PLACEMENT_3D ( 'NONE', #24184, #3139, #33273 ) ;
#5936 = CARTESIAN_POINT ( 'NONE',  ( 0.3240706152708106025, -3.670543518250628967, -1.335466778558061241E-15 ) ) ;
#5937 = LINE ( 'NONE', #30664, #3774 ) ;
#5938 = CARTESIAN_POINT ( 'NONE',  ( -10.94028622754223967, 0.000000000000000000, 11.14038480894692995 ) ) ;
#5939 = ORIENTED_EDGE ( 'NONE', *, *, #15241, .F. ) ;
#5940 = LINE ( 'NONE', #31770, #14692 ) ;
#5941 = ADVANCED_FACE ( 'NONE', ( #35069 ), #21968, .F. ) ;
#5942 = ORIENTED_EDGE ( 'NONE', *, *, #26273, .T. ) ;
#5943 = LINE ( 'NONE', #9336, #11007 ) ;
#5944 = DIRECTION ( 'NONE',  ( -0.6427681459581293666, -0.7660444431189770143, -0.005002170337467561935 ) ) ;
#5945 = AXIS2_PLACEMENT_3D ( 'NONE', #13511, #30571, #17199 ) ;
#5946 = EDGE_CURVE ( 'NONE', #3951, #30703, #17732, .T. ) ;
#5947 = DIRECTION ( 'NONE',  ( -0.5449076811759708816, 0.6444004775717707689, 0.5364919789714475140 ) ) ;
#5948 = CARTESIAN_POINT ( 'NONE',  ( -14.01545677930355183, 0.000000000000000000, 2.126011111488108174 ) ) ;
#5949 = CARTESIAN_POINT ( 'NONE',  ( -61.38973930853472183, 7.404220597074748333, 2.999999999999993339 ) ) ;
#5950 = DIRECTION ( 'NONE',  ( -0.005002170337468016433, -0.7660444431189770143, 0.6427681459581293666 ) ) ;
#5952 = VECTOR ( 'NONE', #22817, 999.9999999999998863 ) ;
#5951 = DIRECTION ( 'NONE',  ( -0.005961354470445682716, -0.6427876096865404731, 0.7660212471507180654 ) ) ;
#5953 = EDGE_LOOP ( 'NONE', ( #19872, #47122, #30568, #3263, #13837 ) ) ;
#5954 = PLANE ( 'NONE',  #9276 ) ;
#5955 = ORIENTED_EDGE ( 'NONE', *, *, #41848, .T. ) ;
#5956 = VECTOR ( 'NONE', #30182, 1000.000000000000114 ) ;
#5957 = DIRECTION ( 'NONE',  ( 0.007781995580012662783, 0.000000000000000000, -0.9999697198139514409 ) ) ;
#5958 = LINE ( 'NONE', #23278, #6982 ) ;
#5959 = CARTESIAN_POINT ( 'NONE',  ( -20.72814514249575168, 20.40220053346460460, 4.343046601168861542 ) ) ;
#5960 = CARTESIAN_POINT ( 'NONE',  ( -15.33262645716528461, 0.000000000000000000, 4.162426997743341239 ) ) ;
#5961 = VECTOR ( 'NONE', #29045, 1000.000000000000227 ) ;
#5962 = CARTESIAN_POINT ( 'NONE',  ( -21.90706668065662654, 4.819660872929013351, 5.037607981832593396 ) ) ;
#5963 = PLANE ( 'NONE',  #435 ) ;
#5964 = LINE ( 'NONE', #49096, #29767 ) ;
#5966 = VECTOR ( 'NONE', #29884, 999.9999999999998863 ) ;
#5965 = CARTESIAN_POINT ( 'NONE',  ( 2.072287782118878319, 0.000000000000000000, -2.950529333540147015 ) ) ;
#5967 = VECTOR ( 'NONE', #24284, 1000.000000000000227 ) ;
#5968 =( NAMED_UNIT ( * ) PLANE_ANGLE_UNIT ( ) SI_UNIT ( $, .RADIAN. ) );
#5969 = DIRECTION ( 'NONE',  ( -0.005002170337468016433, -0.7660444431189770143, 0.6427681459581293666 ) ) ;
#5970 = ORIENTED_EDGE ( 'NONE', *, *, #33462, .T. ) ;
#5971 = LINE ( 'NONE', #1945, #17560 ) ;
#5972 = DIRECTION ( 'NONE',  ( 0.9999697198139515519, 0.000000000000000000, 0.007781995580013368816 ) ) ;
#5973 = DIRECTION ( 'NONE',  ( 0.005961354470445682716, -0.6427876096865404731, -0.7660212471507180654 ) ) ;
#5975 = VECTOR ( 'NONE', #44703, 1000.000000000000000 ) ;
#5974 = PLANE ( 'NONE',  #15088 ) ;
#5976 = CIRCLE ( 'NONE', #11382, 0.5000000000000004441 ) ;
#5977 = LINE ( 'NONE', #40319, #25490 ) ;
#5978 = VECTOR ( 'NONE', #42555, 1000.000000000000227 ) ;
#5979 = EDGE_CURVE ( 'NONE', #22139, #43104, #34228, .T. ) ;
#5980 = DIRECTION ( 'NONE',  ( 0.005961354470445682716, -0.6427876096865404731, -0.7660212471507180654 ) ) ;
#5981 = LINE ( 'NONE', #45402, #10243 ) ;
#5982 = ORIENTED_EDGE ( 'NONE', *, *, #49981, .T. ) ;
#5983 = VECTOR ( 'NONE', #42987, 1000.000000000000000 ) ;
#5984 = AXIS2_PLACEMENT_3D ( 'NONE', #36538, #10140, #27763 ) ;
#5985 = EDGE_LOOP ( 'NONE', ( #26212, #4671, #31421, #2724 ) ) ;
#5986 = DIRECTION ( 'NONE',  ( 0.5449076811759707706, 0.6444004775717708799, -0.5364919789714476250 ) ) ;
#5987 = DIRECTION ( 'NONE',  ( 0.7660212471507180654, -0.6427876096865404731, 0.005961354470445141482 ) ) ;
#5988 = EDGE_LOOP ( 'NONE', ( #26371, #16218, #31808, #19968 ) ) ;
#5989 = DIRECTION ( 'NONE',  ( 0.007781995580012662783, 0.000000000000000000, -0.9999697198139514409 ) ) ;
#5990 = ORIENTED_EDGE ( 'NONE', *, *, #12440, .F. ) ;
#5991 = PLANE ( 'NONE',  #32897 ) ;
#5992 = EDGE_CURVE ( 'NONE', #3929, #35510, #26241, .T. ) ;
#5993 = VECTOR ( 'NONE', #13162, 999.9999999999998863 ) ;
#5994 = ORIENTED_EDGE ( 'NONE', *, *, #20676, .T. ) ;
#5995 = ORIENTED_EDGE ( 'NONE', *, *, #43242, .F. ) ;
#5996 = EDGE_LOOP ( 'NONE', ( #36506, #54861, #40288, #50594 ) ) ;
#5997 = CARTESIAN_POINT ( 'NONE',  ( 3.004435629306332345, -1.000000000000000000, -3.312607213261892003 ) ) ;
#5998 = CARTESIAN_POINT ( 'NONE',  ( -16.81190032086591302, 0.000000000000000000, 3.212244750653343583 ) ) ;
#5999 = AXIS2_PLACEMENT_3D ( 'NONE', #5520, #18029, #416 ) ;
#6000 = DIRECTION ( 'NONE',  ( 0.7660212471507180654, -0.6427876096865404731, 0.005961354470445141482 ) ) ;
#6001 = DIRECTION ( 'NONE',  ( -0.8531650599175529814, -0.4028455766673920135, 0.3313982828793697877 ) ) ;
#6002 = EDGE_CURVE ( 'NONE', #5490, #12113, #13190, .T. ) ;
#6003 = ORIENTED_EDGE ( 'NONE', *, *, #22469, .T. ) ;
#6004 = VECTOR ( 'NONE', #16539, 1000.000000000000227 ) ;
#6005 = ORIENTED_EDGE ( 'NONE', *, *, #23913, .F. ) ;
#6006 = EDGE_CURVE ( 'NONE', #44182, #55542, #43553, .T. ) ;
#6007 = AXIS2_PLACEMENT_3D ( 'NONE', #45138, #45667, #1396 ) ;
#6008 = AXIS2_PLACEMENT_3D ( 'NONE', #49522, #2061, #28777 ) ;
#6009 = PLANE ( 'NONE',  #39996 ) ;
#6010 = EDGE_LOOP ( 'NONE', ( #38108, #39885, #47498, #14252, #21388 ) ) ;
#6011 = DIRECTION ( 'NONE',  ( -0.005002170337468016433, -0.7660444431189770143, 0.6427681459581293666 ) ) ;
#6012 = EDGE_LOOP ( 'NONE', ( #18636, #41171, #55271, #54668 ) ) ;
#6013 = DIRECTION ( 'NONE',  ( 0.000000000000000000, -1.000000000000000000, 0.000000000000000000 ) ) ;
#6014 = CARTESIAN_POINT ( 'NONE',  ( -10.69907135716483992, 0.000000000000000000, 5.845140687749472264 ) ) ;
#6015 = AXIS2_PLACEMENT_3D ( 'NONE', #32625, #3074, #45397 ) ;
#6016 = ADVANCED_FACE ( 'NONE', ( #4110 ), #21436, .F. ) ;
#6017 = VERTEX_POINT ( 'NONE', #12896 ) ;
#6018 = VECTOR ( 'NONE', #7054, 1000.000000000000227 ) ;
#6019 = PLANE ( 'NONE',  #55808 ) ;
#6020 = ORIENTED_EDGE ( 'NONE', *, *, #31135, .T. ) ;
#6021 = AXIS2_PLACEMENT_3D ( 'NONE', #8866, #43478, #17641 ) ;
#6022 = EDGE_CURVE ( 'NONE', #17269, #38231, #39297, .T. ) ;
#6023 = DIRECTION ( 'NONE',  ( 0.000000000000000000, -1.000000000000000000, 0.000000000000000000 ) ) ;
#6024 = VECTOR ( 'NONE', #4150, 1000.000000000000114 ) ;
#6025 = ORIENTED_EDGE ( 'NONE', *, *, #42934, .T. ) ;
#6026 = DIRECTION ( 'NONE',  ( 0.000000000000000000, -0.000000000000000000, -1.000000000000000000 ) ) ;
#6027 = PLANE ( 'NONE',  #25693 ) ;
#6028 = DIRECTION ( 'NONE',  ( -0.7660212471507179544, -0.6427876096865405842, -0.005961354470445141482 ) ) ;
#6029 = ORIENTED_EDGE ( 'NONE', *, *, #42849, .F. ) ;
#6030 = DIRECTION ( 'NONE',  ( 0.9999697198139515519, 0.000000000000000000, 0.007781995580013368816 ) ) ;
#6031 = FACE_OUTER_BOUND ( 'NONE', #20733, .T. ) ;
#6032 = PLANE ( 'NONE',  #35785 ) ;
#6033 = DIRECTION ( 'NONE',  ( 0.007781995580012663651, 0.000000000000000000, -0.9999697198139515519 ) ) ;
#6034 = DIRECTION ( 'NONE',  ( 0.6427681459581294776, -0.7660444431189769032, 0.005002170337467562802 ) ) ;
#6035 = LINE ( 'NONE', #54520, #56025 ) ;
#6036 = AXIS2_PLACEMENT_3D ( 'NONE', #37058, #27705, #2105 ) ;
#6037 = CARTESIAN_POINT ( 'NONE',  ( -68.68358996202969990, -9.704760845431907867, -6.471852447744065095 ) ) ;
#6038 = ORIENTED_EDGE ( 'NONE', *, *, #17459, .T. ) ;
#6039 = DIRECTION ( 'NONE',  ( -0.5449076811759708816, 0.6444004775717707689, 0.5364919789714475140 ) ) ;
#6040 = FACE_OUTER_BOUND ( 'NONE', #12927, .T. ) ;
#6041 = CARTESIAN_POINT ( 'NONE',  ( -67.10382889302627518, 2.688821387764050996E-14, -6.245432549308967296 ) ) ;
#6042 = ORIENTED_EDGE ( 'NONE', *, *, #11758, .F. ) ;
#6043 = DIRECTION ( 'NONE',  ( 0.7660212471507180654, -0.6427876096865404731, 0.005961354470445141482 ) ) ;
#6044 = FACE_OUTER_BOUND ( 'NONE', #49420, .T. ) ;
#6045 = VECTOR ( 'NONE', #8907, 999.9999999999998863 ) ;
#6046 = ORIENTED_EDGE ( 'NONE', *, *, #26162, .F. ) ;
#6047 = ADVANCED_FACE ( 'NONE', ( #3805 ), #387, .F. ) ;
#6048 = VECTOR ( 'NONE', #361, 1000.000000000000227 ) ;
#6049 = LINE ( 'NONE', #32151, #10464 ) ;
#6050 = EDGE_CURVE ( 'NONE', #5827, #32592, #39604, .T. ) ;
#6051 = CARTESIAN_POINT ( 'NONE',  ( -9.542064456761055524, 0.000000000000000000, 10.59726798936431180 ) ) ;
#6052 = LINE ( 'NONE', #10845, #15649 ) ;
#6053 = EDGE_LOOP ( 'NONE', ( #28188, #12542, #41951, #802 ) ) ;
#6054 = VECTOR ( 'NONE', #15251, 999.9999999999998863 ) ;
#6055 = EDGE_CURVE ( 'NONE', #47084, #18846, #47541, .T. ) ;
#6056 = ORIENTED_EDGE ( 'NONE', *, *, #12795, .F. ) ;
#6057 = ADVANCED_FACE ( 'NONE', ( #8354 ), #33921, .F. ) ;
#6058 = PLANE ( 'NONE',  #47691 ) ;
#6059 = LINE ( 'NONE', #44370, #53186 ) ;
#6060 = EDGE_CURVE ( 'NONE', #1131, #54483, #29694, .T. ) ;
#6061 = ADVANCED_FACE ( 'NONE', ( #4397 ), #21710, .F. ) ;
#6062 = EDGE_CURVE ( 'NONE', #16128, #2320, #31348, .T. ) ;
#6063 = LINE ( 'NONE', #53453, #29331 ) ;
#6065 = PLANE ( 'NONE',  #22856 ) ;
#6064 = AXIS2_PLACEMENT_3D ( 'NONE', #36816, #32803, #23472 ) ;
#6066 = ORIENTED_EDGE ( 'NONE', *, *, #44117, .F. ) ;
#6067 = LINE ( 'NONE', #6585, #19454 ) ;
#6068 = ORIENTED_EDGE ( 'NONE', *, *, #6327, .T. ) ;
#6069 = CARTESIAN_POINT ( 'NONE',  ( -13.08330893211609869, 0.000000000000000000, 1.763933231766363630 ) ) ;
#6070 = VECTOR ( 'NONE', #16964, 999.9999999999998863 ) ;
#6071 = AXIS2_PLACEMENT_3D ( 'NONE', #44704, #41001, #52951 ) ;
#6072 = CARTESIAN_POINT ( 'NONE',  ( -20.54204810873173415, 0.000000000000000000, 4.860550213503115558 ) ) ;
#6073 = ORIENTED_EDGE ( 'NONE', *, *, #10422, .F. ) ;
#6074 = DIRECTION ( 'NONE',  ( -0.6427681459581293666, -0.7660444431189770143, -0.005002170337467561935 ) ) ;
#6075 = LINE ( 'NONE', #32997, #45015 ) ;
#6076 = CARTESIAN_POINT ( 'NONE',  ( -13.76498388619131852, 0.1245042932765033361, 2.432441075759850690 ) ) ;
#6077 = ORIENTED_EDGE ( 'NONE', *, *, #37510, .T. ) ;
#6078 = DIRECTION ( 'NONE',  ( 0.007781995580012663651, -3.146120232559066537E-19, -0.9999697198139514409 ) ) ;
#6079 = EDGE_CURVE ( 'NONE', #18980, #34834, #23105, .T. ) ;
#6080 = VERTEX_POINT ( 'NONE', #44392 ) ;
#6081 = AXIS2_PLACEMENT_3D ( 'NONE', #8583, #11970, #34416 ) ;
#6083 = VERTEX_POINT ( 'NONE', #27644 ) ;
#6082 = EDGE_CURVE ( 'NONE', #33009, #27645, #1778, .T. ) ;
#6084 = ORIENTED_EDGE ( 'NONE', *, *, #10177, .F. ) ;
#6085 = CARTESIAN_POINT ( 'NONE',  ( -50.27554558092695913, 4.209026340267034705, 5.000000000000000000 ) ) ;
#6086 = EDGE_CURVE ( 'NONE', #3178, #51656, #18259, .T. ) ;
#6087 = VERTEX_POINT ( 'NONE', #48366 ) ;
#6088 = DIRECTION ( 'NONE',  ( 0.5364919789714477361, 0.6444004775717706579, 0.5449076811759711036 ) ) ;
#6089 = PRODUCT_DEFINITION_SHAPE ( 'NONE', 'NONE',  #46837 ) ;
#6090 = EDGE_LOOP ( 'NONE', ( #37489, #8324, #27160, #40780 ) ) ;
#6091 = DIRECTION ( 'NONE',  ( -0.000000000000000000, -0.000000000000000000, 1.000000000000000000 ) ) ;
#6092 = DIRECTION ( 'NONE',  ( 0.9999697198139515519, 0.000000000000000000, 0.007781995580013368816 ) ) ;
#6093 = ADVANCED_FACE ( 'NONE', ( #32186 ), #6340, .F. ) ;
#6094 = ORIENTED_EDGE ( 'NONE', *, *, #34226, .F. ) ;
#6095 = AXIS2_PLACEMENT_3D ( 'NONE', #52676, #43353, #13779 ) ;
#6096 = DIRECTION ( 'NONE',  ( 0.9999697198139515519, 0.000000000000000000, 0.007781995580013368816 ) ) ;
#6097 = VERTEX_POINT ( 'NONE', #9476 ) ;
#6098 = AXIS2_PLACEMENT_3D ( 'NONE', #52656, #26020, #51820 ) ;
#6099 = PLANE ( 'NONE',  #55493 ) ;
#6100 = CARTESIAN_POINT ( 'NONE',  ( 2.072287782118878319, 0.000000000000000000, -2.950529333540147015 ) ) ;
#6101 = CARTESIAN_POINT ( 'NONE',  ( -21.06965149344186372, 20.49370688441071664, -4.657437592157546824 ) ) ;
#6102 = PLANE ( 'NONE',  #26627 ) ;
#6103 = PLANE ( 'NONE',  #39580 ) ;
#6104 = DIRECTION ( 'NONE',  ( 0.000000000000000000, -0.000000000000000000, -1.000000000000000000 ) ) ;
#6105 = LINE ( 'NONE', #23405, #15677 ) ;
#6106 = ORIENTED_EDGE ( 'NONE', *, *, #16165, .F. ) ;
#6107 = ORIENTED_EDGE ( 'NONE', *, *, #52906, .T. ) ;
#6108 = AXIS2_PLACEMENT_3D ( 'NONE', #20927, #3895, #25481 ) ;
#6109 = CARTESIAN_POINT ( 'NONE',  ( -16.47051635532609737, 0.000000000000000000, 5.261567884864613909 ) ) ;
#6110 = CARTESIAN_POINT ( 'NONE',  ( -15.28246537544034922, -2.137015261443158565, 6.125366393289809253 ) ) ;
#6111 = LINE ( 'NONE', #25626, #4353 ) ;
#6112 = VECTOR ( 'NONE', #41220, 1000.000000000000000 ) ;
#6113 = CARTESIAN_POINT ( 'NONE',  ( -9.075990533167328067, 0.000000000000000000, 10.41622904950343909 ) ) ;
#6114 = VERTEX_POINT ( 'NONE', #53220 ) ;
#6115 = CARTESIAN_POINT ( 'NONE',  ( -12.70458494993575194, -0.1191753592594197858, 11.86531876794841978 ) ) ;
#6116 = CARTESIAN_POINT ( 'NONE',  ( -61.21055533376208757, 7.871010810323348039, -3.000000000000007105 ) ) ;
#6117 = ORIENTED_EDGE ( 'NONE', *, *, #50563, .F. ) ;
#6118 = FACE_OUTER_BOUND ( 'NONE', #48750, .T. ) ;
#6119 = CARTESIAN_POINT ( 'NONE',  ( -16.30345465431069485, 0.000000000000000000, 9.494846779111002277 ) ) ;
#6120 = ORIENTED_EDGE ( 'NONE', *, *, #49303, .T. ) ;
#6121 = CARTESIAN_POINT ( 'NONE',  ( -67.86011035204582242, -8.871290095601276349, 5.504334939579316632 ) ) ;
#6122 = DIRECTION ( 'NONE',  ( 0.007781995580012662783, 0.000000000000000000, -0.9999697198139514409 ) ) ;
#6123 = PLANE ( 'NONE',  #3237 ) ;
#6124 = DIRECTION ( 'NONE',  ( -0.005002170337468016433, -0.7660444431189770143, 0.6427681459581293666 ) ) ;
#6125 = DIRECTION ( 'NONE',  ( 0.5449076811759707706, 0.6444004775717708799, -0.5364919789714476250 ) ) ;
#6126 = ORIENTED_EDGE ( 'NONE', *, *, #2013, .F. ) ;
#6127 = ORIENTED_EDGE ( 'NONE', *, *, #25714, .F. ) ;
#6128 = DIRECTION ( 'NONE',  ( 0.000000000000000000, -1.000000000000000000, 0.000000000000000000 ) ) ;
#6129 = DIRECTION ( 'NONE',  ( 0.005002170337468016433, -0.7660444431189770143, -0.6427681459581293666 ) ) ;
#6130 = CARTESIAN_POINT ( 'NONE',  ( -17.74404816805336793, 0.000000000000000000, 3.574322630375089460 ) ) ;
#6131 = EDGE_CURVE ( 'NONE', #31029, #33959, #9779, .T. ) ;
#6132 = ADVANCED_FACE ( 'NONE', ( #10626 ), #5493, .F. ) ;
#6133 = LINE ( 'NONE', #23437, #4699 ) ;
#6134 = CARTESIAN_POINT ( 'NONE',  ( -19.99988053418094935, 2.553033558614008047, 4.369109392650745605 ) ) ;
#6136 = EDGE_CURVE ( 'NONE', #32655, #11685, #31891, .T. ) ;
#6135 = ORIENTED_EDGE ( 'NONE', *, *, #8949, .T. ) ;
#6137 = DIRECTION ( 'NONE',  ( 0.000000000000000000, -0.000000000000000000, -1.000000000000000000 ) ) ;
#6138 = DIRECTION ( 'NONE',  ( 0.9999697198139515519, 0.000000000000000000, 0.007781995580013368816 ) ) ;
#6140 = VECTOR ( 'NONE', #33605, 999.9999999999998863 ) ;
#6139 = CARTESIAN_POINT ( 'NONE',  ( -16.43317633868556626, -0.1191753592594197858, 13.31363028683540151 ) ) ;
#6141 = DIRECTION ( 'NONE',  ( 0.9999697198139515519, 0.000000000000000000, 0.007781995580013368816 ) ) ;
#6142 = ORIENTED_EDGE ( 'NONE', *, *, #10565, .T. ) ;
#6143 = LINE ( 'NONE', #27138, #27479 ) ;
#6144 = ORIENTED_EDGE ( 'NONE', *, *, #37958, .T. ) ;
#6145 = FACE_OUTER_BOUND ( 'NONE', #33341, .T. ) ;
#6146 = DIRECTION ( 'NONE',  ( -0.5364919789714478471, 0.6444004775717705469, -0.5449076811759709926 ) ) ;
#6147 = ORIENTED_EDGE ( 'NONE', *, *, #49213, .T. ) ;
#6148 = VECTOR ( 'NONE', #51551, 1000.000000000000227 ) ;
#6149 = LINE ( 'NONE', #48438, #9098 ) ;
#6150 = VERTEX_POINT ( 'NONE', #27086 ) ;
#6151 = EDGE_CURVE ( 'NONE', #1256, #42362, #44973, .T. ) ;
#6152 = VERTEX_POINT ( 'NONE', #18558 ) ;
#6153 = ORIENTED_EDGE ( 'NONE', *, *, #28187, .T. ) ;
#6154 = CARTESIAN_POINT ( 'NONE',  ( -30.55480944230645690, 15.01744838932757276, 4.775844711708173485 ) ) ;
#6155 = EDGE_LOOP ( 'NONE', ( #6680, #37340, #30470, #48577 ) ) ;
#6156 = EDGE_CURVE ( 'NONE', #11345, #18640, #27, .T. ) ;
#6157 = ORIENTED_EDGE ( 'NONE', *, *, #30261, .T. ) ;
#6158 = LINE ( 'NONE', #41599, #15680 ) ;
#6159 = DIRECTION ( 'NONE',  ( 0.6427681459581294776, -0.7660444431189769032, 0.005002170337467562802 ) ) ;
#6160 = ORIENTED_EDGE ( 'NONE', *, *, #53723, .T. ) ;
#6161 = ADVANCED_FACE ( 'NONE', ( #53741 ), #14858, .F. ) ;
#6162 = VERTEX_POINT ( 'NONE', #39858 ) ;
#6163 = CARTESIAN_POINT ( 'NONE',  ( -25.20123094555300369, 0.000000000000000000, 6.470945668149052032 ) ) ;
#6164 = VERTEX_POINT ( 'NONE', #44127 ) ;
#6165 = ORIENTED_EDGE ( 'NONE', *, *, #19215, .T. ) ;
#6166 = ADVANCED_FACE ( 'NONE', ( #5240 ), #14322, .F. ) ;
#6167 = PLANE ( 'NONE',  #44681 ) ;
#6168 = DIRECTION ( 'NONE',  ( 0.7660212471507180654, -0.6427876096865404731, 0.005961354470445141482 ) ) ;
#6169 = CARTESIAN_POINT ( 'NONE',  ( -16.00013135147444387, 0.000000000000000000, 4.526564390117095549 ) ) ;
#6170 = CARTESIAN_POINT ( 'NONE',  ( -18.15050602765391119, 0.000000000000000000, 8.003144319007907015 ) ) ;
#6171 = EDGE_CURVE ( 'NONE', #8281, #35209, #27344, .T. ) ;
#6172 = EDGE_LOOP ( 'NONE', ( #1059, #50608, #38921, #8908 ) ) ;
#6173 = LINE ( 'NONE', #53556, #48226 ) ;
#6174 = VERTEX_POINT ( 'NONE', #54868 ) ;
#6175 = LINE ( 'NONE', #23734, #26648 ) ;
#6176 = FACE_OUTER_BOUND ( 'NONE', #25161, .T. ) ;
#6177 = LINE ( 'NONE', #24785, #13211 ) ;
#6178 = DIRECTION ( 'NONE',  ( -0.5449076811759708816, 0.6444004775717707689, 0.5364919789714475140 ) ) ;
#6179 = PLANE ( 'NONE',  #40242 ) ;
#6180 = LINE ( 'NONE', #42730, #46761 ) ;
#6181 = ORIENTED_EDGE ( 'NONE', *, *, #45855, .F. ) ;
#6182 = LINE ( 'NONE', #52719, #29249 ) ;
#6183 = VERTEX_POINT ( 'NONE', #7436 ) ;
#6184 = AXIS2_PLACEMENT_3D ( 'NONE', #13142, #17678, #35289 ) ;
#6185 = CARTESIAN_POINT ( 'NONE',  ( -17.46532115785441519, 0.000000000000000000, 13.67492996699914265 ) ) ;
#6186 = CARTESIAN_POINT ( 'NONE',  ( -17.93777409820730639, -3.108426967578162170, 3.749786651630157230 ) ) ;
#6187 = CARTESIAN_POINT ( 'NONE',  ( -12.63827574153160072, -0.1191753592594188005, 3.344727890296471440 ) ) ;
#6188 = LINE ( 'NONE', #7269, #39491 ) ;
#6189 = FACE_OUTER_BOUND ( 'NONE', #5178, .T. ) ;
#6190 = FACE_OUTER_BOUND ( 'NONE', #12308, .T. ) ;
#6191 = ORIENTED_EDGE ( 'NONE', *, *, #48311, .T. ) ;
#6192 = LINE ( 'NONE', #49873, #2179 ) ;
#6193 = CARTESIAN_POINT ( 'NONE',  ( -16.43317633868556626, -0.1191753592594197858, 13.31363028683540151 ) ) ;
#6194 = DIRECTION ( 'NONE',  ( 0.007781995580012663651, -3.146120232559066537E-19, -0.9999697198139514409 ) ) ;
#6195 = ADVANCED_FACE ( 'NONE', ( #40960, #24763 ), #15980, .T. ) ;
#6196 = CARTESIAN_POINT ( 'NONE',  ( -68.07613967535824884, 1.957879731433807224, -7.460487485314824418 ) ) ;
#6197 = CARTESIAN_POINT ( 'NONE',  ( -22.40556560354864146, -0.1191753592594197858, 5.484709000965211523 ) ) ;
#6198 = ADVANCED_FACE ( 'NONE', ( #36722 ), #2349, .F. ) ;
#6199 = CARTESIAN_POINT ( 'NONE',  ( 2.602374448188125350E-16, -1.000000000000000000, -2.125000000000000000 ) ) ;
#6200 = EDGE_CURVE ( 'NONE', #19740, #2262, #6610, .T. ) ;
#6201 = DIRECTION ( 'NONE',  ( -0.6427681459581293666, -0.7660444431189770143, -0.005002170337467561935 ) ) ;
#6202 = LINE ( 'NONE', #44798, #41414 ) ;
#6203 = LINE ( 'NONE', #45100, #44659 ) ;
#6204 = EDGE_LOOP ( 'NONE', ( #5550, #29246, #15960 ) ) ;
#6205 = ORIENTED_EDGE ( 'NONE', *, *, #43723, .T. ) ;
#6206 = ORIENTED_EDGE ( 'NONE', *, *, #31930, .F. ) ;
#6207 = EDGE_LOOP ( 'NONE', ( #15127, #34480, #55334, #38164 ) ) ;
#6208 = EDGE_LOOP ( 'NONE', ( #14902, #5939, #43075, #20128 ) ) ;
#6209 = EDGE_LOOP ( 'NONE', ( #16597, #29700, #5620, #37769 ) ) ;
#6210 = LINE ( 'NONE', #27485, #9708 ) ;
#6211 = LINE ( 'NONE', #23516, #47583 ) ;
#6212 = VECTOR ( 'NONE', #50708, 999.9999999999998863 ) ;
#6213 = ORIENTED_EDGE ( 'NONE', *, *, #30689, .F. ) ;
#6214 = ORIENTED_EDGE ( 'NONE', *, *, #25445, .T. ) ;
#6215 = ORIENTED_EDGE ( 'NONE', *, *, #54418, .F. ) ;
#6216 = EDGE_CURVE ( 'NONE', #17655, #5535, #6910, .T. ) ;
#6217 = CARTESIAN_POINT ( 'NONE',  ( -68.75873835633035469, -8.975997488099570987, -7.041125024101304142 ) ) ;
#6218 = EDGE_CURVE ( 'NONE', #27279, #33543, #41790, .T. ) ;
#6219 = DIRECTION ( 'NONE',  ( 0.9999697198139515519, 0.000000000000000000, 0.007781995580013368816 ) ) ;
#6220 = PLANE ( 'NONE',  #4189 ) ;
#6221 = EDGE_CURVE ( 'NONE', #14352, #31046, #24474, .T. ) ;
#6222 = ORIENTED_EDGE ( 'NONE', *, *, #25450, .F. ) ;
#6223 = CARTESIAN_POINT ( 'NONE',  ( -17.88298902127032619, 0.000000000000000000, 7.635894128402147096 ) ) ;
#6224 = ORIENTED_EDGE ( 'NONE', *, *, #37633, .F. ) ;
#6225 = CARTESIAN_POINT ( 'NONE',  ( -19.35672695474844218, 0.000000000000000000, 4.300436530774871535 ) ) ;
#6226 = ADVANCED_FACE ( 'NONE', ( #28765 ), #11137, .F. ) ;
#6227 = DIRECTION ( 'NONE',  ( 0.6427681459581294776, -0.7660444431189769032, 0.005002170337467562802 ) ) ;
#6228 = CARTESIAN_POINT ( 'NONE',  ( -18.09799117768911003, 0.2864062442990034651, 4.381236941275065355 ) ) ;
#6229 = FACE_OUTER_BOUND ( 'NONE', #47798, .T. ) ;
#6230 = DIRECTION ( 'NONE',  ( 0.000000000000000000, -1.000000000000000000, 0.000000000000000000 ) ) ;
#6231 = DIRECTION ( 'NONE',  ( 0.007781995580012662783, 0.000000000000000000, -0.9999697198139514409 ) ) ;
#6232 = DIRECTION ( 'NONE',  ( -0.005002170337468016433, -0.7660444431189770143, 0.6427681459581293666 ) ) ;
#6233 = ORIENTED_EDGE ( 'NONE', *, *, #39223, .T. ) ;
#6234 = DIRECTION ( 'NONE',  ( 0.6427681459581294776, -0.7660444431189769032, 0.005002170337467562802 ) ) ;
#6235 = EDGE_LOOP ( 'NONE', ( #12749, #11486, #2764, #49889, #8798, #34469, #63 ) ) ;
#6236 = LINE ( 'NONE', #15302, #36523 ) ;
#6237 = CARTESIAN_POINT ( 'NONE',  ( -17.56606728872570500, 2.391131607591507446, 7.628832529946389052 ) ) ;
#6238 = LINE ( 'NONE', #23542, #36757 ) ;
#6239 = LINE ( 'NONE', #11024, #37736 ) ;
#6240 = DIRECTION ( 'NONE',  ( -0.005002170337468016433, -0.7660444431189770143, 0.6427681459581293666 ) ) ;
#6241 = CARTESIAN_POINT ( 'NONE',  ( -16.47758211672594086, 0.000000000000000000, 6.169503050675118061 ) ) ;
#6243 = ADVANCED_FACE ( 'NONE', ( #2882 ), #24222, .F. ) ;
#6242 = LINE ( 'NONE', #33402, #30698 ) ;
#6244 = DIRECTION ( 'NONE',  ( 0.6427681459581294776, -0.7660444431189769032, 0.005002170337467562802 ) ) ;
#6245 = DIRECTION ( 'NONE',  ( -0.7660212471507179544, -0.6427876096865405842, -0.005961354470445141482 ) ) ;
#6246 = ORIENTED_EDGE ( 'NONE', *, *, #28972, .T. ) ;
#6247 = DIRECTION ( 'NONE',  ( 0.8531650599175529814, -0.4028455766673920135, -0.3313982828793697877 ) ) ;
#6248 = CARTESIAN_POINT ( 'NONE',  ( -13.16056798344334133, -0.03739765774599676518, 1.931956729131618200 ) ) ;
#6249 = EDGE_CURVE ( 'NONE', #20652, #33216, #20212, .T. ) ;
#6250 = CARTESIAN_POINT ( 'NONE',  ( -69.30403031588791407, -1.000000000000000666, -6.450409451741321298 ) ) ;
#6251 = CARTESIAN_POINT ( 'NONE',  ( -18.54007560369215568, -3.270328918600661883, 3.978575490718303520 ) ) ;
#6252 = AXIS2_PLACEMENT_3D ( 'NONE', #8318, #8616, #25948 ) ;
#6253 = ADVANCED_FACE ( 'NONE', ( #28181 ), #19682, .F. ) ;
#6254 = FACE_OUTER_BOUND ( 'NONE', #3019, .T. ) ;
#6255 = CARTESIAN_POINT ( 'NONE',  ( -29.86274838104827367, -0.1191753592594197858, 8.381332038739175871 ) ) ;
#6256 = DIRECTION ( 'NONE',  ( 0.005002170337468016433, -0.7660444431189770143, -0.6427681459581293666 ) ) ;
#6257 = ADVANCED_FACE ( 'NONE', ( #20519 ), #37847, .F. ) ;
#6258 = DIRECTION ( 'NONE',  ( 0.9999697198139515519, 0.000000000000000000, 0.007781995580013368816 ) ) ;
#6259 = ORIENTED_EDGE ( 'NONE', *, *, #7028, .F. ) ;
#6260 = ORIENTED_EDGE ( 'NONE', *, *, #19519, .T. ) ;
#6261 = CARTESIAN_POINT ( 'NONE',  ( -24.26908309836554878, 0.000000000000000000, 6.108867788427308376 ) ) ;
#6262 = PLANE ( 'NONE',  #18680 ) ;
#6263 = B_SPLINE_CURVE_WITH_KNOTS ( 'NONE', 3,
 ( #10723, #10967, #1330, #28286 ),
 .UNSPECIFIED., .F., .F.,
 ( 4, 4 ),
 ( 0.0002184642560491729404, 0.0003536952807433174899 ),
 .UNSPECIFIED. ) ;
#6264 = EDGE_CURVE ( 'NONE', #45853, #24338, #37005, .T. ) ;
#6265 = EDGE_LOOP ( 'NONE', ( #43088, #269, #33748, #35392 ) ) ;
#6266 = PLANE ( 'NONE',  #5934 ) ;
#6267 = VERTEX_POINT ( 'NONE', #33562 ) ;
#6268 = DIRECTION ( 'NONE',  ( 0.000000000000000000, 0.000000000000000000, -1.000000000000000000 ) ) ;
#6269 = ADVANCED_FACE ( 'NONE', ( #46622 ), #41256, .F. ) ;
#6270 = VERTEX_POINT ( 'NONE', #19939 ) ;
#6271 = ORIENTED_EDGE ( 'NONE', *, *, #47171, .F. ) ;
#6272 = VERTEX_POINT ( 'NONE', #32718 ) ;
#6273 = FACE_OUTER_BOUND ( 'NONE', #26902, .T. ) ;
#6274 = PLANE ( 'NONE',  #54083 ) ;
#6275 = CARTESIAN_POINT ( 'NONE',  ( -9.542064456761055524, 0.000000000000000000, 10.59726798936431180 ) ) ;
#6276 = ORIENTED_EDGE ( 'NONE', *, *, #24919, .F. ) ;
#6277 = ORIENTED_EDGE ( 'NONE', *, *, #6839, .F. ) ;
#6278 = LINE ( 'NONE', #49137, #49956 ) ;
#6279 = EDGE_LOOP ( 'NONE', ( #40336, #44542, #12761, #8799 ) ) ;
#6280 = DIRECTION ( 'NONE',  ( -0.6427681459581293666, -0.7660444431189770143, -0.005002170337467561935 ) ) ;
#6281 = VERTEX_POINT ( 'NONE', #37260 ) ;
#6282 = CARTESIAN_POINT ( 'NONE',  ( 2.072287782118878319, 0.000000000000000000, -2.950529333540147015 ) ) ;
#6283 = CARTESIAN_POINT ( 'NONE',  ( 4.866417447938705898, 0.000000000000000000, -1.967953638240998337 ) ) ;
#6284 = COLOUR_RGB ( '', 0.66274510, 0.83137255, 0.94901961) ;
#6285 = EDGE_LOOP ( 'NONE', ( #32260, #18290, #26734, #5035 ) ) ;
#6286 = DIRECTION ( 'NONE',  ( -0.9999697198139514409, -0.000000000000000000, -0.007781995580013368816 ) ) ;
#6287 = ADVANCED_FACE ( 'NONE', ( #54561 ), #15671, .F. ) ;
#6288 = DIRECTION ( 'NONE',  ( -0.005961354470445682716, -0.6427876096865404731, 0.7660212471507180654 ) ) ;
#6289 = EDGE_LOOP ( 'NONE', ( #12183, #55459, #41428, #35829, #17218 ) ) ;
#6290 = CARTESIAN_POINT ( 'NONE',  ( -11.22056963685719211, 0.000000000000000000, 1.239771416285661010 ) ) ;
#6291 = CARTESIAN_POINT ( 'NONE',  ( -9.518333015441259093, -1.607988201085719160, 2.489039940304945020 ) ) ;
#6292 = DIRECTION ( 'NONE',  ( 0.007781995580012663651, -3.146120232559066537E-19, -0.9999697198139514409 ) ) ;
#6293 = ORIENTED_EDGE ( 'NONE', *, *, #22198, .F. ) ;
#6294 = EDGE_CURVE ( 'NONE', #11120, #19445, #16820, .T. ) ;
#6295 = DIRECTION ( 'NONE',  ( 0.5449076811759707706, 0.6444004775717708799, -0.5364919789714476250 ) ) ;
#6296 = CARTESIAN_POINT ( 'NONE',  ( -10.94028622754223967, 0.000000000000000000, 11.14038480894692995 ) ) ;
#6297 = CARTESIAN_POINT ( 'NONE',  ( -16.36974118378670084, -0.1191753592594190225, 5.162349112441218857 ) ) ;
#6298 = DIRECTION ( 'NONE',  ( 0.000000000000000000, -1.000000000000000000, 0.000000000000000000 ) ) ;
#6299 = EDGE_CURVE ( 'NONE', #2679, #18318, #30451, .T. ) ;
#6300 = DIRECTION ( 'NONE',  ( 0.7660212471507180654, -0.6427876096865404731, 0.005961354470445141482 ) ) ;
#6302 = ADVANCED_FACE ( 'NONE', ( #25069 ), #23, .F. ) ;
#6301 = CARTESIAN_POINT ( 'NONE',  ( -27.06630483948590893, -0.1191753592594197858, 7.295098399573937797 ) ) ;
#6303 = CARTESIAN_POINT ( 'NONE',  ( -66.80596856838349140, -11.36862731764621515, 7.586268967159024434 ) ) ;
#6304 = ORIENTED_EDGE ( 'NONE', *, *, #3965, .F. ) ;
#6305 = LINE ( 'NONE', #18220, #54299 ) ;
#6306 = CARTESIAN_POINT ( 'NONE',  ( -12.73042875255514872, 0.000000000000000000, 2.336017552946574760 ) ) ;
#6307 = CARTESIAN_POINT ( 'NONE',  ( -66.43438701333805341, -1.405445106517288831E-11, -0.3573205173190009409 ) ) ;
#6308 = ORIENTED_EDGE ( 'NONE', *, *, #54239, .F. ) ;
#6309 = DIRECTION ( 'NONE',  ( 0.007781995580012662783, 0.000000000000000000, -0.9999697198139514409 ) ) ;
#6310 = DIRECTION ( 'NONE',  ( 0.9999697198139515519, 0.000000000000000000, 0.007781995580013368816 ) ) ;
#6311 = ADVANCED_FACE ( 'NONE', ( #47467 ), #29878, .F. ) ;
#6312 = CARTESIAN_POINT ( 'NONE',  ( -15.12407731238180730, 1.743523803501506375, 2.501009437766517518 ) ) ;
#6313 = LINE ( 'NONE', #36147, #22404 ) ;
#6314 = EDGE_CURVE ( 'NONE', #51395, #17188, #47772, .T. ) ;
#6315 = DIRECTION ( 'NONE',  ( 0.5449076811759707706, 0.6444004775717708799, -0.5364919789714476250 ) ) ;
#6316 = VERTEX_POINT ( 'NONE', #51467 ) ;
#6317 = ORIENTED_EDGE ( 'NONE', *, *, #53780, .T. ) ;
#6318 = DIRECTION ( 'NONE',  ( 0.005961354470445682716, -0.6427876096865404731, -0.7660212471507180654 ) ) ;
#6319 = FACE_OUTER_BOUND ( 'NONE', #1900, .T. ) ;
#6320 = PLANE ( 'NONE',  #10285 ) ;
#6321 = ADVANCED_FACE ( 'NONE', ( #8876 ), #21359, .T. ) ;
#6322 = AXIS2_PLACEMENT_3D ( 'NONE', #35709, #48783, #9878 ) ;
#6323 = EDGE_LOOP ( 'NONE', ( #49344, #38488, #17950, #23446 ) ) ;
#6324 = CARTESIAN_POINT ( 'NONE',  ( -10.74029228357944987, 0.000000000000000000, 11.14194120806293320 ) ) ;
#6325 = ORIENTED_EDGE ( 'NONE', *, *, #10800, .F. ) ;
#6326 = CARTESIAN_POINT ( 'NONE',  ( -19.32961685222932147, 0.000000000000000000, 14.39908572644263351 ) ) ;
#6327 = EDGE_CURVE ( 'NONE', #20518, #40648, #3472, .T. ) ;
#6328 = ORIENTED_EDGE ( 'NONE', *, *, #15330, .F. ) ;
#6329 = ORIENTED_EDGE ( 'NONE', *, *, #40063, .F. ) ;
#6330 = LINE ( 'NONE', #31880, #32025 ) ;
#6331 = CARTESIAN_POINT ( 'NONE',  ( -16.86311861568060877, -0.1191753592594181482, 8.851830233250854718 ) ) ;
#6332 = LINE ( 'NONE', #19373, #9436 ) ;
#6333 = VERTEX_POINT ( 'NONE', #3735 ) ;
#6334 = FACE_OUTER_BOUND ( 'NONE', #17083, .T. ) ;
#6335 = EDGE_LOOP ( 'NONE', ( #55920, #17801, #29057, #35026 ) ) ;
#6336 = EDGE_LOOP ( 'NONE', ( #20328, #37787, #17576, #54888 ) ) ;
#6337 = ORIENTED_EDGE ( 'NONE', *, *, #25353, .F. ) ;
#6338 = FACE_OUTER_BOUND ( 'NONE', #41596, .T. ) ;
#6339 = ORIENTED_EDGE ( 'NONE', *, *, #51028, .F. ) ;
#6340 = PLANE ( 'NONE',  #32967 ) ;
#6342 = EDGE_CURVE ( 'NONE', #47897, #8966, #3987, .T. ) ;
#6341 = ORIENTED_EDGE ( 'NONE', *, *, #46449, .F. ) ;
#6343 = CARTESIAN_POINT ( 'NONE',  ( -15.60102546347950536, 0.000000000000000000, 12.95077420755565356 ) ) ;
#6344 = DIRECTION ( 'NONE',  ( -0.005961354470445682716, -0.6427876096865404731, 0.7660212471507180654 ) ) ;
#6345 = EDGE_LOOP ( 'NONE', ( #4392, #36710, #4453, #39835 ) ) ;
#6346 = PLANE ( 'NONE',  #52208 ) ;
#6347 = ADVANCED_FACE ( 'NONE', ( #51717 ), #34993, .F. ) ;
#6348 = ORIENTED_EDGE ( 'NONE', *, *, #49291, .T. ) ;
#6349 = LINE ( 'NONE', #22821, #20096 ) ;
#6350 = ADVANCED_FACE ( 'NONE', ( #25910 ), #17354, .F. ) ;
#6351 = LINE ( 'NONE', #15413, #17535 ) ;
#6352 = DIRECTION ( 'NONE',  ( 0.005002170337468016433, -0.7660444431189770143, -0.6427681459581293666 ) ) ;
#6353 = CARTESIAN_POINT ( 'NONE',  ( -15.13495153988577968, 0.000000000000000000, 12.76973526769478084 ) ) ;
#6354 = LINE ( 'NONE', #45506, #15092 ) ;
#6355 = DIRECTION ( 'NONE',  ( -0.2426528472758542054, 0.7422098413412800966, -0.6246952433987894571 ) ) ;
#6356 = DIRECTION ( 'NONE',  ( 0.000000000000000000, -1.000000000000000000, 0.000000000000000000 ) ) ;
#6357 = VERTEX_POINT ( 'NONE', #17654 ) ;
#6358 = EDGE_CURVE ( 'NONE', #37343, #49895, #4587, .T. ) ;
#6359 = ADVANCED_FACE ( 'NONE', ( #34414 ), #4334, .F. ) ;
#6360 = EDGE_CURVE ( 'NONE', #36106, #46689, #13411, .T. ) ;
#6361 = ORIENTED_EDGE ( 'NONE', *, *, #4124, .F. ) ;
#6362 = DIRECTION ( 'NONE',  ( 0.7660212471507180654, -0.6427876096865404731, 0.005961354470445141482 ) ) ;
#6363 = DIRECTION ( 'NONE',  ( -0.5449076811759708816, 0.6444004775717707689, 0.5364919789714475140 ) ) ;
#6364 = DIRECTION ( 'NONE',  ( 0.007781995580012663651, -3.146120232559066537E-19, -0.9999697198139514409 ) ) ;
#6366 = EDGE_CURVE ( 'NONE', #1256, #20039, #30725, .T. ) ;
#6365 = CARTESIAN_POINT ( 'NONE',  ( -13.08408713167409942, -0.1191753592594197858, 1.863930203747758085 ) ) ;
#6367 = CYLINDRICAL_SURFACE ( 'NONE', #37649, 1.750000000000003331 ) ;
#6368 = ORIENTED_EDGE ( 'NONE', *, *, #29237, .F. ) ;
#6369 = PLANE ( 'NONE',  #13144 ) ;
#6370 = LINE ( 'NONE', #11470, #53182 ) ;
#6371 = ORIENTED_EDGE ( 'NONE', *, *, #6602, .T. ) ;
#6372 = CARTESIAN_POINT ( 'NONE',  ( -19.60990026154428278, 0.000000000000000000, 4.498472333781370125 ) ) ;
#6373 = DIRECTION ( 'NONE',  ( 0.000000000000000000, -1.000000000000000000, 0.000000000000000000 ) ) ;
#6374 = ORIENTED_EDGE ( 'NONE', *, *, #38605, .F. ) ;
#6375 = CARTESIAN_POINT ( 'NONE',  ( -13.01806413347570590, 0.000000000000000000, 5.288435666356683384 ) ) ;
#6376 = DIRECTION ( 'NONE',  ( -0.9335804264972041855, 0.3583679495452941621, 0.000000000000000000 ) ) ;
#6377 = EDGE_CURVE ( 'NONE', #42918, #19378, #21054, .T. ) ;
#6378 = DIRECTION ( 'NONE',  ( 0.5364919789714477361, 0.6444004775717706579, 0.5449076811759711036 ) ) ;
#6379 = DIRECTION ( 'NONE',  ( -0.005002170337468016433, -0.7660444431189770143, 0.6427681459581293666 ) ) ;
#6380 = EDGE_CURVE ( 'NONE', #7777, #31631, #38386, .T. ) ;
#6381 = CARTESIAN_POINT ( 'NONE',  ( -17.87724091425976169, 0.000000000000000000, 6.897274721886618387 ) ) ;
#6382 = ORIENTED_EDGE ( 'NONE', *, *, #26319, .T. ) ;
#6383 = ORIENTED_EDGE ( 'NONE', *, *, #30907, .F. ) ;
#6384 = EDGE_CURVE ( 'NONE', #42368, #33896, #14256, .T. ) ;
#6385 = LINE ( 'NONE', #11187, #49339 ) ;
#6386 = LINE ( 'NONE', #44712, #18630 ) ;
#6387 = CARTESIAN_POINT ( 'NONE',  ( -18.75345506656806549, -0.03739765774599677212, 4.104424007462089463 ) ) ;
#6388 = ADVANCED_FACE ( 'NONE', ( #31568 ), #32116, .F. ) ;
#6389 = DIRECTION ( 'NONE',  ( -0.5364919789714478471, 0.6444004775717705469, -0.5449076811759709926 ) ) ;
#6390 = CARTESIAN_POINT ( 'NONE',  ( -1.246832498358330099E-15, 0.000000000000000000, 0.000000000000000000 ) ) ;
#6391 = ORIENTED_EDGE ( 'NONE', *, *, #47063, .T. ) ;
#6392 = CARTESIAN_POINT ( 'NONE',  ( 5.415767943939227891, -1.059274754233117344, -2.423176835373680227 ) ) ;
#6393 = VECTOR ( 'NONE', #27410, 1000.000000000000000 ) ;
#6394 = CARTESIAN_POINT ( 'NONE',  ( -18.67697421479882181, -0.1191753592594197858, 4.036397482078229793 ) ) ;
#6395 = CARTESIAN_POINT ( 'NONE',  ( -30.79489622823572859, -0.1191753592594197858, 8.743409918460921304 ) ) ;
#6396 = ORIENTED_EDGE ( 'NONE', *, *, #19581, .T. ) ;
#6397 = CARTESIAN_POINT ( 'NONE',  ( -30.79411802867772607, 0.000000000000000000, 8.643412946479525516 ) ) ;
#6398 = VERTEX_POINT ( 'NONE', #40644 ) ;
#6399 = FACE_OUTER_BOUND ( 'NONE', #34899, .T. ) ;
#6400 = CARTESIAN_POINT ( 'NONE',  ( -17.73140113748535285, 0.000000000000000000, 13.85752530597602039 ) ) ;
#6401 = EDGE_LOOP ( 'NONE', ( #21398, #41983, #37501, #37466 ) ) ;
#6402 = DIRECTION ( 'NONE',  ( 0.5449076811759707706, 0.6444004775717708799, -0.5364919789714476250 ) ) ;
#6403 = ORIENTED_EDGE ( 'NONE', *, *, #3975, .F. ) ;
#6404 = ORIENTED_EDGE ( 'NONE', *, *, #27785, .T. ) ;
#6405 = ORIENTED_EDGE ( 'NONE', *, *, #9455, .F. ) ;
#6406 = PLANE ( 'NONE',  #50210 ) ;
#6407 = VERTEX_POINT ( 'NONE', #9124 ) ;
#6408 = ORIENTED_EDGE ( 'NONE', *, *, #11879, .T. ) ;
#6409 = PLANE ( 'NONE',  #28377 ) ;
#6411 = ADVANCED_FACE ( 'NONE', ( #48290 ), #44892, .F. ) ;
#6410 = ORIENTED_EDGE ( 'NONE', *, *, #19360, .F. ) ;
#6412 = EDGE_LOOP ( 'NONE', ( #11903, #53625, #19750, #6084 ) ) ;
#6413 = LINE ( 'NONE', #10942, #44938 ) ;
#6414 = ORIENTED_EDGE ( 'NONE', *, *, #4962, .F. ) ;
#6415 = EDGE_CURVE ( 'NONE', #39023, #3706, #18193, .T. ) ;
#6416 = ORIENTED_EDGE ( 'NONE', *, *, #22324, .F. ) ;
#6417 = VERTEX_POINT ( 'NONE', #44330 ) ;
#6418 = ADVANCED_FACE ( 'NONE', ( #4869 ), #53147, .F. ) ;
#6419 = DIRECTION ( 'NONE',  ( -0.6427681459581293666, -0.7660444431189770143, -0.005002170337467561935 ) ) ;
#6420 = DIRECTION ( 'NONE',  ( 0.9999697198139515519, 0.000000000000000000, 0.007781995580013368816 ) ) ;
#6421 = CARTESIAN_POINT ( 'NONE',  ( -18.67697421479882181, -0.1191753592594197858, 4.036397482078229793 ) ) ;
#6422 = LINE ( 'NONE', #46144, #54031 ) ;
#6423 = ORIENTED_EDGE ( 'NONE', *, *, #22159, .F. ) ;
#6424 = CARTESIAN_POINT ( 'NONE',  ( -15.70177159435079695, 2.391131607591507446, 6.904676770502899075 ) ) ;
#6425 = ORIENTED_EDGE ( 'NONE', *, *, #12828, .F. ) ;
#6426 = EDGE_CURVE ( 'NONE', #11310, #21341, #22743, .T. ) ;
#6427 = EDGE_CURVE ( 'NONE', #47379, #40739, #26725, .T. ) ;
#6428 = ADVANCED_FACE ( 'NONE', ( #44051 ), #35524, .F. ) ;
#6429 = EDGE_LOOP ( 'NONE', ( #34279, #7161, #47602, #36465 ) ) ;
#6430 = AXIS2_PLACEMENT_3D ( 'NONE', #38621, #55359, #12210 ) ;
#6431 = LINE ( 'NONE', #14950, #51126 ) ;
#6432 = PRODUCT_DEFINITION_CONTEXT ( 'detailed design', #56163, 'design' ) ;
#6433 = ADVANCED_FACE ( 'NONE', ( #53413 ), #14512, .F. ) ;
#6434 = VECTOR ( 'NONE', #53706, 1000.000000000000000 ) ;
#6435 = CARTESIAN_POINT ( 'NONE',  ( -44.89558674184503673, 6.737796755050466935, -5.000000000000005329 ) ) ;
#6436 = CARTESIAN_POINT ( 'NONE',  ( -12.86480176444844581, -1.489407457353158160, 4.123429006776876626 ) ) ;
#6437 = CARTESIAN_POINT ( 'NONE',  ( -18.38240279575065017, -1.975113310420658852, 3.958654176621851484 ) ) ;
#6438 = LINE ( 'NONE', #19194, #11367 ) ;
#6439 = ORIENTED_EDGE ( 'NONE', *, *, #16301, .F. ) ;
#6440 = DIRECTION ( 'NONE',  ( 0.007781995580012663651, 0.000000000000000000, -0.9999697198139515519 ) ) ;
#6441 = ORIENTED_EDGE ( 'NONE', *, *, #39309, .T. ) ;
#6442 = DIRECTION ( 'NONE',  ( -0.7660212471507179544, -0.6427876096865405842, -0.005961354470445141482 ) ) ;
#6443 = PLANE ( 'NONE',  #2420 ) ;
#6444 = DIRECTION ( 'NONE',  ( -0.6427681459581293666, -0.7660444431189770143, -0.005002170337467561935 ) ) ;
#6445 = CARTESIAN_POINT ( 'NONE',  ( -9.872934393541347831, -0.1117717739994080611, 7.053356580378568275 ) ) ;
#6446 = ADVANCED_FACE ( 'NONE', ( #40059 ), #22191, .F. ) ;
#6447 = DIRECTION ( 'NONE',  ( 0.007781995580012663651, 0.000000000000000000, -0.9999697198139515519 ) ) ;
#6448 = VERTEX_POINT ( 'NONE', #43753 ) ;
#6449 = ADVANCED_FACE ( 'NONE', ( #1715 ), #53674, .F. ) ;
#6450 = CARTESIAN_POINT ( 'NONE',  ( -17.26532721389163072, 0.000000000000000000, 13.67648636611514590 ) ) ;
#6451 = CARTESIAN_POINT ( 'NONE',  ( 5.057731014323088026, -1.114607557371864122, 2.289010529401726668 ) ) ;
#6452 = DIRECTION ( 'NONE',  ( 0.005002170337468016433, -0.7660444431189770143, -0.6427681459581293666 ) ) ;
#6453 = EDGE_CURVE ( 'NONE', #20837, #22139, #52562, .T. ) ;
#6454 = VECTOR ( 'NONE', #36654, 1000.000000000000227 ) ;
#6455 = DIRECTION ( 'NONE',  ( 0.007781995580012662783, 0.000000000000000000, -0.9999697198139514409 ) ) ;
#6456 = DIRECTION ( 'NONE',  ( 0.7660212471507180654, -0.6427876096865404731, 0.005961354470445141482 ) ) ;
#6457 = PLANE ( 'NONE',  #36356 ) ;
#6458 = PLANE ( 'NONE',  #33791 ) ;
#6459 = EDGE_CURVE ( 'NONE', #21349, #48276, #30974, .T. ) ;
#6460 = CARTESIAN_POINT ( 'NONE',  ( -31.72626587586518099, 0.000000000000000000, 9.005490826201270949 ) ) ;
#6461 = CARTESIAN_POINT ( 'NONE',  ( -13.73672976910459909, 0.000000000000000000, 12.22661844811216270 ) ) ;
#6462 = EDGE_LOOP ( 'NONE', ( #50734, #31075, #54859, #38899 ) ) ;
#6463 = VECTOR ( 'NONE', #15837, 1000.000000000000227 ) ;
#6464 = VECTOR ( 'NONE', #24382, 1000.000000000000227 ) ;
#6465 = ORIENTED_EDGE ( 'NONE', *, *, #44254, .T. ) ;
#6466 = ORIENTED_EDGE ( 'NONE', *, *, #17915, .T. ) ;
#6467 = ORIENTED_EDGE ( 'NONE', *, *, #4691, .F. ) ;
#6468 = ORIENTED_EDGE ( 'NONE', *, *, #41551, .F. ) ;
#6469 = CARTESIAN_POINT ( 'NONE',  ( -21.47263955680318404, 0.000000000000000000, 5.022634149262071190 ) ) ;
#6470 = DIRECTION ( 'NONE',  ( -0.005961354470445682716, -0.6427876096865404731, 0.7660212471507180654 ) ) ;
#6471 = ORIENTED_EDGE ( 'NONE', *, *, #18532, .T. ) ;
#6472 = PLANE ( 'NONE',  #14985 ) ;
#6473 = ORIENTED_EDGE ( 'NONE', *, *, #3282, .T. ) ;
#6474 = ORIENTED_EDGE ( 'NONE', *, *, #30663, .T. ) ;
#6475 = CARTESIAN_POINT ( 'NONE',  ( -67.11552282731028640, -9.391017982635339933, -7.239294561908663717 ) ) ;
#6476 = DIRECTION ( 'NONE',  ( 0.000000000000000000, -0.000000000000000000, -1.000000000000000000 ) ) ;
#6477 = CARTESIAN_POINT ( 'NONE',  ( -16.06709938707323460, 0.000000000000000000, 13.13181314741652628 ) ) ;
#6478 = ORIENTED_EDGE ( 'NONE', *, *, #31397, .F. ) ;
#6479 = DIRECTION ( 'NONE',  ( 0.005002170337468016433, -0.7660444431189770143, -0.6427681459581293666 ) ) ;
#6480 = ADVANCED_FACE ( 'NONE', ( #13944 ), #31269, .F. ) ;
#6481 = AXIS2_PLACEMENT_3D ( 'NONE', #40618, #36621, #40871 ) ;
#6482 = VECTOR ( 'NONE', #23264, 1000.000000000000227 ) ;
#6483 = CARTESIAN_POINT ( 'NONE',  ( -10.77398004715669444, -0.1191753592594188005, 2.620572130852981907 ) ) ;
#6484 = DIRECTION ( 'NONE',  ( -0.005002170337468016433, -0.7660444431189770143, 0.6427681459581293666 ) ) ;
#6485 = ADVANCED_FACE ( 'NONE', ( #27023 ), #19878, .F. ) ;
#6486 = ADVANCED_FACE ( 'NONE', ( #24413 ), #2557, .F. ) ;
#6487 = CARTESIAN_POINT ( 'NONE',  ( -15.86710544311044302, 0.000000000000000000, 13.13336954653252953 ) ) ;
#6488 = FACE_OUTER_BOUND ( 'NONE', #14892, .T. ) ;
#6489 = CARTESIAN_POINT ( 'NONE',  ( -20.45041684859848630, 0.000000000000000000, 4.994449012483184625 ) ) ;
#6490 = CARTESIAN_POINT ( 'NONE',  ( -27.06630483948590893, -0.1191753592594197858, 7.295098399573937797 ) ) ;
#6491 = CARTESIAN_POINT ( 'NONE',  ( -16.51810710137574034, -1.975113310420659740, 3.234498417178360175 ) ) ;
#6492 = CARTESIAN_POINT ( 'NONE',  ( -17.26532721389163072, 0.000000000000000000, 13.67648636611514590 ) ) ;
#6493 = ORIENTED_EDGE ( 'NONE', *, *, #31750, .F. ) ;
#6494 = PLANE ( 'NONE',  #45542 ) ;
#6495 = EDGE_LOOP ( 'NONE', ( #2350, #3330, #22851, #20538 ) ) ;
#6496 = CARTESIAN_POINT ( 'NONE',  ( -17.82366898634780128, -4.565544526780660028, 11.09808643466108613 ) ) ;
#6497 = DIRECTION ( 'NONE',  ( 0.6427681459581294776, -0.7660444431189769032, 0.005002170337467562802 ) ) ;
#6498 = CARTESIAN_POINT ( 'NONE',  ( -14.94916102560700821, 0.000000000000000000, 2.688082935172642962 ) ) ;
#6499 = DIRECTION ( 'NONE',  ( -0.005961354470445682716, -0.6427876096865404731, 0.7660212471507180654 ) ) ;
#6500 = DIRECTION ( 'NONE',  ( 0.5449076811759707706, 0.6444004775717708799, -0.5364919789714476250 ) ) ;
#6501 = CARTESIAN_POINT ( 'NONE',  ( -13.65970254623731783, 0.000000000000000000, 2.328785729410555394 ) ) ;
#6502 = CARTESIAN_POINT ( 'NONE',  ( -1.148821818165424169, 4.447699752827971587, 3.664614983992416697 ) ) ;
#6503 = VECTOR ( 'NONE', #18411, 1000.000000000000227 ) ;
#6504 = CARTESIAN_POINT ( 'NONE',  ( -16.06709938707323460, 0.000000000000000000, 13.13181314741652628 ) ) ;
#6505 = CARTESIAN_POINT ( 'NONE',  ( -11.38054826722768098, 24.93301270189227381, 3.000000000000000000 ) ) ;
#6506 = LINE ( 'NONE', #19574, #3968 ) ;
#6507 = DIRECTION ( 'NONE',  ( -0.005002170337468016433, -0.7660444431189770143, 0.6427681459581293666 ) ) ;
#6508 = PLANE ( 'NONE',  #20022 ) ;
#6509 = PLANE ( 'NONE',  #6015 ) ;
#6510 = LINE ( 'NONE', #41447, #3712 ) ;
#6511 = LINE ( 'NONE', #28940, #24848 ) ;
#6512 = ADVANCED_FACE ( 'NONE', ( #6833 ), #33245, .F. ) ;
#6513 = CARTESIAN_POINT ( 'NONE',  ( -27.99845268667336384, -0.1191753592594197858, 7.657176279295684118 ) ) ;
#6514 = CARTESIAN_POINT ( 'NONE',  ( -14.63655816273770149, 0.6102101463440035012, 2.347799083036467671 ) ) ;
#6515 = ORIENTED_EDGE ( 'NONE', *, *, #21979, .F. ) ;
#6516 = CARTESIAN_POINT ( 'NONE',  ( -27.99767448711536133, 0.000000000000000000, 7.557179307314289218 ) ) ;
#6517 = ORIENTED_EDGE ( 'NONE', *, *, #36388, .F. ) ;
#6518 = ADVANCED_FACE ( 'NONE', ( #2278 ), #45181, .F. ) ;
#6519 = PLANE ( 'NONE',  #41375 ) ;
#6520 = DIRECTION ( 'NONE',  ( 0.007781995580012663651, 0.000000000000000000, -0.9999697198139515519 ) ) ;
#6521 = VECTOR ( 'NONE', #29133, 1000.000000000000227 ) ;
#6522 = VECTOR ( 'NONE', #12298, 1000.000000000000114 ) ;
#6523 = ORIENTED_EDGE ( 'NONE', *, *, #44643, .T. ) ;
#6524 = LINE ( 'NONE', #15327, #34016 ) ;
#6525 = ADVANCED_FACE ( 'NONE', ( #24687 ), #55097, .F. ) ;
#6526 = ORIENTED_EDGE ( 'NONE', *, *, #33647, .F. ) ;
#6527 = CARTESIAN_POINT ( 'NONE',  ( -18.69867377500269257, -0.1191753592594165800, 5.882888960116697596 ) ) ;
#6528 = VERTEX_POINT ( 'NONE', #32413 ) ;
#6529 = ORIENTED_EDGE ( 'NONE', *, *, #11707, .F. ) ;
#6530 = VECTOR ( 'NONE', #35617, 1000.000000000000227 ) ;
#6531 = ORIENTED_EDGE ( 'NONE', *, *, #49562, .F. ) ;
#6532 = DIRECTION ( 'NONE',  ( -0.7660212471507179544, -0.6427876096865405842, -0.005961354470445141482 ) ) ;
#6533 = FACE_OUTER_BOUND ( 'NONE', #45933, .T. ) ;
#6534 = LINE ( 'NONE', #37774, #36682 ) ;
#6535 = ORIENTED_EDGE ( 'NONE', *, *, #19165, .T. ) ;
#6536 = AXIS2_PLACEMENT_3D ( 'NONE', #26903, #484, #8748 ) ;
#6537 = VERTEX_POINT ( 'NONE', #54793 ) ;
#6538 = AXIS2_PLACEMENT_3D ( 'NONE', #27355, #2059, #31359 ) ;
#6539 = CARTESIAN_POINT ( 'NONE',  ( -9.432946420178224045, 1.988741823534331044, 2.708862623243400769 ) ) ;
#6540 = ORIENTED_EDGE ( 'NONE', *, *, #42144, .T. ) ;
#6541 = LINE ( 'NONE', #28392, #53635 ) ;
#6542 = ADVANCED_FACE ( 'NONE', ( #10555 ), #54247, .F. ) ;
#6543 = ORIENTED_EDGE ( 'NONE', *, *, #26124, .F. ) ;
#6544 = CARTESIAN_POINT ( 'NONE',  ( -14.00280974873554030, 0.000000000000000000, 12.40921378708904044 ) ) ;
#6545 = LINE ( 'NONE', #23858, #32170 ) ;
#6547 = EDGE_LOOP ( 'NONE', ( #29927, #36817, #30180, #43493 ) ) ;
#6546 = EDGE_CURVE ( 'NONE', #1661, #22227, #40898, .T. ) ;
#6548 = LINE ( 'NONE', #23862, #1038 ) ;
#6549 = EDGE_CURVE ( 'NONE', #47842, #52488, #3110, .T. ) ;
#6550 = FACE_OUTER_BOUND ( 'NONE', #48558, .T. ) ;
#6551 = VERTEX_POINT ( 'NONE', #50553 ) ;
#6552 = DIRECTION ( 'NONE',  ( -0.9999697198139514409, -0.000000000000000000, -0.007781995580013368816 ) ) ;
#6553 = LINE ( 'NONE', #24171, #2172 ) ;
#6554 = VECTOR ( 'NONE', #49098, 1000.000000000000000 ) ;
#6555 = CARTESIAN_POINT ( 'NONE',  ( -12.75761288849197328, 0.000000000000000000, 5.829120641561431171 ) ) ;
#6556 = VERTEX_POINT ( 'NONE', #27873 ) ;
#6557 = VECTOR ( 'NONE', #48069, 1000.000000000000227 ) ;
#6558 = VECTOR ( 'NONE', #30927, 999.9999999999998863 ) ;
#6559 = DIRECTION ( 'NONE',  ( -0.5449076811759708816, 0.6444004775717707689, 0.5364919789714475140 ) ) ;
#6560 = PLANE ( 'NONE',  #7901 ) ;
#6561 = DIRECTION ( 'NONE',  ( 0.7660212471507180654, -0.6427876096865404731, 0.005961354470445141482 ) ) ;
#6562 = FACE_OUTER_BOUND ( 'NONE', #10972, .T. ) ;
#6563 = CARTESIAN_POINT ( 'NONE',  ( -9.761175402966818737, 0.000000000000000000, 4.744443401512198122 ) ) ;
#6564 = FACE_OUTER_BOUND ( 'NONE', #15870, .T. ) ;
#6565 = ADVANCED_FACE ( 'NONE', ( #37782 ), #23581, .F. ) ;
#6566 = VECTOR ( 'NONE', #36285, 1000.000000000000227 ) ;
#6567 = CARTESIAN_POINT ( 'NONE',  ( -66.91943787661757881, -11.38163932023507385, -3.410887992466311136 ) ) ;
#6568 = VECTOR ( 'NONE', #51945, 1000.000000000000114 ) ;
#6569 = EDGE_LOOP ( 'NONE', ( #36596, #12206, #15666, #14016 ) ) ;
#6570 = DIRECTION ( 'NONE',  ( -0.9321478471874540261, 0.000000000000000000, 0.3620778797217457656 ) ) ;
#6571 = DIRECTION ( 'NONE',  ( -0.5449076811759708816, 0.6444004775717707689, 0.5364919789714475140 ) ) ;
#6572 = CARTESIAN_POINT ( 'NONE',  ( -67.03651911971512334, -0.6010133214110180422, -0.6815216469086778917 ) ) ;
#6573 = ORIENTED_EDGE ( 'NONE', *, *, #17979, .F. ) ;
#6574 = CARTESIAN_POINT ( 'NONE',  ( -17.93139508144814442, 0.000000000000000000, 13.85596890686001537 ) ) ;
#6575 = PLANE ( 'NONE',  #49023 ) ;
#6576 = FACE_OUTER_BOUND ( 'NONE', #16856, .T. ) ;
#6577 = VECTOR ( 'NONE', #53241, 999.9999999999998863 ) ;
#6578 = DIRECTION ( 'NONE',  ( -0.005961354470445682716, -0.6427876096865404731, 0.7660212471507180654 ) ) ;
#6579 = CARTESIAN_POINT ( 'NONE',  ( -55.97617513261492661, 6.813462753686547302, 1.872163189751866907 ) ) ;
#6580 = ORIENTED_EDGE ( 'NONE', *, *, #52151, .T. ) ;
#6581 = VERTEX_POINT ( 'NONE', #19313 ) ;
#6582 = CARTESIAN_POINT ( 'NONE',  ( -11.21979143729922157, -0.1191753592594201050, 1.139774444304266554 ) ) ;
#6583 = FACE_OUTER_BOUND ( 'NONE', #812, .T. ) ;
#6584 = ORIENTED_EDGE ( 'NONE', *, *, #32256, .T. ) ;
#6585 = CARTESIAN_POINT ( 'NONE',  ( -15.68268933366439732, -4.241740624735661491, 9.735039861682876605 ) ) ;
#6586 = ADVANCED_FACE ( 'NONE', ( #28697 ), #53965, .F. ) ;
#6587 = VECTOR ( 'NONE', #48975, 1000.000000000000000 ) ;
#6588 = ORIENTED_EDGE ( 'NONE', *, *, #9361, .T. ) ;
#6589 = CARTESIAN_POINT ( 'NONE',  ( -19.42910703681909368, 21.15220053346460816, 4.255330291687501543 ) ) ;
#6590 = ORIENTED_EDGE ( 'NONE', *, *, #12205, .T. ) ;
#6591 = ORIENTED_EDGE ( 'NONE', *, *, #2266, .T. ) ;
#6592 = LINE ( 'NONE', #41239, #1203 ) ;
#6593 = AXIS2_PLACEMENT_3D ( 'NONE', #28236, #18906, #11496 ) ;
#6594 = FACE_OUTER_BOUND ( 'NONE', #17017, .T. ) ;
#6595 = DIRECTION ( 'NONE',  ( -0.005961354470445682716, -0.6427876096865404731, 0.7660212471507180654 ) ) ;
#6596 = EDGE_CURVE ( 'NONE', #15779, #15522, #32938, .T. ) ;
#6597 = ORIENTED_EDGE ( 'NONE', *, *, #7382, .T. ) ;
#6598 = VECTOR ( 'NONE', #46178, 1000.000000000000000 ) ;
#6599 = VECTOR ( 'NONE', #51274, 999.9999999999998863 ) ;
#6600 = CARTESIAN_POINT ( 'NONE',  ( -23.33849165029409889, 0.000000000000000000, 5.946783852668351855 ) ) ;
#6601 = EDGE_LOOP ( 'NONE', ( #3523, #5146, #20964, #15091 ) ) ;
#6602 = EDGE_CURVE ( 'NONE', #17094, #43539, #7369, .T. ) ;
#6603 = EDGE_CURVE ( 'NONE', #25448, #35388, #10813, .T. ) ;
#6604 = VERTEX_POINT ( 'NONE', #45427 ) ;
#6605 = VECTOR ( 'NONE', #29367, 999.9999999999998863 ) ;
#6606 = EDGE_LOOP ( 'NONE', ( #41022, #15281, #4651, #28201 ) ) ;
#6607 = DIRECTION ( 'NONE',  ( 0.000000000000000000, -1.000000000000000000, 0.000000000000000000 ) ) ;
#6608 = AXIS2_PLACEMENT_3D ( 'NONE', #45665, #49380, #24637 ) ;
#6609 = ORIENTED_EDGE ( 'NONE', *, *, #43186, .T. ) ;
#6610 = LINE ( 'NONE', #33312, #44770 ) ;
#6611 = EDGE_CURVE ( 'NONE', #22139, #32655, #6541, .T. ) ;
#6612 = ORIENTED_EDGE ( 'NONE', *, *, #41658, .F. ) ;
#6613 = DIRECTION ( 'NONE',  ( 0.007781995580012663651, 0.000000000000000000, -0.9999697198139515519 ) ) ;
#6614 = CARTESIAN_POINT ( 'NONE',  ( 4.994031378522667985, 0.000000000000000000, 2.289010529401726668 ) ) ;
#6615 = VERTEX_POINT ( 'NONE', #41477 ) ;
#6616 = EDGE_CURVE ( 'NONE', #48632, #16890, #21583, .T. ) ;
#6618 = AXIS2_PLACEMENT_3D ( 'NONE', #16687, #34561, #21223 ) ;
#6617 = CARTESIAN_POINT ( 'NONE',  ( -19.62989625882111255, -4.565544526780664469, 4.360574684536503653 ) ) ;
#6619 = ORIENTED_EDGE ( 'NONE', *, *, #37522, .T. ) ;
#6620 = VECTOR ( 'NONE', #27274, 1000.000000000000227 ) ;
#6621 = EDGE_CURVE ( 'NONE', #8639, #21470, #42853, .T. ) ;
#6622 = CARTESIAN_POINT ( 'NONE',  ( 2.072287782118878319, 0.000000000000000000, -2.950529333540147015 ) ) ;
#6623 = CARTESIAN_POINT ( 'NONE',  ( -12.03474988952295455, -0.5179957512181563306, 2.206756566172713097 ) ) ;
#6624 = FACE_OUTER_BOUND ( 'NONE', #25253, .T. ) ;
#6625 = CARTESIAN_POINT ( 'NONE',  ( -13.46833076279037833, 0.000000000000000000, 3.438271238299851706 ) ) ;
#6626 = CARTESIAN_POINT ( 'NONE',  ( -13.13165317342551397, -0.1191753592594194527, 7.034209011106107745 ) ) ;
#6627 = EDGE_LOOP ( 'NONE', ( #43377, #33752, #55801, #27306 ) ) ;
#6628 = VECTOR ( 'NONE', #4042, 999.9999999999998863 ) ;
#6629 = ADVANCED_FACE ( 'NONE', ( #47117 ), #29231, .F. ) ;
#6630 = EDGE_LOOP ( 'NONE', ( #35466, #54308, #7503, #30337 ) ) ;
#6631 = CARTESIAN_POINT ( 'NONE',  ( -13.08486533123210194, 0.000000000000000000, 1.963927175729152541 ) ) ;
#6632 = LINE ( 'NONE', #19404, #31189 ) ;
#6633 = VECTOR ( 'NONE', #52347, 999.9999999999998863 ) ;
#6634 = CARTESIAN_POINT ( 'NONE',  ( -10.47421230394850866, 0.000000000000000000, 10.95934586908605723 ) ) ;
#6635 = DIRECTION ( 'NONE',  ( 0.6427681459581294776, -0.7660444431189769032, 0.005002170337467562802 ) ) ;
#6636 = EDGE_CURVE ( 'NONE', #28378, #35444, #12200, .T. ) ;
#6637 = DIRECTION ( 'NONE',  ( -0.7660212471507179544, -0.6427876096865405842, -0.005961354470445141482 ) ) ;
#6638 = EDGE_LOOP ( 'NONE', ( #51500, #25516, #42248, #37505 ) ) ;
#6639 = PLANE ( 'NONE',  #21373 ) ;
#6640 = CARTESIAN_POINT ( 'NONE',  ( 2.072287782118878319, 0.000000000000000000, -2.950529333540147015 ) ) ;
#6641 = ORIENTED_EDGE ( 'NONE', *, *, #30338, .F. ) ;
#6643 = DIRECTION ( 'NONE',  ( -0.5364919789714478471, 0.6444004775717705469, -0.5449076811759709926 ) ) ;
#6642 = VECTOR ( 'NONE', #42365, 1000.000000000000227 ) ;
#6644 = CARTESIAN_POINT ( 'NONE',  ( -24.26908309836554878, 0.000000000000000000, 6.108867788427308376 ) ) ;
#6645 = ORIENTED_EDGE ( 'NONE', *, *, #21216, .T. ) ;
#6646 = AXIS2_PLACEMENT_3D ( 'NONE', #1577, #53522, #6232 ) ;
#6647 = VECTOR ( 'NONE', #24252, 999.9999999999998863 ) ;
#6648 = CARTESIAN_POINT ( 'NONE',  ( -67.56320601492518563, -0.9999999999999974465, -2.442027903730110250 ) ) ;
#6649 = LINE ( 'NONE', #24258, #12452 ) ;
#6650 = LINE ( 'NONE', #1564, #39533 ) ;
#6651 = LINE ( 'NONE', #35948, #27789 ) ;
#6652 = FACE_OUTER_BOUND ( 'NONE', #24701, .T. ) ;
#6653 = EDGE_LOOP ( 'NONE', ( #18670, #3870, #21672, #36433 ) ) ;
#6654 = AXIS2_PLACEMENT_3D ( 'NONE', #296, #26425, #14 ) ;
#6655 = VECTOR ( 'NONE', #23066, 1000.000000000000000 ) ;
#6656 = ORIENTED_EDGE ( 'NONE', *, *, #9049, .T. ) ;
#6657 = LINE ( 'NONE', #46111, #54752 ) ;
#6658 = DIRECTION ( 'NONE',  ( 0.6427681459581294776, -0.7660444431189769032, 0.005002170337467562802 ) ) ;
#6659 = FACE_OUTER_BOUND ( 'NONE', #5241, .T. ) ;
#6660 = CARTESIAN_POINT ( 'NONE',  ( -12.80458192191714595, 0.000000000000000000, 11.86454056839041726 ) ) ;
#6661 = DIRECTION ( 'NONE',  ( 0.5364919789714477361, 0.6444004775717706579, 0.5449076811759711036 ) ) ;
#6662 = LINE ( 'NONE', #23976, #5898 ) ;
#6663 = EDGE_CURVE ( 'NONE', #56078, #48949, #29819, .T. ) ;
#6664 = ORIENTED_EDGE ( 'NONE', *, *, #31749, .F. ) ;
#6666 = VECTOR ( 'NONE', #10939, 1000.000000000000227 ) ;
#6665 = DIRECTION ( 'NONE',  ( 0.007781995580012663651, -3.146120232559066537E-19, -0.9999697198139514409 ) ) ;
#6667 = DIRECTION ( 'NONE',  ( 0.9999697198139515519, 0.000000000000000000, 0.007781995580013368816 ) ) ;
#6668 = DIRECTION ( 'NONE',  ( 0.007781995580012663651, -3.146120232559066537E-19, -0.9999697198139514409 ) ) ;
#6669 = ORIENTED_EDGE ( 'NONE', *, *, #54780, .T. ) ;
#6670 = CARTESIAN_POINT ( 'NONE',  ( -69.43545830293986398, -9.790829293527439248, 7.501778215771295777 ) ) ;
#6671 = DIRECTION ( 'NONE',  ( 0.9321478471874540261, 0.000000000000000000, -0.3620778797217456546 ) ) ;
#6672 = VECTOR ( 'NONE', #18942, 1000.000000000000227 ) ;
#6673 = ADVANCED_FACE ( 'NONE', ( #16445 ), #42579, .F. ) ;
#6674 = CARTESIAN_POINT ( 'NONE',  ( 2.072287782118878319, 0.000000000000000000, -2.950529333540147015 ) ) ;
#6675 = ORIENTED_EDGE ( 'NONE', *, *, #52380, .T. ) ;
#6676 = FACE_OUTER_BOUND ( 'NONE', #53165, .T. ) ;
#6677 = AXIS2_PLACEMENT_3D ( 'NONE', #15383, #42360, #28437 ) ;
#6678 = VERTEX_POINT ( 'NONE', #3411 ) ;
#6679 = EDGE_CURVE ( 'NONE', #8091, #24779, #8221, .T. ) ;
#6680 = ORIENTED_EDGE ( 'NONE', *, *, #25450, .T. ) ;
#6681 = ORIENTED_EDGE ( 'NONE', *, *, #18532, .F. ) ;
#6682 = ORIENTED_EDGE ( 'NONE', *, *, #12768, .T. ) ;
#6683 = EDGE_LOOP ( 'NONE', ( #33292, #29988, #10668, #9770 ) ) ;
#6684 = VECTOR ( 'NONE', #12350, 1000.000000000000227 ) ;
#6685 = CARTESIAN_POINT ( 'NONE',  ( -61.74810725808002587, 6.470640170577546257, -3.000000000000007105 ) ) ;
#6686 = ORIENTED_EDGE ( 'NONE', *, *, #10964, .F. ) ;
#6687 = PRESENTATION_LAYER_ASSIGNMENT (  '', '', ( #19357 ) ) ;
#6688 = VECTOR ( 'NONE', #28348, 1000.000000000000227 ) ;
#6689 = ORIENTED_EDGE ( 'NONE', *, *, #33111, .T. ) ;
#6690 = CARTESIAN_POINT ( 'NONE',  ( -11.27597963956645089, -0.1191753592594181482, 7.417982361435909056 ) ) ;
#6691 = EDGE_CURVE ( 'NONE', #22414, #5753, #20988, .T. ) ;
#6692 = ORIENTED_EDGE ( 'NONE', *, *, #8618, .F. ) ;
#6693 = ORIENTED_EDGE ( 'NONE', *, *, #6980, .F. ) ;
#6694 = ADVANCED_FACE ( 'NONE', ( #3671 ), #4267, .F. ) ;
#6695 = ORIENTED_EDGE ( 'NONE', *, *, #47633, .T. ) ;
#6696 = VECTOR ( 'NONE', #49690, 1000.000000000000227 ) ;
#6697 = VECTOR ( 'NONE', #19845, 1000.000000000000000 ) ;
#6698 = DIRECTION ( 'NONE',  ( -0.6427681459581293666, -0.7660444431189770143, -0.005002170337467561935 ) ) ;
#6699 = CARTESIAN_POINT ( 'NONE',  ( -18.12619594522237065, 0.000000000000000000, 4.879350933650815847 ) ) ;
#6700 = CARTESIAN_POINT ( 'NONE',  ( -17.93139508144814442, 0.000000000000000000, 13.85596890686001537 ) ) ;
#6701 = DIRECTION ( 'NONE',  ( -0.9999697198139514409, -0.000000000000000000, -0.007781995580013368816 ) ) ;
#6702 = ORIENTED_EDGE ( 'NONE', *, *, #48843, .T. ) ;
#6703 = DIRECTION ( 'NONE',  ( 0.9999697198139515519, 0.000000000000000000, 0.007781995580013368816 ) ) ;
#6704 = ORIENTED_EDGE ( 'NONE', *, *, #45451, .T. ) ;
#6705 = EDGE_CURVE ( 'NONE', #46401, #2028, #25273, .T. ) ;
#6706 = VERTEX_POINT ( 'NONE', #8810 ) ;
#6707 = PLANE ( 'NONE',  #11246 ) ;
#6708 = CARTESIAN_POINT ( 'NONE',  ( 2.072287782118878319, 0.000000000000000000, -2.950529333540147015 ) ) ;
#6709 = CARTESIAN_POINT ( 'NONE',  ( -30.79411802867772607, 0.000000000000000000, 8.643412946479525516 ) ) ;
#6710 = AXIS2_PLACEMENT_3D ( 'NONE', #2048, #11710, #16243 ) ;
#6711 = DIRECTION ( 'NONE',  ( 0.007781995580012663651, 0.000000000000000000, -0.9999697198139515519 ) ) ;
#6712 = DIRECTION ( 'NONE',  ( 0.9999697198139515519, 0.000000000000000000, 0.007781995580013368816 ) ) ;
#6713 = ORIENTED_EDGE ( 'NONE', *, *, #14409, .T. ) ;
#6714 = DIRECTION ( 'NONE',  ( -0.5449076811759708816, 0.6444004775717707689, 0.5364919789714475140 ) ) ;
#6715 = VECTOR ( 'NONE', #6363, 1000.000000000000227 ) ;
#6716 = ORIENTED_EDGE ( 'NONE', *, *, #41092, .T. ) ;
#6717 = DIRECTION ( 'NONE',  ( -0.6427681459581293666, -0.7660444431189770143, -0.005002170337467561935 ) ) ;
#6718 = DIRECTION ( 'NONE',  ( 0.007781995580012662783, 0.000000000000000000, -0.9999697198139514409 ) ) ;
#6719 = DIRECTION ( 'NONE',  ( 0.9999697198139515519, 0.000000000000000000, 0.007781995580013368816 ) ) ;
#6720 = VECTOR ( 'NONE', #10426, 1000.000000000000000 ) ;
#6721 = LINE ( 'NONE', #1880, #19529 ) ;
#6722 = DIRECTION ( 'NONE',  ( 0.007781995580012662783, 0.000000000000000000, -0.9999697198139514409 ) ) ;
#6723 = ORIENTED_EDGE ( 'NONE', *, *, #19766, .F. ) ;
#6724 = VECTOR ( 'NONE', #611, 1000.000000000000114 ) ;
#6725 = LINE ( 'NONE', #32308, #52001 ) ;
#6726 = CARTESIAN_POINT ( 'NONE',  ( -16.99924723426068951, 0.000000000000000000, 13.49389102713827171 ) ) ;
#6727 = DIRECTION ( 'NONE',  ( -0.005961354470445682716, -0.6427876096865404731, 0.7660212471507180654 ) ) ;
#6728 = ADVANCED_FACE ( 'NONE', ( #33772 ), #33506, .F. ) ;
#6729 = VECTOR ( 'NONE', #2291, 999.9999999999998863 ) ;
#6730 = LINE ( 'NONE', #24052, #39146 ) ;
#6731 = DIRECTION ( 'NONE',  ( -0.000000000000000000, -1.000000000000000000, 0.000000000000000000 ) ) ;
#6732 = EDGE_CURVE ( 'NONE', #6615, #10587, #21831, .T. ) ;
#6733 = CARTESIAN_POINT ( 'NONE',  ( 2.072287782118878319, 0.000000000000000000, -2.950529333540147015 ) ) ;
#6734 = CARTESIAN_POINT ( 'NONE',  ( -19.60912206198628027, -0.1191753592594197858, 4.398475361799976113 ) ) ;
#6735 = VECTOR ( 'NONE', #44794, 1000.000000000000114 ) ;
#6736 = VECTOR ( 'NONE', #38207, 1000.000000000000114 ) ;
#6737 = DIRECTION ( 'NONE',  ( 0.9999697198139515519, 0.000000000000000000, 0.007781995580013368816 ) ) ;
#6738 = EDGE_CURVE ( 'NONE', #32684, #37529, #34353, .T. ) ;
#6739 = DIRECTION ( 'NONE',  ( 0.5364919789714477361, 0.6444004775717706579, 0.5449076811759711036 ) ) ;
#6740 = EDGE_CURVE ( 'NONE', #20350, #33580, #34079, .T. ) ;
#6741 = ADVANCED_FACE ( 'NONE', ( #12501 ), #56200, .F. ) ;
#6742 = EDGE_CURVE ( 'NONE', #29012, #5769, #34609, .T. ) ;
#6743 = EDGE_LOOP ( 'NONE', ( #32775, #41751, #48940, #49886 ) ) ;
#6744 = AXIS2_PLACEMENT_3D ( 'NONE', #33247, #50555, #16186 ) ;
#6745 = ORIENTED_EDGE ( 'NONE', *, *, #39992, .F. ) ;
#6746 = ORIENTED_EDGE ( 'NONE', *, *, #704, .T. ) ;
#6747 = ORIENTED_EDGE ( 'NONE', *, *, #31131, .F. ) ;
#6748 = ORIENTED_EDGE ( 'NONE', *, *, #44899, .T. ) ;
#6749 = DIRECTION ( 'NONE',  ( 0.005961354470445682716, -0.6427876096865404731, -0.7660212471507180654 ) ) ;
#6750 = CARTESIAN_POINT ( 'NONE',  ( -11.40636015113596180, 0.000000000000000000, 11.32142374880780089 ) ) ;
#6751 = VECTOR ( 'NONE', #41, 1000.000000000000227 ) ;
#6752 = ORIENTED_EDGE ( 'NONE', *, *, #13911, .T. ) ;
#6753 = PLANE ( 'NONE',  #44890 ) ;
#6754 = EDGE_CURVE ( 'NONE', #6764, #51258, #30376, .T. ) ;
#6755 = ORIENTED_EDGE ( 'NONE', *, *, #19158, .T. ) ;
#6756 = ORIENTED_EDGE ( 'NONE', *, *, #18186, .T. ) ;
#6757 = ADVANCED_FACE ( 'NONE', ( #24991 ), #22677, .F. ) ;
#6758 = VECTOR ( 'NONE', #17758, 1000.000000000000227 ) ;
#6759 = CARTESIAN_POINT ( 'NONE',  ( -65.07086784306864047, -9.156548800121029785, 0.3806443636437001898 ) ) ;
#6760 = ADVANCED_FACE ( 'NONE', ( #4797 ), #1076, .F. ) ;
#6761 = VECTOR ( 'NONE', #34069, 1000.000000000000227 ) ;
#6762 = DIRECTION ( 'NONE',  ( 0.000000000000000000, -1.000000000000000000, 0.000000000000000000 ) ) ;
#6763 = CARTESIAN_POINT ( 'NONE',  ( -19.60990026154428278, 0.000000000000000000, 4.498472333781370125 ) ) ;
#6764 = VERTEX_POINT ( 'NONE', #22427 ) ;
#6765 = CARTESIAN_POINT ( 'NONE',  ( -13.23817645197547144, 0.000000000000000000, 7.872047190045031506 ) ) ;
#6766 = VECTOR ( 'NONE', #25625, 1000.000000000000000 ) ;
#6767 = ADVANCED_FACE ( 'NONE', ( #40582 ), #549, .F. ) ;
#6768 = LINE ( 'NONE', #11592, #37277 ) ;
#6769 = LINE ( 'NONE', #55293, #37509 ) ;
#6770 = EDGE_CURVE ( 'NONE', #8639, #13033, #36051, .T. ) ;
#6771 = AXIS2_PLACEMENT_3D ( 'NONE', #23374, #27624, #40690 ) ;
#6772 = DIRECTION ( 'NONE',  ( 0.000000000000000000, 1.000000000000000000, 0.000000000000000000 ) ) ;
#6773 = DIRECTION ( 'NONE',  ( -0.6246952433987893460, -0.7422098413412802076, 0.2426528472758542054 ) ) ;
#6774 = VECTOR ( 'NONE', #54476, 1000.000000000000227 ) ;
#6775 = CARTESIAN_POINT ( 'NONE',  ( -10.20150221737636542, 0.000000000000000000, 1.617034104387096383 ) ) ;
#6776 = DIRECTION ( 'NONE',  ( 0.007781995580012663651, -3.146120232559066537E-19, -0.9999697198139514409 ) ) ;
#6777 = DIRECTION ( 'NONE',  ( -0.7660212471507179544, -0.6427876096865405842, -0.005961354470445141482 ) ) ;
#6778 = LINE ( 'NONE', #41676, #53774 ) ;
#6779 = VERTEX_POINT ( 'NONE', #44522 ) ;
#6780 = DIRECTION ( 'NONE',  ( 0.007781995580012662783, 0.000000000000000000, -0.9999697198139514409 ) ) ;
#6781 = EDGE_LOOP ( 'NONE', ( #28456, #45534, #33698, #44036 ) ) ;
#6782 = CARTESIAN_POINT ( 'NONE',  ( -26.13493519185646008, 0.000000000000000000, 7.033017491833586377 ) ) ;
#6783 = CARTESIAN_POINT ( 'NONE',  ( -14.07363356994439840, -1.813211359398156919, 5.124397700033340719 ) ) ;
#6784 = DIRECTION ( 'NONE',  ( 0.9999697198139515519, 0.000000000000000000, 0.007781995580013368816 ) ) ;
#6785 = DIRECTION ( 'NONE',  ( -0.005002170337468016433, -0.7660444431189770143, 0.6427681459581293666 ) ) ;
#6786 = LINE ( 'NONE', #54747, #10468 ) ;
#6787 = VECTOR ( 'NONE', #30052, 1000.000000000000227 ) ;
#6788 = DIRECTION ( 'NONE',  ( -0.5449076811759708816, 0.6444004775717707689, 0.5364919789714475140 ) ) ;
#6789 = AXIS2_PLACEMENT_3D ( 'NONE', #25602, #29310, #17103 ) ;
#6790 = FACE_OUTER_BOUND ( 'NONE', #45076, .T. ) ;
#6791 = LINE ( 'NONE', #7333, #55648 ) ;
#6792 = DIRECTION ( 'NONE',  ( -0.005002170337468016433, -0.7660444431189770143, 0.6427681459581293666 ) ) ;
#6793 = DIRECTION ( 'NONE',  ( -0.9999697198139514409, -0.000000000000000000, -0.007781995580013368816 ) ) ;
#6794 = VECTOR ( 'NONE', #9514, 1000.000000000000227 ) ;
#6795 = CARTESIAN_POINT ( 'NONE',  ( -13.07066190154808361, 0.000000000000000000, 12.04713590736729678 ) ) ;
#6796 = PLANE ( 'NONE',  #6481 ) ;
#6797 = AXIS2_PLACEMENT_3D ( 'NONE', #20456, #17047, #38625 ) ;
#6798 = CARTESIAN_POINT ( 'NONE',  ( -21.47263955680318404, 0.000000000000000000, 5.022634149262071190 ) ) ;
#6799 = DIRECTION ( 'NONE',  ( -0.005002170337468016433, -0.7660444431189770143, 0.6427681459581293666 ) ) ;
#6800 = DIRECTION ( 'NONE',  ( -0.8531650599175527594, 0.4028455766673922356, 0.3313982828793700652 ) ) ;
#6801 = ORIENTED_EDGE ( 'NONE', *, *, #30139, .F. ) ;
#6802 = DIRECTION ( 'NONE',  ( 0.007781995580012663651, 0.000000000000000000, -0.9999697198139515519 ) ) ;
#6803 = AXIS2_PLACEMENT_3D ( 'NONE', #16999, #41958, #29187 ) ;
#6804 = VECTOR ( 'NONE', #41499, 999.9999999999998863 ) ;
#6805 = ORIENTED_EDGE ( 'NONE', *, *, #12410, .F. ) ;
#6806 = VECTOR ( 'NONE', #5139, 1000.000000000000114 ) ;
#6807 = CARTESIAN_POINT ( 'NONE',  ( -33.59056157024009082, 0.000000000000000000, 9.729646585644761814 ) ) ;
#6808 = VECTOR ( 'NONE', #38524, 1000.000000000000227 ) ;
#6809 = LINE ( 'NONE', #24134, #33056 ) ;
#6810 = VECTOR ( 'NONE', #28722, 1000.000000000000227 ) ;
#6811 = EDGE_CURVE ( 'NONE', #17974, #19153, #35750, .T. ) ;
#6812 = ADVANCED_FACE ( 'NONE', ( #13870 ), #31767, .F. ) ;
#6813 = EDGE_LOOP ( 'NONE', ( #53295, #4976, #44860, #33084 ) ) ;
#6814 = ORIENTED_EDGE ( 'NONE', *, *, #9853, .F. ) ;
#6815 = FACE_OUTER_BOUND ( 'NONE', #16623, .T. ) ;
#6816 = ADVANCED_FACE ( 'NONE', ( #5373 ), #39453, .T. ) ;
#6817 = AXIS2_PLACEMENT_3D ( 'NONE', #16793, #12546, #20187 ) ;
#6818 = ORIENTED_EDGE ( 'NONE', *, *, #5869, .T. ) ;
#6819 = AXIS2_PLACEMENT_3D ( 'NONE', #30806, #110, #8372 ) ;
#6820 = EDGE_LOOP ( 'NONE', ( #7515, #41652, #28955, #40442 ) ) ;
#6821 = EDGE_LOOP ( 'NONE', ( #25405, #10431, #53843, #2264 ) ) ;
#6822 = DIRECTION ( 'NONE',  ( 0.005961354470445682716, -0.6427876096865404731, -0.7660212471507180654 ) ) ;
#6823 = DIRECTION ( 'NONE',  ( 0.9999697198139515519, 0.000000000000000000, 0.007781995580013368816 ) ) ;
#6824 = CARTESIAN_POINT ( 'NONE',  ( -27.99923088623136636, 0.000000000000000000, 7.757173251277078130 ) ) ;
#6825 = VERTEX_POINT ( 'NONE', #39738 ) ;
#6826 = VERTEX_POINT ( 'NONE', #40282 ) ;
#6827 = EDGE_CURVE ( 'NONE', #51400, #40198, #14451, .T. ) ;
#6828 = VECTOR ( 'NONE', #15721, 999.9999999999998863 ) ;
#6829 = CARTESIAN_POINT ( 'NONE',  ( -58.00000000000000711, -8.999999999999998224, 2.750000000000013323 ) ) ;
#6830 = DIRECTION ( 'NONE',  ( 0.9999697198139515519, 0.000000000000000000, 0.007781995580013368816 ) ) ;
#6831 = CLOSED_SHELL ( 'NONE', ( #47988, #39827, #3719, #23415, #26829, #43131, #39539, #24833, #28152, #23876 ) ) ;
#6832 = ORIENTED_EDGE ( 'NONE', *, *, #727, .T. ) ;
#6833 = FACE_OUTER_BOUND ( 'NONE', #747, .T. ) ;
#6834 = ORIENTED_EDGE ( 'NONE', *, *, #44318, .F. ) ;
#6835 = VECTOR ( 'NONE', #8120, 1000.000000000000114 ) ;
#6836 = LINE ( 'NONE', #11068, #33944 ) ;
#6837 = LINE ( 'NONE', #7121, #22189 ) ;
#6838 = ORIENTED_EDGE ( 'NONE', *, *, #28804, .T. ) ;
#6839 = EDGE_CURVE ( 'NONE', #55994, #1128, #52763, .T. ) ;
#6840 = CARTESIAN_POINT ( 'NONE',  ( 0.1285714285714296967, 2.000000000000000000, 5.998622290806041590 ) ) ;
#6841 = VECTOR ( 'NONE', #33714, 1000.000000000000227 ) ;
#6842 = EDGE_CURVE ( 'NONE', #42246, #28007, #5937, .T. ) ;
#6843 = FACE_OUTER_BOUND ( 'NONE', #29165, .T. ) ;
#6844 = VECTOR ( 'NONE', #10819, 999.9999999999998863 ) ;
#6845 = VECTOR ( 'NONE', #29843, 1000.000000000000227 ) ;
#6847 = EDGE_CURVE ( 'NONE', #28953, #24378, #47963, .T. ) ;
#6846 = ORIENTED_EDGE ( 'NONE', *, *, #7978, .T. ) ;
#6848 = CARTESIAN_POINT ( 'NONE',  ( -22.40478740399063895, 0.000000000000000000, 5.384712028983816623 ) ) ;
#6849 = DIRECTION ( 'NONE',  ( 0.000000000000000000, -0.000000000000000000, -1.000000000000000000 ) ) ;
#6850 = DIRECTION ( 'NONE',  ( -0.7660212471507179544, -0.6427876096865405842, -0.005961354470445141482 ) ) ;
#6851 = EDGE_CURVE ( 'NONE', #37046, #34473, #35453, .T. ) ;
#6852 = ORIENTED_EDGE ( 'NONE', *, *, #21676, .T. ) ;
#6853 = VECTOR ( 'NONE', #25496, 1000.000000000000227 ) ;
#6854 = VECTOR ( 'NONE', #4526, 1000.000000000000227 ) ;
#6855 = CARTESIAN_POINT ( 'NONE',  ( 2.072287782118878319, 0.000000000000000000, -2.950529333540147015 ) ) ;
#6856 = DIRECTION ( 'NONE',  ( -0.6427681459581293666, -0.7660444431189770143, -0.005002170337467561935 ) ) ;
#6857 = ADVANCED_FACE ( 'NONE', ( #9915 ), #31196, .T. ) ;
#6858 = PLANE ( 'NONE',  #9515 ) ;
#6859 = CARTESIAN_POINT ( 'NONE',  ( -19.60834386242827776, 0.000000000000000000, 4.298478389818581213 ) ) ;
#6860 = DIRECTION ( 'NONE',  ( 0.005002170337468016433, -0.7660444431189770143, -0.6427681459581293666 ) ) ;
#6861 = CARTESIAN_POINT ( 'NONE',  ( -27.06630483948590893, -0.1191753592594197858, 7.295098399573937797 ) ) ;
#6862 = AXIS2_PLACEMENT_3D ( 'NONE', #18321, #30587, #23169 ) ;
#6863 = VECTOR ( 'NONE', #5456, 1000.000000000000227 ) ;
#6864 = CARTESIAN_POINT ( 'NONE',  ( -69.49918034145071033, -9.798606072444741244, -7.579899494734580578 ) ) ;
#6865 = ORIENTED_EDGE ( 'NONE', *, *, #51964, .F. ) ;
#6866 = CARTESIAN_POINT ( 'NONE',  ( -11.67244013076689946, 0.000000000000000000, 11.50401908778467863 ) ) ;
#6867 = CARTESIAN_POINT ( 'NONE',  ( -9.879165764022332041, -0.1191753592594198830, 7.055777056291618443 ) ) ;
#6868 = CARTESIAN_POINT ( 'NONE',  ( -66.91434672699239172, 8.085008987418439830E-12, -3.536654368688153305 ) ) ;
#6869 = ORIENTED_EDGE ( 'NONE', *, *, #33116, .T. ) ;
#6870 = CARTESIAN_POINT ( 'NONE',  ( -20.77435557342690231, 1.257817950434006793, 4.711265958276037225 ) ) ;
#6871 = DIRECTION ( 'NONE',  ( -0.5449076811759708816, 0.6444004775717707689, 0.5364919789714475140 ) ) ;
#6872 = PLANE ( 'NONE',  #47626 ) ;
#6873 = DIRECTION ( 'NONE',  ( 0.007781995580012663651, -3.146120232559066537E-19, -0.9999697198139514409 ) ) ;
#6874 = CARTESIAN_POINT ( 'NONE',  ( -10.42161453587613096, 0.000000000000000000, 4.200645628075444726 ) ) ;
#6875 = AXIS2_PLACEMENT_3D ( 'NONE', #10848, #23077, #23368 ) ;
#6876 = VERTEX_POINT ( 'NONE', #1375 ) ;
#6877 = ORIENTED_EDGE ( 'NONE', *, *, #23320, .F. ) ;
#6878 = VECTOR ( 'NONE', #31053, 1000.000000000000114 ) ;
#6879 = DIRECTION ( 'NONE',  ( 0.9999697198139515519, 0.000000000000000000, 0.007781995580013368816 ) ) ;
#6880 = VECTOR ( 'NONE', #23958, 1000.000000000000227 ) ;
#6881 = DIRECTION ( 'NONE',  ( 0.9999697198139515519, 0.000000000000000000, 0.007781995580013368816 ) ) ;
#6882 = EDGE_CURVE ( 'NONE', #53298, #43550, #52499, .T. ) ;
#6883 = EDGE_LOOP ( 'NONE', ( #46419, #26015, #45572, #20922 ) ) ;
#6884 = LINE ( 'NONE', #32698, #14030 ) ;
#6885 = VECTOR ( 'NONE', #43188, 999.9999999999998863 ) ;
#6886 = VERTEX_POINT ( 'NONE', #30910 ) ;
#6887 = CARTESIAN_POINT ( 'NONE',  ( -19.36810218178846910, 21.37987375194729367, 4.244941833917287077 ) ) ;
#6888 = ADVANCED_FACE ( 'NONE', ( #27218 ), #48220, .F. ) ;
#6889 = ADVANCED_FACE ( 'NONE', ( #36579 ), #54436, .F. ) ;
#6890 = VECTOR ( 'NONE', #50206, 1000.000000000000227 ) ;
#6891 = VECTOR ( 'NONE', #30238, 1000.000000000000000 ) ;
#6892 = ORIENTED_EDGE ( 'NONE', *, *, #52371, .F. ) ;
#6893 = ORIENTED_EDGE ( 'NONE', *, *, #25514, .T. ) ;
#6894 = LINE ( 'NONE', #20774, #33841 ) ;
#6895 = AXIS2_PLACEMENT_3D ( 'NONE', #6709, #5885, #37347 ) ;
#6896 = DIRECTION ( 'NONE',  ( -0.000000000000000000, -0.000000000000000000, 1.000000000000000000 ) ) ;
#6897 = PLANE ( 'NONE',  #42051 ) ;
#6898 = AXIS2_PLACEMENT_3D ( 'NONE', #3510, #43456, #4553 ) ;
#6899 = ORIENTED_EDGE ( 'NONE', *, *, #39907, .T. ) ;
#6900 = VECTOR ( 'NONE', #9011, 999.9999999999998863 ) ;
#6901 = CARTESIAN_POINT ( 'NONE',  ( -13.67539046815301162, 0.000000000000000000, 4.344650004994353942 ) ) ;
#6902 = VERTEX_POINT ( 'NONE', #11291 ) ;
#6903 = ADVANCED_FACE ( 'NONE', ( #10753 ), #15825, .F. ) ;
#6904 = AXIS2_PLACEMENT_3D ( 'NONE', #1768, #10310, #40697 ) ;
#6905 = ORIENTED_EDGE ( 'NONE', *, *, #49213, .F. ) ;
#6906 = AXIS2_PLACEMENT_3D ( 'NONE', #54154, #5897, #23751 ) ;
#6907 = VERTEX_POINT ( 'NONE', #36301 ) ;
#6908 = LINE ( 'NONE', #7175, #8695 ) ;
#6909 = ORIENTED_EDGE ( 'NONE', *, *, #9002, .F. ) ;
#6910 = LINE ( 'NONE', #49778, #26642 ) ;
#6911 = ORIENTED_EDGE ( 'NONE', *, *, #46153, .F. ) ;
#6912 = PLANE ( 'NONE',  #40365 ) ;
#6913 = CARTESIAN_POINT ( 'NONE',  ( -16.91648110301675345, 4.981562823951512620, 3.093929542590271087 ) ) ;
#6914 = EDGE_LOOP ( 'NONE', ( #7714, #18468, #39455, #27145 ) ) ;
#6915 = CARTESIAN_POINT ( 'NONE',  ( -11.67244013076689946, 0.000000000000000000, 11.50401908778467863 ) ) ;
#6916 = EDGE_LOOP ( 'NONE', ( #7862, #55693, #10027, #1048 ) ) ;
#6917 = EDGE_CURVE ( 'NONE', #46950, #1369, #50488, .T. ) ;
#6918 = VECTOR ( 'NONE', #5147, 1000.000000000000114 ) ;
#6919 = PLANE ( 'NONE',  #37335 ) ;
#6920 = CARTESIAN_POINT ( 'NONE',  ( -2.428019651919397948, -4.270454567941153634, -2.275248286963848177 ) ) ;
#6921 = DIRECTION ( 'NONE',  ( 0.5449076811759707706, 0.6444004775717708799, -0.5364919789714476250 ) ) ;
#6922 = CARTESIAN_POINT ( 'NONE',  ( -11.40636015113596180, 0.000000000000000000, 11.32142374880780089 ) ) ;
#6923 = DIRECTION ( 'NONE',  ( 0.6427681459581294776, -0.7660444431189769032, 0.005002170337467562802 ) ) ;
#6924 = CARTESIAN_POINT ( 'NONE',  ( 2.072287782118878319, 0.000000000000000000, -2.950529333540147015 ) ) ;
#6925 = AXIS2_PLACEMENT_3D ( 'NONE', #55444, #25101, #42956 ) ;
#6926 = ORIENTED_EDGE ( 'NONE', *, *, #37234, .F. ) ;
#6927 = ORIENTED_EDGE ( 'NONE', *, *, #36562, .T. ) ;
#6928 = CARTESIAN_POINT ( 'NONE',  ( -56.00000000000000711, 3.800000000000001599, 1.887458608817694561 ) ) ;
#6929 = VECTOR ( 'NONE', #16717, 999.9999999999998863 ) ;
#6930 = EDGE_CURVE ( 'NONE', #32088, #41657, #28324, .T. ) ;
#6931 = CARTESIAN_POINT ( 'NONE',  ( -17.74560456716937296, 0.000000000000000000, 3.774316574337878372 ) ) ;
#6932 = CARTESIAN_POINT ( 'NONE',  ( -21.06902270529800347, 1.581621852479006440, 7.660955954857441519 ) ) ;
#6933 = CARTESIAN_POINT ( 'NONE',  ( -17.65081820860546813, -5.536956232915666298, 3.560840440734917234 ) ) ;
#6934 = VECTOR ( 'NONE', #2459, 999.9999999999998863 ) ;
#6935 = CARTESIAN_POINT ( 'NONE',  ( -16.49350878336835891, 0.000000000000000000, 8.216045510926729634 ) ) ;
#6936 = ORIENTED_EDGE ( 'NONE', *, *, #22789, .T. ) ;
#6937 = DIRECTION ( 'NONE',  ( 0.2426528472758542054, 0.7422098413412800966, 0.6246952433987894571 ) ) ;
#6938 = DIRECTION ( 'NONE',  ( 0.6246952433987893460, 0.7422098413412802076, -0.2426528472758539279 ) ) ;
#6939 = ORIENTED_EDGE ( 'NONE', *, *, #48204, .F. ) ;
#6940 = CARTESIAN_POINT ( 'NONE',  ( -1.451368222102410455, 5.185123052344191130, 3.782134281800667797 ) ) ;
#6941 = DIRECTION ( 'NONE',  ( -0.6427681459581293666, -0.7660444431189770143, -0.005002170337467561935 ) ) ;
#6942 = ORIENTED_EDGE ( 'NONE', *, *, #33046, .F. ) ;
#6943 = VECTOR ( 'NONE', #40869, 1000.000000000000000 ) ;
#6944 = EDGE_CURVE ( 'NONE', #36692, #13999, #28624, .T. ) ;
#6945 = CARTESIAN_POINT ( 'NONE',  ( -67.84970284451081568, 2.000000000000001776, -4.138470222184130520 ) ) ;
#6946 = CARTESIAN_POINT ( 'NONE',  ( -19.12962290826653700, 0.000000000000000000, 14.40064212555863854 ) ) ;
#6947 = AXIS2_PLACEMENT_3D ( 'NONE', #15685, #2630, #50344 ) ;
#6948 = DIRECTION ( 'NONE',  ( 0.5364919789714477361, 0.6444004775717706579, 0.5449076811759711036 ) ) ;
#6949 = ADVANCED_FACE ( 'NONE', ( #41409 ), #14718, .F. ) ;
#6950 = EDGE_CURVE ( 'NONE', #33489, #29959, #10478, .T. ) ;
#6951 = DIRECTION ( 'NONE',  ( 0.005002170337468016433, -0.7660444431189770143, -0.6427681459581293666 ) ) ;
#6952 = VECTOR ( 'NONE', #15524, 999.9999999999998863 ) ;
#6953 = DIRECTION ( 'NONE',  ( 0.9999697198139515519, 0.000000000000000000, 0.007781995580013368816 ) ) ;
#6954 = ORIENTED_EDGE ( 'NONE', *, *, #1165, .F. ) ;
#6955 = AXIS2_PLACEMENT_3D ( 'NONE', #5467, #31604, #14828 ) ;
#6956 = ORIENTED_EDGE ( 'NONE', *, *, #45985, .F. ) ;
#6957 = CARTESIAN_POINT ( 'NONE',  ( -12.33850799832341849, 0.000000000000000000, 11.68350162852954632 ) ) ;
#6958 = DIRECTION ( 'NONE',  ( -0.9999697198139514409, -0.000000000000000000, -0.007781995580013368816 ) ) ;
#6959 = CARTESIAN_POINT ( 'NONE',  ( -9.110551994824897193, 0.000000000000000000, 3.538847790438064411 ) ) ;
#6960 = EDGE_CURVE ( 'NONE', #41338, #51942, #27803, .T. ) ;
#6961 = DIRECTION ( 'NONE',  ( 0.6427681459581294776, -0.7660444431189769032, 0.005002170337467562802 ) ) ;
#6962 = DIRECTION ( 'NONE',  ( 0.000000000000000000, 0.000000000000000000, 1.000000000000000000 ) ) ;
#6963 = EDGE_CURVE ( 'NONE', #3917, #11166, #19816, .T. ) ;
#6964 = LINE ( 'NONE', #10917, #46693 ) ;
#6965 = ORIENTED_EDGE ( 'NONE', *, *, #54241, .T. ) ;
#6966 = CARTESIAN_POINT ( 'NONE',  ( 2.072287782118878319, 0.000000000000000000, -2.950529333540147015 ) ) ;
#6967 = EDGE_CURVE ( 'NONE', #23008, #36173, #24615, .T. ) ;
#6968 = VECTOR ( 'NONE', #13614, 999.9999999999998863 ) ;
#6969 = CARTESIAN_POINT ( 'NONE',  ( -27.99845268667336384, -0.1191753592594197858, 7.657176279295684118 ) ) ;
#6970 = FACE_OUTER_BOUND ( 'NONE', #24754, .T. ) ;
#6971 = ORIENTED_EDGE ( 'NONE', *, *, #24563, .T. ) ;
#6972 = DIRECTION ( 'NONE',  ( 0.000000000000000000, -0.000000000000000000, -1.000000000000000000 ) ) ;
#6973 = PLANE ( 'NONE',  #18663 ) ;
#6974 = LINE ( 'NONE', #46126, #20243 ) ;
#6975 = EDGE_CURVE ( 'NONE', #55993, #27150, #1657, .T. ) ;
#6976 = ORIENTED_EDGE ( 'NONE', *, *, #6679, .F. ) ;
#6977 = LINE ( 'NONE', #46389, #54918 ) ;
#6978 = AXIS2_PLACEMENT_3D ( 'NONE', #24592, #11565, #7282 ) ;
#6979 = ORIENTED_EDGE ( 'NONE', *, *, #53792, .T. ) ;
#6980 = EDGE_CURVE ( 'NONE', #35417, #14078, #18982, .T. ) ;
#6981 = ORIENTED_EDGE ( 'NONE', *, *, #2052, .F. ) ;
#6982 = VECTOR ( 'NONE', #34028, 1000.000000000000000 ) ;
#6983 = ORIENTED_EDGE ( 'NONE', *, *, #51950, .T. ) ;
#6984 = ORIENTED_EDGE ( 'NONE', *, *, #44079, .T. ) ;
#6985 = ORIENTED_EDGE ( 'NONE', *, *, #23359, .F. ) ;
#6986 = DIRECTION ( 'NONE',  ( 0.9999697198139515519, 0.000000000000000000, 0.007781995580013368816 ) ) ;
#6987 = VERTEX_POINT ( 'NONE', #32867 ) ;
#6988 = VECTOR ( 'NONE', #42252, 1000.000000000000000 ) ;
#6989 = ORIENTED_EDGE ( 'NONE', *, *, #44960, .T. ) ;
#6990 = CARTESIAN_POINT ( 'NONE',  ( -14.16520784441536662, 2.229229656569005957, 6.042114544152918043 ) ) ;
#6991 = VERTEX_POINT ( 'NONE', #45945 ) ;
#6992 = ORIENTED_EDGE ( 'NONE', *, *, #41203, .T. ) ;
#6993 = VECTOR ( 'NONE', #50290, 1000.000000000000227 ) ;
#6994 = CARTESIAN_POINT ( 'NONE',  ( -18.19747506107908563, 0.000000000000000000, 14.03856424583689311 ) ) ;
#6995 = CARTESIAN_POINT ( 'NONE',  ( -16.03058795173162920, -0.8417996532631574214, 3.081288062448307663 ) ) ;
#6996 = PLANE ( 'NONE',  #25058 ) ;
#6997 = LINE ( 'NONE', #49299, #23276 ) ;
#6998 = CARTESIAN_POINT ( 'NONE',  ( -24.27063949748155380, 0.000000000000000000, 6.308861732390097288 ) ) ;
#6999 = ORIENTED_EDGE ( 'NONE', *, *, #54811, .F. ) ;
#7000 = ORIENTED_EDGE ( 'NONE', *, *, #44997, .F. ) ;
#7001 = CARTESIAN_POINT ( 'NONE',  ( -27.06708303904391144, 0.000000000000000000, 7.395095371555332697 ) ) ;
#7002 = EDGE_CURVE ( 'NONE', #55978, #19207, #49656, .T. ) ;
#7003 = FACE_OUTER_BOUND ( 'NONE', #2731, .T. ) ;
#7004 = VECTOR ( 'NONE', #48880, 999.9999999999998863 ) ;
#7005 = FACE_OUTER_BOUND ( 'NONE', #6638, .T. ) ;
#7006 = EDGE_CURVE ( 'NONE', #38002, #25423, #32597, .T. ) ;
#7007 = PLANE ( 'NONE',  #31386 ) ;
#7008 = CARTESIAN_POINT ( 'NONE',  ( -12.74611667447084251, 0.000000000000000000, 4.351881828530372864 ) ) ;
#7009 = LINE ( 'NONE', #10960, #30437 ) ;
#7010 = ORIENTED_EDGE ( 'NONE', *, *, #39150, .F. ) ;
#7011 = CARTESIAN_POINT ( 'NONE',  ( -13.07066190154808361, 0.000000000000000000, 12.04713590736729678 ) ) ;
#7012 = VERTEX_POINT ( 'NONE', #1912 ) ;
#7013 = EDGE_CURVE ( 'NONE', #7579, #27972, #24352, .T. ) ;
#7014 = FACE_OUTER_BOUND ( 'NONE', #40520, .T. ) ;
#7015 = PLANE ( 'NONE',  #42356 ) ;
#7017 = DIRECTION ( 'NONE',  ( -0.7660212471507179544, -0.6427876096865405842, -0.005961354470445141482 ) ) ;
#7016 = AXIS2_PLACEMENT_3D ( 'NONE', #21113, #8636, #12880 ) ;
#7018 = CARTESIAN_POINT ( 'NONE',  ( -15.13495153988577968, 0.000000000000000000, 12.76973526769478084 ) ) ;
#7019 = EDGE_CURVE ( 'NONE', #17655, #33054, #19246, .T. ) ;
#7020 = CARTESIAN_POINT ( 'NONE',  ( -15.88053067323648371, -0.1191753592594190225, 2.950163842912993939 ) ) ;
#7021 = CIRCLE ( 'NONE', #30582, 2.125000000000000000 ) ;
#7022 = ORIENTED_EDGE ( 'NONE', *, *, #766, .F. ) ;
#7023 = DIRECTION ( 'NONE',  ( 0.000000000000000000, -5.782411586589354681E-16, 1.000000000000000000 ) ) ;
#7024 = DIRECTION ( 'NONE',  ( 0.6427681459581294776, -0.7660444431189769032, 0.005002170337467562802 ) ) ;
#7025 = DIRECTION ( 'NONE',  ( 0.005002170337468016433, -0.7660444431189770143, -0.6427681459581293666 ) ) ;
#7026 = AXIS2_PLACEMENT_3D ( 'NONE', #8681, #20618, #43325 ) ;
#7027 = FACE_OUTER_BOUND ( 'NONE', #31184, .T. ) ;
#7028 = EDGE_CURVE ( 'NONE', #873, #46046, #37398, .T. ) ;
#7029 = CARTESIAN_POINT ( 'NONE',  ( 2.072287782118878319, 0.000000000000000000, -2.950529333540147015 ) ) ;
#7030 = LINE ( 'NONE', #2175, #4623 ) ;
#7031 = CARTESIAN_POINT ( 'NONE',  ( -10.94028622754223967, 0.000000000000000000, 11.14038480894692995 ) ) ;
#7032 = ADVANCED_FACE ( 'NONE', ( #54720 ), #19538, .F. ) ;
#7033 = FACE_OUTER_BOUND ( 'NONE', #18093, .T. ) ;
#7034 = CARTESIAN_POINT ( 'NONE',  ( -23.33849165029409889, 0.000000000000000000, 5.946783852668351855 ) ) ;
#7035 = ORIENTED_EDGE ( 'NONE', *, *, #49838, .T. ) ;
#7036 = ADVANCED_FACE ( 'NONE', ( #16124 ), #55873, .F. ) ;
#7037 = ORIENTED_EDGE ( 'NONE', *, *, #2880, .F. ) ;
#7038 = EDGE_CURVE ( 'NONE', #20767, #39658, #47058, .T. ) ;
#7039 = ORIENTED_EDGE ( 'NONE', *, *, #33930, .F. ) ;
#7040 = ORIENTED_EDGE ( 'NONE', *, *, #47911, .F. ) ;
#7041 = VERTEX_POINT ( 'NONE', #3613 ) ;
#7042 = VERTEX_POINT ( 'NONE', #33702 ) ;
#7043 = LINE ( 'NONE', #41401, #4243 ) ;
#7044 = CARTESIAN_POINT ( 'NONE',  ( -20.48739968382506405, 3.686347215771509589, 4.522319747380798560 ) ) ;
#7045 = PLANE ( 'NONE',  #27643 ) ;
#7046 = ORIENTED_EDGE ( 'NONE', *, *, #20839, .F. ) ;
#7047 = EDGE_LOOP ( 'NONE', ( #3544, #29454, #16168, #24602, #55140 ) ) ;
#7048 = VERTEX_POINT ( 'NONE', #29160 ) ;
#7049 = PLANE ( 'NONE',  #20454 ) ;
#7050 = ORIENTED_EDGE ( 'NONE', *, *, #7885, .F. ) ;
#7051 = VECTOR ( 'NONE', #50149, 1000.000000000000000 ) ;
#7052 = CARTESIAN_POINT ( 'NONE',  ( -65.97914594675513911, -9.260704868562440240, -1.425848428488597053 ) ) ;
#7053 = DIRECTION ( 'NONE',  ( 0.007781995580012663651, -3.146120232559066537E-19, -0.9999697198139514409 ) ) ;
#7054 = DIRECTION ( 'NONE',  ( 0.007781995580012662783, 0.000000000000000000, -0.9999697198139514409 ) ) ;
#7055 = ORIENTED_EDGE ( 'NONE', *, *, #33265, .T. ) ;
#7056 = PLANE ( 'NONE',  #39160 ) ;
#7057 = ORIENTED_EDGE ( 'NONE', *, *, #55520, .F. ) ;
#7058 = AXIS2_PLACEMENT_3D ( 'NONE', #5732, #13433, #18217 ) ;
#7059 = DIRECTION ( 'NONE',  ( 0.5364919789714477361, 0.6444004775717706579, 0.5449076811759711036 ) ) ;
#7060 = EDGE_CURVE ( 'NONE', #25539, #30922, #56145, .T. ) ;
#7061 = PLANE ( 'NONE',  #44775 ) ;
#7062 = FACE_OUTER_BOUND ( 'NONE', #19501, .T. ) ;
#7063 = LINE ( 'NONE', #19548, #35134 ) ;
#7064 = ADVANCED_FACE ( 'NONE', ( #8163 ), #42779, .F. ) ;
#7065 = DIRECTION ( 'NONE',  ( 0.9999697198139515519, 0.000000000000000000, 0.007781995580013368816 ) ) ;
#7066 = DIRECTION ( 'NONE',  ( -0.7660212471507179544, -0.6427876096865405842, -0.005961354470445141482 ) ) ;
#7067 = CARTESIAN_POINT ( 'NONE',  ( -31.72782227498118601, 0.000000000000000000, 9.205484770164058972 ) ) ;
#7068 = EDGE_CURVE ( 'NONE', #43270, #30652, #41934, .T. ) ;
#7069 = DIRECTION ( 'NONE',  ( -0.5449076811759708816, 0.6444004775717707689, 0.5364919789714475140 ) ) ;
#7070 = DIRECTION ( 'NONE',  ( 0.000000000000000000, -1.000000000000000000, 0.000000000000000000 ) ) ;
#7071 = EDGE_LOOP ( 'NONE', ( #24673, #2794, #53827, #55925 ) ) ;
#7072 = LINE ( 'NONE', #7918, #39225 ) ;
#7073 = ORIENTED_EDGE ( 'NONE', *, *, #2534, .T. ) ;
#7074 = EDGE_CURVE ( 'NONE', #33995, #10709, #51601, .T. ) ;
#7075 = EDGE_CURVE ( 'NONE', #50804, #12359, #46786, .T. ) ;
#7076 = EDGE_CURVE ( 'NONE', #16783, #48336, #3037, .T. ) ;
#7077 = CARTESIAN_POINT ( 'NONE',  ( -25.20278734466900517, 0.000000000000000000, 6.670939612111840944 ) ) ;
#7078 = DIRECTION ( 'NONE',  ( -0.7660212471507179544, -0.6427876096865405842, -0.005961354470445141482 ) ) ;
#7079 = FACE_OUTER_BOUND ( 'NONE', #16825, .T. ) ;
#7080 = CARTESIAN_POINT ( 'NONE',  ( -27.06552663992790997, 0.000000000000000000, 7.195101427592543786 ) ) ;
#7081 = FACE_OUTER_BOUND ( 'NONE', #13026, .T. ) ;
#7082 = LINE ( 'NONE', #28930, #45538 ) ;
#7083 = FILL_AREA_STYLE_COLOUR ( '', #10850 ) ;
#7084 = VERTEX_POINT ( 'NONE', #21519 ) ;
#7085 = PLANE ( 'NONE',  #2024 ) ;
#7086 = LINE ( 'NONE', #10778, #23910 ) ;
#7087 = DIRECTION ( 'NONE',  ( 0.6427681459581294776, -0.7660444431189769032, 0.005002170337467562802 ) ) ;
#7088 = CARTESIAN_POINT ( 'NONE',  ( -17.74482636761137044, -0.1191753592594197858, 3.674319602356483916 ) ) ;
#7089 = DIRECTION ( 'NONE',  ( 0.9999697198139515519, 0.000000000000000000, 0.007781995580013368816 ) ) ;
#7090 = LINE ( 'NONE', #3642, #11895 ) ;
#7091 = EDGE_CURVE ( 'NONE', #42498, #29609, #3885, .T. ) ;
#7092 = FACE_OUTER_BOUND ( 'NONE', #48936, .T. ) ;
#7093 = CARTESIAN_POINT ( 'NONE',  ( -28.92982233430281980, 0.000000000000000000, 7.919257187036034651 ) ) ;
#7094 = LINE ( 'NONE', #49404, #37422 ) ;
#7095 = EDGE_LOOP ( 'NONE', ( #48864, #17265, #20511, #29446 ) ) ;
#7096 = EDGE_CURVE ( 'NONE', #9163, #46599, #21210, .T. ) ;
#7097 = DIRECTION ( 'NONE',  ( 0.9999697198139515519, 0.000000000000000000, 0.007781995580013368816 ) ) ;
#7098 = VERTEX_POINT ( 'NONE', #25214 ) ;
#7099 = ADVANCED_FACE ( 'NONE', ( #48377 ), #30019, .F. ) ;
#7100 = DIRECTION ( 'NONE',  ( -0.005961354470445682716, -0.6427876096865404731, 0.7660212471507180654 ) ) ;
#7101 = CARTESIAN_POINT ( 'NONE',  ( -19.36023273628322983, -4.727446477803162850, 11.96064866101106716 ) ) ;
#7102 = EDGE_CURVE ( 'NONE', #47628, #3649, #20920, .T. ) ;
#7103 = VECTOR ( 'NONE', #13761, 1000.000000000000000 ) ;
#7104 = ORIENTED_EDGE ( 'NONE', *, *, #46221, .T. ) ;
#7105 = ORIENTED_EDGE ( 'NONE', *, *, #21392, .T. ) ;
#7106 = CARTESIAN_POINT ( 'NONE',  ( -0.8462754142284378833, 3.710276453311750267, 3.547095686184165153 ) ) ;
#7107 = ORIENTED_EDGE ( 'NONE', *, *, #54546, .F. ) ;
#7108 = ORIENTED_EDGE ( 'NONE', *, *, #39592, .F. ) ;
#7109 = VERTEX_POINT ( 'NONE', #29762 ) ;
#7110 = PLANE ( 'NONE',  #36563 ) ;
#7111 = CARTESIAN_POINT ( 'NONE',  ( -66.91760232564914190, -9.368321606677067592, -6.901381173728423413 ) ) ;
#7112 = LINE ( 'NONE', #16176, #5843 ) ;
#7113 = ORIENTED_EDGE ( 'NONE', *, *, #41797, .T. ) ;
#7114 = ORIENTED_EDGE ( 'NONE', *, *, #26471, .F. ) ;
#7115 = DIRECTION ( 'NONE',  ( 0.5364919789714477361, 0.6444004775717706579, 0.5449076811759711036 ) ) ;
#7116 = CARTESIAN_POINT ( 'NONE',  ( -18.29747203306047609, -0.1191753592594177458, 14.03778604627889059 ) ) ;
#7117 = EDGE_LOOP ( 'NONE', ( #40148, #21455, #42706, #34078 ) ) ;
#7118 = CARTESIAN_POINT ( 'NONE',  ( -27.06552663992790997, 0.000000000000000000, 7.195101427592543786 ) ) ;
#7119 = ORIENTED_EDGE ( 'NONE', *, *, #17490, .F. ) ;
#7120 = DIRECTION ( 'NONE',  ( 0.007781995580012662783, 0.000000000000000000, -0.9999697198139514409 ) ) ;
#7121 = CARTESIAN_POINT ( 'NONE',  ( -16.06709938707323460, 0.000000000000000000, 13.13181314741652628 ) ) ;
#7122 = ORIENTED_EDGE ( 'NONE', *, *, #25788, .T. ) ;
#7123 = CARTESIAN_POINT ( 'NONE',  ( -14.93495759592298988, 0.000000000000000000, 12.77129166681078409 ) ) ;
#7124 = FACE_OUTER_BOUND ( 'NONE', #46118, .T. ) ;
#7125 = ORIENTED_EDGE ( 'NONE', *, *, #23973, .T. ) ;
#7126 = LINE ( 'NONE', #53977, #12221 ) ;
#7127 = LINE ( 'NONE', #45441, #27559 ) ;
#7128 = DIRECTION ( 'NONE',  ( 0.6427681459581294776, -0.7660444431189769032, 0.005002170337467562802 ) ) ;
#7129 = ORIENTED_EDGE ( 'NONE', *, *, #44539, .F. ) ;
#7130 = ADVANCED_FACE ( 'NONE', ( #24921 ), #25760, .F. ) ;
#7131 = ADVANCED_FACE ( 'NONE', ( #42244 ), #13737, .F. ) ;
#7132 = AXIS2_PLACEMENT_3D ( 'NONE', #14292, #17690, #48908 ) ;
#7133 = PLANE ( 'NONE',  #43727 ) ;
#7134 = CARTESIAN_POINT ( 'NONE',  ( -3.360905869600907092, 1.712176620043476140E-14, -3.600000000000000089 ) ) ;
#7135 = PLANE ( 'NONE',  #55708 ) ;
#7136 = DIRECTION ( 'NONE',  ( -0.5449076811759708816, 0.6444004775717707689, 0.5364919789714475140 ) ) ;
#7137 = EDGE_CURVE ( 'NONE', #33896, #29311, #20668, .T. ) ;
#7138 = CARTESIAN_POINT ( 'NONE',  ( -9.442067484779661513, -0.1191753592594197858, 10.59804618892231254 ) ) ;
#7139 = FACE_OUTER_BOUND ( 'NONE', #22201, .T. ) ;
#7140 = CARTESIAN_POINT ( 'NONE',  ( -67.75725311154501185, -11.47771511529060007, -8.849861037685116116 ) ) ;
#7141 = EDGE_LOOP ( 'NONE', ( #49008, #7470, #34409, #686 ) ) ;
#7142 = CARTESIAN_POINT ( 'NONE',  ( -20.54049170961573267, 0.000000000000000000, 4.660556269540326646 ) ) ;
#7143 = CARTESIAN_POINT ( 'NONE',  ( -22.64140378624534833, -5.375054281893165253, 5.504518879977243095 ) ) ;
#7144 = CARTESIAN_POINT ( 'NONE',  ( -69.24996902294029155, -0.6012229694362068999, 7.030741166005281428 ) ) ;
#7145 = EDGE_LOOP ( 'NONE', ( #22747, #33256, #14511, #3103 ) ) ;
#7146 = CARTESIAN_POINT ( 'NONE',  ( -15.87975247367846166, 0.000000000000000000, 2.850166870931599927 ) ) ;
#7147 = LINE ( 'NONE', #54276, #40877 ) ;
#7148 = CARTESIAN_POINT ( 'NONE',  ( -16.41782547135460391, -0.1941918491731542684, 3.252366345260954805 ) ) ;
#7149 = DIRECTION ( 'NONE',  ( 0.005961354470445682716, -0.6427876096865404731, -0.7660212471507180654 ) ) ;
#7150 = ADVANCED_FACE ( 'NONE', ( #9793 ), #14332, .F. ) ;
#7151 = CARTESIAN_POINT ( 'NONE',  ( -13.30267207010766839, 4.010151117816511679, 1.721196508061384023 ) ) ;
#7152 = ORIENTED_EDGE ( 'NONE', *, *, #2260, .T. ) ;
#7153 = EDGE_LOOP ( 'NONE', ( #50530, #28836, #31836, #34535 ) ) ;
#7154 = EDGE_CURVE ( 'NONE', #21504, #10403, #14203, .T. ) ;
#7155 = FACE_OUTER_BOUND ( 'NONE', #51508, .T. ) ;
#7156 = DIRECTION ( 'NONE',  ( 0.6427681459581294776, -0.7660444431189769032, 0.005002170337467562802 ) ) ;
#7157 = DIRECTION ( 'NONE',  ( -0.5449076811759708816, 0.6444004775717707689, 0.5364919789714475140 ) ) ;
#7158 = ADVANCED_FACE ( 'NONE', ( #49218 ), #35912, .F. ) ;
#7159 = ORIENTED_EDGE ( 'NONE', *, *, #48328, .F. ) ;
#7160 = CARTESIAN_POINT ( 'NONE',  ( -14.05805291360240261, -0.1191753592594190225, 6.657667484312323580 ) ) ;
#7161 = ORIENTED_EDGE ( 'NONE', *, *, #24253, .F. ) ;
#7162 = DIRECTION ( 'NONE',  ( 0.5449076811759707706, 0.6444004775717708799, -0.5364919789714476250 ) ) ;
#7163 = EDGE_CURVE ( 'NONE', #51867, #1451, #1786, .T. ) ;
#7164 = ORIENTED_EDGE ( 'NONE', *, *, #28272, .F. ) ;
#7165 = ORIENTED_EDGE ( 'NONE', *, *, #16838, .F. ) ;
#7166 = CARTESIAN_POINT ( 'NONE',  ( -18.66354898467281132, 0.000000000000000000, 14.21960318569776582 ) ) ;
#7167 = FACE_OUTER_BOUND ( 'NONE', #38365, .T. ) ;
#7168 = DIRECTION ( 'NONE',  ( -0.9999697198139514409, -0.000000000000000000, -0.007781995580013368816 ) ) ;
#7169 = ORIENTED_EDGE ( 'NONE', *, *, #29158, .F. ) ;
#7170 = AXIS2_PLACEMENT_3D ( 'NONE', #2583, #45455, #23881 ) ;
#7171 = CARTESIAN_POINT ( 'NONE',  ( -13.17065887352947762, -0.1191753592594197858, 12.04635770780929427 ) ) ;
#7172 = ORIENTED_EDGE ( 'NONE', *, *, #23422, .F. ) ;
#7173 = EDGE_LOOP ( 'NONE', ( #17696, #38260, #43587, #46463 ) ) ;
#7174 = ORIENTED_EDGE ( 'NONE', *, *, #41913, .T. ) ;
#7175 = CARTESIAN_POINT ( 'NONE',  ( -13.53673582514181106, 0.000000000000000000, 12.22817484722816772 ) ) ;
#7176 = CARTESIAN_POINT ( 'NONE',  ( -16.33317936670417225, 0.000000000000000000, 13.31440848639340224 ) ) ;
#7177 = ORIENTED_EDGE ( 'NONE', *, *, #11568, .F. ) ;
#7178 = DIRECTION ( 'NONE',  ( 0.005002170337468016433, -0.7660444431189770143, -0.6427681459581293666 ) ) ;
#7179 = ORIENTED_EDGE ( 'NONE', *, *, #5487, .T. ) ;
#7180 = LINE ( 'NONE', #19386, #11337 ) ;
#7181 = CARTESIAN_POINT ( 'NONE',  ( -11.40636015113596180, 0.000000000000000000, 11.32142374880780089 ) ) ;
#7182 = ORIENTED_EDGE ( 'NONE', *, *, #9445, .F. ) ;
#7183 = FACE_OUTER_BOUND ( 'NONE', #26999, .T. ) ;
#7184 = ORIENTED_EDGE ( 'NONE', *, *, #672, .F. ) ;
#7185 = CARTESIAN_POINT ( 'NONE',  ( -14.93495759592298988, 0.000000000000000000, 12.77129166681078409 ) ) ;
#7186 = PLANE ( 'NONE',  #19348 ) ;
#7187 = PLANE ( 'NONE',  #13264 ) ;
#7188 = CARTESIAN_POINT ( 'NONE',  ( -13.03950016240196597, 0.000000000000000000, 8.042919348456010198 ) ) ;
#7189 = CARTESIAN_POINT ( 'NONE',  ( -26.26580391614848864, 17.49370688441070953, -4.657437592157546824 ) ) ;
#7190 = CARTESIAN_POINT ( 'NONE',  ( -15.42180871032122091, -0.1191753592594190225, 2.771980654253273002 ) ) ;
#7191 = ORIENTED_EDGE ( 'NONE', *, *, #44195, .F. ) ;
#7192 = ADVANCED_FACE ( 'NONE', ( #49786 ), #36437, .F. ) ;
#7193 = VERTEX_POINT ( 'NONE', #44401 ) ;
#7194 = PLANE ( 'NONE',  #40046 ) ;
#7195 = CARTESIAN_POINT ( 'NONE',  ( -8.878251335088286567, 6.547824941322106795, 0.2302407495689529626 ) ) ;
#7196 = DIRECTION ( 'NONE',  ( 0.007781995580012663651, 0.000000000000000000, -0.9999697198139515519 ) ) ;
#7197 = EDGE_CURVE ( 'NONE', #27809, #20135, #26815, .T. ) ;
#7198 = ADVANCED_FACE ( 'NONE', ( #14586 ), #32195, .F. ) ;
#7199 = CARTESIAN_POINT ( 'NONE',  ( -15.57823159443524119, 0.6102101463440037232, 3.933894115644549050 ) ) ;
#7200 = CARTESIAN_POINT ( 'NONE',  ( -30.79567442779373110, 0.000000000000000000, 8.843406890442315316 ) ) ;
#7201 = CARTESIAN_POINT ( 'NONE',  ( -10.74029228357944987, 0.000000000000000000, 11.14194120806293320 ) ) ;
#7202 = ORIENTED_EDGE ( 'NONE', *, *, #23360, .F. ) ;
#7203 = DIRECTION ( 'NONE',  ( -0.5449076811759708816, 0.6444004775717707689, 0.5364919789714475140 ) ) ;
#7204 = PLANE ( 'NONE',  #34124 ) ;
#7205 = VERTEX_POINT ( 'NONE', #18863 ) ;
#7206 = DIRECTION ( 'NONE',  ( 0.9999697198139515519, 0.000000000000000000, 0.007781995580013368816 ) ) ;
#7207 = DIRECTION ( 'NONE',  ( 0.9999697198139515519, 0.000000000000000000, 0.007781995580013368816 ) ) ;
#7208 = ORIENTED_EDGE ( 'NONE', *, *, #21365, .F. ) ;
#7209 = DIRECTION ( 'NONE',  ( -0.5449076811759708816, 0.6444004775717707689, 0.5364919789714475140 ) ) ;
#7210 = LINE ( 'NONE', #24799, #45955 ) ;
#7211 = CARTESIAN_POINT ( 'NONE',  ( -14.06667507411825113, -0.1191753592594177180, 7.765596594085615756 ) ) ;
#7212 = DIRECTION ( 'NONE',  ( 0.5364919789714477361, 0.6444004775717706579, 0.5449076811759711036 ) ) ;
#7213 = CARTESIAN_POINT ( 'NONE',  ( -58.00000000000000711, -9.000000000000000000, 7.102951435054649637E-15 ) ) ;
#7214 = ORIENTED_EDGE ( 'NONE', *, *, #24051, .T. ) ;
#7215 = EDGE_LOOP ( 'NONE', ( #32331, #27930, #18466, #10040 ) ) ;
#7216 = LINE ( 'NONE', #10367, #42062 ) ;
#7217 = DIRECTION ( 'NONE',  ( 0.005002170337468016433, -0.7660444431189770143, -0.6427681459581293666 ) ) ;
#7218 = CARTESIAN_POINT ( 'NONE',  ( -18.67775241435682432, 0.000000000000000000, 4.136394454059623804 ) ) ;
#7219 = DIRECTION ( 'NONE',  ( -0.9999697198139514409, -0.000000000000000000, -0.007781995580013368816 ) ) ;
#7220 = LINE ( 'NONE', #37892, #20118 ) ;
#7221 = CARTESIAN_POINT ( 'NONE',  ( -18.13326170662221415, 0.000000000000000000, 5.787286099461318223 ) ) ;
#7222 = ORIENTED_EDGE ( 'NONE', *, *, #55454, .T. ) ;
#7223 = CARTESIAN_POINT ( 'NONE',  ( -12.34488701508258224, -3.108426967578160838, 1.577319373299684857 ) ) ;
#7224 = ADVANCED_FACE ( 'NONE', ( #53750 ), #6099, .F. ) ;
#7225 = CARTESIAN_POINT ( 'NONE',  ( -9.110551994824897193, 0.000000000000000000, 3.538847790438064411 ) ) ;
#7226 = DIRECTION ( 'NONE',  ( 0.5449076811759707706, 0.6444004775717708799, -0.5364919789714476250 ) ) ;
#7227 = EDGE_LOOP ( 'NONE', ( #27587, #54717, #21827, #3055, #53404 ) ) ;
#7228 = EDGE_CURVE ( 'NONE', #7431, #16954, #6349, .T. ) ;
#7229 = CARTESIAN_POINT ( 'NONE',  ( -25.20123094555300369, 0.000000000000000000, 6.470945668149052032 ) ) ;
#7230 = PLANE ( 'NONE',  #29569 ) ;
#7231 = EDGE_CURVE ( 'NONE', #16077, #10405, #23651, .T. ) ;
#7232 = DIRECTION ( 'NONE',  ( -0.7660212471507179544, -0.6427876096865405842, -0.005961354470445141482 ) ) ;
#7233 = ORIENTED_EDGE ( 'NONE', *, *, #6131, .F. ) ;
#7234 = LINE ( 'NONE', #16045, #15041 ) ;
#7235 = ADVANCED_FACE ( 'NONE', ( #48951 ), #10043, .F. ) ;
#7236 = ORIENTED_EDGE ( 'NONE', *, *, #42285, .T. ) ;
#7237 = ORIENTED_EDGE ( 'NONE', *, *, #16116, .F. ) ;
#7238 = ORIENTED_EDGE ( 'NONE', *, *, #28815, .T. ) ;
#7239 = VERTEX_POINT ( 'NONE', #44673 ) ;
#7240 = EDGE_LOOP ( 'NONE', ( #39555, #20125, #24406, #50361 ) ) ;
#7241 = FACE_OUTER_BOUND ( 'NONE', #22292, .T. ) ;
#7242 = ORIENTED_EDGE ( 'NONE', *, *, #23546, .F. ) ;
#7243 = ORIENTED_EDGE ( 'NONE', *, *, #46969, .T. ) ;
#7244 = FACE_OUTER_BOUND ( 'NONE', #5773, .T. ) ;
#7245 = ORIENTED_EDGE ( 'NONE', *, *, #38550, .T. ) ;
#7246 = EDGE_LOOP ( 'NONE', ( #44820, #21683, #16798, #12114 ) ) ;
#7247 = ADVANCED_FACE ( 'NONE', ( #19392 ), #40445, .F. ) ;
#7248 = FACE_OUTER_BOUND ( 'NONE', #13283, .T. ) ;
#7249 = DIRECTION ( 'NONE',  ( 0.5449076811759707706, 0.6444004775717708799, -0.5364919789714476250 ) ) ;
#7250 = DIRECTION ( 'NONE',  ( 0.005961354470445682716, -0.6427876096865404731, -0.7660212471507180654 ) ) ;
#7251 = CARTESIAN_POINT ( 'NONE',  ( -20.60218203966579864, 2.714935509636508204, 4.597898231738893671 ) ) ;
#7252 = EDGE_CURVE ( 'NONE', #22744, #36173, #5252, .T. ) ;
#7253 = LINE ( 'NONE', #37923, #11993 ) ;
#7254 = ORIENTED_EDGE ( 'NONE', *, *, #8648, .T. ) ;
#7255 = ORIENTED_EDGE ( 'NONE', *, *, #25517, .T. ) ;
#7256 = EDGE_CURVE ( 'NONE', #19170, #12005, #1534, .T. ) ;
#7257 = CARTESIAN_POINT ( 'NONE',  ( -55.47117325737978888, 6.581829179614757663, -1.080525476705088916 ) ) ;
#7258 = CARTESIAN_POINT ( 'NONE',  ( -11.21901323774118708, 0.000000000000000000, 1.039777472322872098 ) ) ;
#7259 = ADVANCED_FACE ( 'NONE', ( #10331 ), #948, .F. ) ;
#7260 = CARTESIAN_POINT ( 'NONE',  ( -26.13337879274045505, 0.000000000000000000, 6.833023547870798353 ) ) ;
#7261 = CARTESIAN_POINT ( 'NONE',  ( -15.88053067323646417, -0.1191753592594197858, 2.950163842912994383 ) ) ;
#7262 = CARTESIAN_POINT ( 'NONE',  ( -12.73330280606043097, 0.000000000000000000, 2.705327256204338671 ) ) ;
#7263 = EDGE_LOOP ( 'NONE', ( #41067, #5901, #18043, #10744 ) ) ;
#7264 = FACE_OUTER_BOUND ( 'NONE', #43826, .T. ) ;
#7265 = ORIENTED_EDGE ( 'NONE', *, *, #34974, .F. ) ;
#7266 = CARTESIAN_POINT ( 'NONE',  ( -13.53673582514181106, 0.000000000000000000, 12.22817484722816772 ) ) ;
#7267 = FACE_OUTER_BOUND ( 'NONE', #16725, .T. ) ;
#7268 = FACE_OUTER_BOUND ( 'NONE', #54246, .T. ) ;
#7269 = CARTESIAN_POINT ( 'NONE',  ( -15.13495153988577968, 0.000000000000000000, 12.76973526769478084 ) ) ;
#7270 = CARTESIAN_POINT ( 'NONE',  ( -25.20123094555300369, 0.000000000000000000, 6.470945668149052032 ) ) ;
#7271 = EDGE_CURVE ( 'NONE', #23572, #52995, #37016, .T. ) ;
#7272 = AXIS2_PLACEMENT_3D ( 'NONE', #42196, #55247, #29417 ) ;
#7273 = ORIENTED_EDGE ( 'NONE', *, *, #16541, .F. ) ;
#7274 = VERTEX_POINT ( 'NONE', #42088 ) ;
#7275 = CARTESIAN_POINT ( 'NONE',  ( -19.49786065871724006, 4.172053068839010059, 4.122452625480004684 ) ) ;
#7276 = DIRECTION ( 'NONE',  ( 0.5364919789714477361, 0.6444004775717706579, 0.5449076811759711036 ) ) ;
#7277 = CARTESIAN_POINT ( 'NONE',  ( -12.60458797795435615, 0.000000000000000000, 11.86609696750642229 ) ) ;
#7278 = FACE_OUTER_BOUND ( 'NONE', #23375, .T. ) ;
#7279 = LINE ( 'NONE', #11561, #40292 ) ;
#7280 = FACE_OUTER_BOUND ( 'NONE', #43465, .T. ) ;
#7281 = DIRECTION ( 'NONE',  ( -0.5449076811759708816, 0.6444004775717707689, 0.5364919789714475140 ) ) ;
#7282 = DIRECTION ( 'NONE',  ( -0.005002170337468016433, -0.7660444431189770143, 0.6427681459581293666 ) ) ;
#7283 = CARTESIAN_POINT ( 'NONE',  ( -22.02230666951336246, 19.67040017278726438, 4.420763615217817133 ) ) ;
#7284 = ORIENTED_EDGE ( 'NONE', *, *, #53807, .F. ) ;
#7285 = EDGE_CURVE ( 'NONE', #41663, #17974, #20530, .T. ) ;
#7286 = EDGE_LOOP ( 'NONE', ( #50859, #12695, #12469, #47159 ) ) ;
#7287 = ORIENTED_EDGE ( 'NONE', *, *, #14689, .F. ) ;
#7288 = ORIENTED_EDGE ( 'NONE', *, *, #6366, .T. ) ;
#7289 = ORIENTED_EDGE ( 'NONE', *, *, #15125, .F. ) ;
#7290 = CARTESIAN_POINT ( 'NONE',  ( -14.93495759592298988, 0.000000000000000000, 12.77129166681078409 ) ) ;
#7291 = LINE ( 'NONE', #3025, #43821 ) ;
#7292 = CARTESIAN_POINT ( 'NONE',  ( -67.81626209598535127, 0.000000000000000000, 7.454917401049828918 ) ) ;
#7293 = EDGE_CURVE ( 'NONE', #9458, #49209, #50624, .T. ) ;
#7294 = ORIENTED_EDGE ( 'NONE', *, *, #29078, .F. ) ;
#7295 = ORIENTED_EDGE ( 'NONE', *, *, #21527, .T. ) ;
#7296 = EDGE_LOOP ( 'NONE', ( #19943, #41513, #50942, #19681, #35246 ) ) ;
#7297 = FACE_OUTER_BOUND ( 'NONE', #30712, .T. ) ;
#7298 = EDGE_CURVE ( 'NONE', #6114, #22808, #45501, .T. ) ;
#7299 = EDGE_LOOP ( 'NONE', ( #15333, #4560, #25063, #42109 ) ) ;
#7300 = EDGE_CURVE ( 'NONE', #41467, #16440, #29034, .T. ) ;
#7301 = VECTOR ( 'NONE', #31307, 999.9999999999998863 ) ;
#7302 = CARTESIAN_POINT ( 'NONE',  ( -68.96686481439014926, -9.000268183362885921, 7.306242118345172898 ) ) ;
#7303 = CARTESIAN_POINT ( 'NONE',  ( -13.27065584551087163, 0.000000000000000000, 12.04557950825129176 ) ) ;
#7304 = FACE_OUTER_BOUND ( 'NONE', #29447, .T. ) ;
#7305 = EDGE_CURVE ( 'NONE', #21379, #43081, #28189, .T. ) ;
#7306 = ORIENTED_EDGE ( 'NONE', *, *, #23052, .T. ) ;
#7307 = CARTESIAN_POINT ( 'NONE',  ( -11.04000237409175078, -1.003701604285657911, 1.137609623205984244 ) ) ;
#7308 = EDGE_LOOP ( 'NONE', ( #48443, #31680, #39904, #36091 ) ) ;
#7309 = CARTESIAN_POINT ( 'NONE',  ( -15.60102546347950536, 0.000000000000000000, 12.95077420755565356 ) ) ;
#7310 = ADVANCED_FACE ( 'NONE', ( #3195 ), #54880, .F. ) ;
#7311 = CARTESIAN_POINT ( 'NONE',  ( -17.14604581469821909, 3.038739411681509850, 3.245086511306461752 ) ) ;
#7312 = ADVANCED_FACE ( 'NONE', ( #37858 ), #19949, .F. ) ;
#7313 = LINE ( 'NONE', #11847, #6988 ) ;
#7314 = PLANE ( 'NONE',  #43126 ) ;
#7315 = PLANE ( 'NONE',  #9326 ) ;
#7316 = DIRECTION ( 'NONE',  ( 0.007781995580012663651, -3.146120232559066537E-19, -0.9999697198139514409 ) ) ;
#7317 = CARTESIAN_POINT ( 'NONE',  ( -11.67244013076689946, 0.000000000000000000, 11.50401908778467863 ) ) ;
#7318 = FACE_OUTER_BOUND ( 'NONE', #42612, .T. ) ;
#7319 = ORIENTED_EDGE ( 'NONE', *, *, #25183, .F. ) ;
#7320 = LINE ( 'NONE', #45660, #13814 ) ;
#7321 = ORIENTED_EDGE ( 'NONE', *, *, #851, .F. ) ;
#7322 = EDGE_CURVE ( 'NONE', #9106, #10102, #55164, .T. ) ;
#7323 = VECTOR ( 'NONE', #47770, 999.9999999999998863 ) ;
#7324 = DIRECTION ( 'NONE',  ( 0.9999697198139515519, 0.000000000000000000, 0.007781995580013368816 ) ) ;
#7325 = LINE ( 'NONE', #29184, #5156 ) ;
#7326 = CARTESIAN_POINT ( 'NONE',  ( -14.94916102560700821, 0.000000000000000000, 2.688082935172642962 ) ) ;
#7327 = LINE ( 'NONE', #2226, #12368 ) ;
#7328 = DIRECTION ( 'NONE',  ( -0.005002170337468016433, -0.7660444431189770143, 0.6427681459581293666 ) ) ;
#7329 = EDGE_CURVE ( 'NONE', #19098, #48276, #28775, .T. ) ;
#7330 = CARTESIAN_POINT ( 'NONE',  ( -15.03495456790438389, -0.1191753592594197858, 12.77051346725278158 ) ) ;
#7331 = ORIENTED_EDGE ( 'NONE', *, *, #12950, .F. ) ;
#7332 = DIRECTION ( 'NONE',  ( 0.6427681459581294776, -0.7660444431189769032, 0.005002170337467562802 ) ) ;
#7333 = CARTESIAN_POINT ( 'NONE',  ( -11.67244013076689946, 0.000000000000000000, 11.50401908778467863 ) ) ;
#7334 = DIRECTION ( 'NONE',  ( -0.9999697198139514409, -0.000000000000000000, -0.007781995580013368816 ) ) ;
#7335 = CARTESIAN_POINT ( 'NONE',  ( -13.08408713167409942, -0.1191753592594197858, 1.863930203747758085 ) ) ;
#7336 = FACE_OUTER_BOUND ( 'NONE', #17214, .T. ) ;
#7337 = AXIS2_PLACEMENT_3D ( 'NONE', #31579, #18206, #35533 ) ;
#7338 = DIRECTION ( 'NONE',  ( 0.8531650599175529814, -0.4028455766673920135, -0.3313982828793697877 ) ) ;
#7339 = DIRECTION ( 'NONE',  ( -0.9999697198139514409, -0.000000000000000000, -0.007781995580013368816 ) ) ;
#7340 = LINE ( 'NONE', #54761, #49501 ) ;
#7341 = FACE_OUTER_BOUND ( 'NONE', #29879, .T. ) ;
#7342 = EDGE_LOOP ( 'NONE', ( #52812, #49636, #14250, #10871, #29337 ) ) ;
#7343 = VECTOR ( 'NONE', #17005, 1000.000000000000227 ) ;
#7344 = DIRECTION ( 'NONE',  ( -0.7660212471507179544, -0.6427876096865405842, -0.005961354470445141482 ) ) ;
#7345 = DIRECTION ( 'NONE',  ( 0.7660212471507180654, -0.6427876096865404731, 0.005961354470445141482 ) ) ;
#7346 = ORIENTED_EDGE ( 'NONE', *, *, #7947, .T. ) ;
#7347 = LINE ( 'NONE', #1957, #25940 ) ;
#7348 = DIRECTION ( 'NONE',  ( 0.5364919789714477361, 0.6444004775717706579, 0.5449076811759711036 ) ) ;
#7349 = ORIENTED_EDGE ( 'NONE', *, *, #43431, .T. ) ;
#7350 = EDGE_CURVE ( 'NONE', #16502, #53402, #3483, .T. ) ;
#7351 = ORIENTED_EDGE ( 'NONE', *, *, #8364, .F. ) ;
#7352 = CARTESIAN_POINT ( 'NONE',  ( -12.42445214995601077, 4.010151117816509903, 8.288741439567777647 ) ) ;
#7353 = ORIENTED_EDGE ( 'NONE', *, *, #10690, .T. ) ;
#7354 = ORIENTED_EDGE ( 'NONE', *, *, #30523, .F. ) ;
#7355 = VERTEX_POINT ( 'NONE', #16251 ) ;
#7356 = FACE_OUTER_BOUND ( 'NONE', #47162, .T. ) ;
#7357 = CARTESIAN_POINT ( 'NONE',  ( -11.14646393297422833, 0.000000000000000000, 3.625666556434874455 ) ) ;
#7358 = CARTESIAN_POINT ( 'NONE',  ( -31.72782227498118601, 0.000000000000000000, 9.205484770164058972 ) ) ;
#7359 = ADVANCED_FACE ( 'NONE', ( #55425 ), #6919, .F. ) ;
#7360 = EDGE_CURVE ( 'NONE', #50224, #21780, #33572, .T. ) ;
#7361 = AXIS2_PLACEMENT_3D ( 'NONE', #26935, #51898, #13017 ) ;
#7362 = VECTOR ( 'NONE', #14456, 999.9999999999998863 ) ;
#7363 = VERTEX_POINT ( 'NONE', #50879 ) ;
#7364 = ORIENTED_EDGE ( 'NONE', *, *, #52558, .F. ) ;
#7365 = EDGE_CURVE ( 'NONE', #54304, #17269, #46079, .T. ) ;
#7366 = CARTESIAN_POINT ( 'NONE',  ( -15.44653166369588781, 4.819660872929010687, 10.79116317270894143 ) ) ;
#7367 = CARTESIAN_POINT ( 'NONE',  ( -14.29221109521548883, 3.524445264749011208, 2.121063629962177011 ) ) ;
#7368 = EDGE_LOOP ( 'NONE', ( #18118, #24141, #31352, #32680 ) ) ;
#7369 = LINE ( 'NONE', #15083, #39132 ) ;
#7370 = ORIENTED_EDGE ( 'NONE', *, *, #36836, .T. ) ;
#7371 = PLANE ( 'NONE',  #30349 ) ;
#7372 = FACE_OUTER_BOUND ( 'NONE', #31373, .T. ) ;
#7373 = VERTEX_POINT ( 'NONE', #41266 ) ;
#7374 = PLANE ( 'NONE',  #1403 ) ;
#7375 = EDGE_CURVE ( 'NONE', #18842, #15384, #2358, .T. ) ;
#7376 = AXIS2_PLACEMENT_3D ( 'NONE', #44273, #26369, #9330 ) ;
#7377 = EDGE_CURVE ( 'NONE', #27029, #48144, #2627, .T. ) ;
#7378 = CARTESIAN_POINT ( 'NONE',  ( -17.46532115785441519, 0.000000000000000000, 13.67492996699914265 ) ) ;
#7379 = ORIENTED_EDGE ( 'NONE', *, *, #33779, .T. ) ;
#7380 = CARTESIAN_POINT ( 'NONE',  ( -11.35951049007415037, 0.000000000000000000, 5.301342914312717980 ) ) ;
#7381 = LINE ( 'NONE', #19328, #36646 ) ;
#7382 = EDGE_CURVE ( 'NONE', #20189, #28225, #54570, .T. ) ;
#7383 = PLANE ( 'NONE',  #175 ) ;
#7384 = ORIENTED_EDGE ( 'NONE', *, *, #21204, .T. ) ;
#7385 = EDGE_CURVE ( 'NONE', #2815, #47582, #41799, .T. ) ;
#7386 = PLANE ( 'NONE',  #49161 ) ;
#7387 = CARTESIAN_POINT ( 'NONE',  ( 2.072287782118878319, 0.000000000000000000, -2.950529333540147015 ) ) ;
#7388 = CARTESIAN_POINT ( 'NONE',  ( -11.88054826722768276, 25.79903810567671130, -3.000000000000000000 ) ) ;
#7389 = FACE_OUTER_BOUND ( 'NONE', #26945, .T. ) ;
#7390 = DIRECTION ( 'NONE',  ( -0.5449076811759708816, 0.6444004775717707689, 0.5364919789714475140 ) ) ;
#7391 = LINE ( 'NONE', #7689, #8933 ) ;
#7392 = LINE ( 'NONE', #21010, #2250 ) ;
#7393 = EDGE_LOOP ( 'NONE', ( #12076, #23199, #29751, #16167 ) ) ;
#7394 = CARTESIAN_POINT ( 'NONE',  ( -19.60912206198628027, -0.1191753592594197858, 4.398475361799976113 ) ) ;
#7395 = CARTESIAN_POINT ( 'NONE',  ( -27.99767448711536133, 0.000000000000000000, 7.557179307314289218 ) ) ;
#7396 = CARTESIAN_POINT ( 'NONE',  ( -14.56888064431065821, -0.1191753592594197858, 12.58947452739191064 ) ) ;
#7397 = ORIENTED_EDGE ( 'NONE', *, *, #4387, .T. ) ;
#7398 = LINE ( 'NONE', #33809, #35641 ) ;
#7399 = LINE ( 'NONE', #24719, #38154 ) ;
#7400 = AXIS2_PLACEMENT_3D ( 'NONE', #13513, #12672, #39649 ) ;
#7401 = VECTOR ( 'NONE', #46084, 1000.000000000000227 ) ;
#7402 = CARTESIAN_POINT ( 'NONE',  ( -11.13077601105853454, 0.000000000000000000, 1.609802280851077461 ) ) ;
#7403 = FACE_OUTER_BOUND ( 'NONE', #5446, .T. ) ;
#7404 = CARTESIAN_POINT ( 'NONE',  ( -16.75084723012008681, 0.000000000000000000, 7.275372647796405801 ) ) ;
#7405 = EDGE_LOOP ( 'NONE', ( #36180, #55034, #29758, #21340 ) ) ;
#7406 = VECTOR ( 'NONE', #21753, 999.9999999999998863 ) ;
#7407 = ORIENTED_EDGE ( 'NONE', *, *, #8870, .T. ) ;
#7408 = CARTESIAN_POINT ( 'NONE',  ( -16.92210063903004524, 0.000000000000000000, 3.580719216102757230 ) ) ;
#7409 = ADVANCED_FACE ( 'NONE', ( #4879 ), #21907, .F. ) ;
#7410 = DIRECTION ( 'NONE',  ( 0.000000000000000000, -0.000000000000000000, -1.000000000000000000 ) ) ;
#7411 = ORIENTED_EDGE ( 'NONE', *, *, #43525, .F. ) ;
#7412 = DIRECTION ( 'NONE',  ( 0.000000000000000000, -1.000000000000000000, 0.000000000000000000 ) ) ;
#7413 = VECTOR ( 'NONE', #41117, 1000.000000000000114 ) ;
#7414 = EDGE_CURVE ( 'NONE', #30062, #13266, #25345, .T. ) ;
#7415 = ORIENTED_EDGE ( 'NONE', *, *, #35188, .F. ) ;
#7416 = LINE ( 'NONE', #20770, #38372 ) ;
#7417 = VECTOR ( 'NONE', #47475, 1000.000000000000227 ) ;
#7418 = ORIENTED_EDGE ( 'NONE', *, *, #1814, .T. ) ;
#7419 = ORIENTED_EDGE ( 'NONE', *, *, #54953, .F. ) ;
#7420 = ORIENTED_EDGE ( 'NONE', *, *, #3998, .F. ) ;
#7421 = ADVANCED_FACE ( 'NONE', ( #13125 ), #21372, .F. ) ;
#7422 = CARTESIAN_POINT ( 'NONE',  ( -15.42322306907283114, -0.1191753592594189393, 2.953722716430651651 ) ) ;
#7423 = LINE ( 'NONE', #38093, #16879 ) ;
#7424 = DIRECTION ( 'NONE',  ( 0.6427681459581294776, -0.7660444431189769032, 0.005002170337467562802 ) ) ;
#7425 = EDGE_CURVE ( 'NONE', #42825, #37960, #3743, .T. ) ;
#7426 = EDGE_CURVE ( 'NONE', #2679, #41874, #51728, .T. ) ;
#7427 = EDGE_CURVE ( 'NONE', #9180, #41679, #30464, .T. ) ;
#7428 = FACE_OUTER_BOUND ( 'NONE', #49055, .T. ) ;
#7429 = ORIENTED_EDGE ( 'NONE', *, *, #19999, .F. ) ;
#7430 = EDGE_CURVE ( 'NONE', #40269, #6551, #323, .T. ) ;
#7431 = VERTEX_POINT ( 'NONE', #9134 ) ;
#7432 = ORIENTED_EDGE ( 'NONE', *, *, #24417, .F. ) ;
#7433 = CARTESIAN_POINT ( 'NONE',  ( -21.01797471916702165, 2.067327705546507133, 8.438253235298647681 ) ) ;
#7434 = DIRECTION ( 'NONE',  ( 0.007781995580012663651, -3.146120232559066537E-19, -0.9999697198139514409 ) ) ;
#7435 = ORIENTED_EDGE ( 'NONE', *, *, #7154, .F. ) ;
#7436 = CARTESIAN_POINT ( 'NONE',  ( -11.71475005485999077, -0.1191753592594185784, 4.090579120348019515 ) ) ;
#7437 = EDGE_LOOP ( 'NONE', ( #21125, #12984, #32146, #43957 ) ) ;
#7438 = CARTESIAN_POINT ( 'NONE',  ( -18.17847529190681044, 4.819660872929011575, 3.589296462945613886 ) ) ;
#7439 = LINE ( 'NONE', #45242, #22252 ) ;
#7440 = VECTOR ( 'NONE', #46835, 999.9999999999998863 ) ;
#7441 = VECTOR ( 'NONE', #49378, 1000.000000000000227 ) ;
#7442 = EDGE_LOOP ( 'NONE', ( #40895, #33270, #55616, #40434 ) ) ;
#7443 = DIRECTION ( 'NONE',  ( 0.000000000000000000, -1.000000000000000000, 0.000000000000000000 ) ) ;
#7444 = EDGE_CURVE ( 'NONE', #6825, #29855, #42683, .T. ) ;
#7445 = ORIENTED_EDGE ( 'NONE', *, *, #47699, .T. ) ;
#7446 = ADVANCED_FACE ( 'NONE', ( #26443 ), #47780, .F. ) ;
#7447 = VECTOR ( 'NONE', #33422, 1000.000000000000227 ) ;
#7448 = DIRECTION ( 'NONE',  ( -0.9999697198139514409, -0.000000000000000000, -0.007781995580013368816 ) ) ;
#7449 = DIRECTION ( 'NONE',  ( 0.007781995580012663651, 0.000000000000000000, -0.9999697198139515519 ) ) ;
#7450 = AXIS2_PLACEMENT_3D ( 'NONE', #13364, #34368, #12517 ) ;
#7451 = DIRECTION ( 'NONE',  ( 0.7660212471507180654, -0.6427876096865404731, 0.005961354470445141482 ) ) ;
#7452 = CARTESIAN_POINT ( 'NONE',  ( -20.54049170961573267, 0.000000000000000000, 4.660556269540326646 ) ) ;
#7453 = EDGE_CURVE ( 'NONE', #8966, #47897, #15484, .T. ) ;
#7454 = CARTESIAN_POINT ( 'NONE',  ( -10.27421835998572064, 0.000000000000000000, 10.96090226820206048 ) ) ;
#7455 = PLANE ( 'NONE',  #14673 ) ;
#7456 = EDGE_LOOP ( 'NONE', ( #7917, #29300, #14272, #3555 ) ) ;
#7458 = ORIENTED_EDGE ( 'NONE', *, *, #40840, .F. ) ;
#7457 = EDGE_CURVE ( 'NONE', #40214, #45690, #21655, .T. ) ;
#7459 = CARTESIAN_POINT ( 'NONE',  ( -21.47419595591918906, 0.000000000000000000, 5.222628093224860102 ) ) ;
#7460 = FACE_OUTER_BOUND ( 'NONE', #5498, .T. ) ;
#7461 = VECTOR ( 'NONE', #1860, 999.9999999999998863 ) ;
#7462 = CARTESIAN_POINT ( 'NONE',  ( -17.22985439448759237, 0.000000000000000000, 9.118305252317219001 ) ) ;
#7463 = LINE ( 'NONE', #32740, #8597 ) ;
#7464 = EDGE_CURVE ( 'NONE', #41663, #20135, #8293, .T. ) ;
#7465 = PLANE ( 'NONE',  #6184 ) ;
#7466 = LINE ( 'NONE', #3500, #34948 ) ;
#7467 = VERTEX_POINT ( 'NONE', #8589 ) ;
#7468 = DIRECTION ( 'NONE',  ( 0.005961354470445682716, -0.6427876096865404731, -0.7660212471507180654 ) ) ;
#7469 = PLANE ( 'NONE',  #51348 ) ;
#7470 = ORIENTED_EDGE ( 'NONE', *, *, #27277, .F. ) ;
#7471 = DIRECTION ( 'NONE',  ( 0.005961354470445682716, -0.6427876096865404731, -0.7660212471507180654 ) ) ;
#7472 = LINE ( 'NONE', #25103, #53088 ) ;
#7473 = ORIENTED_EDGE ( 'NONE', *, *, #52297, .T. ) ;
#7474 = CARTESIAN_POINT ( 'NONE',  ( -67.98273966911209243, -0.9999999999999978906, -3.909888324369924284 ) ) ;
#7475 = LINE ( 'NONE', #25106, #20589 ) ;
#7476 = LINE ( 'NONE', #33596, #55860 ) ;
#7477 = VECTOR ( 'NONE', #2089, 1000.000000000000227 ) ;
#7478 = PLANE ( 'NONE',  #46830 ) ;
#7479 = CARTESIAN_POINT ( 'NONE',  ( -67.50629308046563892, 1.999999999992078781, -2.738438791729908228 ) ) ;
#7480 = ORIENTED_EDGE ( 'NONE', *, *, #5733, .T. ) ;
#7481 = ORIENTED_EDGE ( 'NONE', *, *, #35313, .T. ) ;
#7482 = DIRECTION ( 'NONE',  ( 0.005002170337468016433, -0.7660444431189770143, -0.6427681459581293666 ) ) ;
#7483 = PLANE ( 'NONE',  #46708 ) ;
#7484 = AXIS2_PLACEMENT_3D ( 'NONE', #42138, #12026, #12342 ) ;
#7485 = DIRECTION ( 'NONE',  ( -0.005002170337468016433, -0.7660444431189770143, 0.6427681459581293666 ) ) ;
#7486 = VECTOR ( 'NONE', #4773, 1000.000000000000227 ) ;
#7487 = PLANE ( 'NONE',  #1416 ) ;
#7488 = VECTOR ( 'NONE', #11795, 999.9999999999998863 ) ;
#7489 = CARTESIAN_POINT ( 'NONE',  ( -13.08330893211609869, 0.000000000000000000, 1.763933231766363630 ) ) ;
#7490 = DIRECTION ( 'NONE',  ( 0.9999697198139515519, 0.000000000000000000, 0.007781995580013368816 ) ) ;
#7491 = ORIENTED_EDGE ( 'NONE', *, *, #5821, .T. ) ;
#7492 = DIRECTION ( 'NONE',  ( -0.3620778797217455991, 0.000000000000000000, -0.9321478471874540261 ) ) ;
#7493 = DIRECTION ( 'NONE',  ( 0.005961354470445682716, -0.6427876096865404731, -0.7660212471507180654 ) ) ;
#7494 = VECTOR ( 'NONE', #19925, 999.9999999999998863 ) ;
#7495 = DIRECTION ( 'NONE',  ( -0.5364919789714478471, 0.6444004775717705469, -0.5449076811759709926 ) ) ;
#7496 = AXIS2_PLACEMENT_3D ( 'NONE', #7266, #54149, #14674 ) ;
#7497 = VERTEX_POINT ( 'NONE', #43496 ) ;
#7498 = DIRECTION ( 'NONE',  ( 0.9999697198139515519, 0.000000000000000000, 0.007781995580013368816 ) ) ;
#7499 = DIRECTION ( 'NONE',  ( 1.000000000000000000, 0.000000000000000000, -8.673617379884027583E-16 ) ) ;
#7500 = PLANE ( 'NONE',  #15704 ) ;
#7501 = ADVANCED_FACE ( 'NONE', ( #42937 ), #52012, .F. ) ;
#7502 = EDGE_CURVE ( 'NONE', #11834, #45314, #52317, .T. ) ;
#7503 = ORIENTED_EDGE ( 'NONE', *, *, #2183, .T. ) ;
#7504 = PLANE ( 'NONE',  #39526 ) ;
#7505 = AXIS2_PLACEMENT_3D ( 'NONE', #8230, #17297, #42328 ) ;
#7506 = ORIENTED_EDGE ( 'NONE', *, *, #46260, .F. ) ;
#7507 = EDGE_CURVE ( 'NONE', #27679, #9163, #48036, .T. ) ;
#7508 = VECTOR ( 'NONE', #37838, 999.9999999999998863 ) ;
#7509 = ORIENTED_EDGE ( 'NONE', *, *, #49014, .F. ) ;
#7510 = ORIENTED_EDGE ( 'NONE', *, *, #13855, .F. ) ;
#7511 = ORIENTED_EDGE ( 'NONE', *, *, #34226, .T. ) ;
#7512 = CARTESIAN_POINT ( 'NONE',  ( -13.08486533123210194, 0.000000000000000000, 1.963927175729152541 ) ) ;
#7513 = VERTEX_POINT ( 'NONE', #12290 ) ;
#7514 = VECTOR ( 'NONE', #49850, 1000.000000000000227 ) ;
#7515 = ORIENTED_EDGE ( 'NONE', *, *, #42110, .T. ) ;
#7516 = CARTESIAN_POINT ( 'NONE',  ( -22.40634380310664397, 0.000000000000000000, 5.584705972946605534 ) ) ;
#7517 = ORIENTED_EDGE ( 'NONE', *, *, #46510, .T. ) ;
#7518 = VECTOR ( 'NONE', #5677, 999.9999999999998863 ) ;
#7519 = ORIENTED_EDGE ( 'NONE', *, *, #40515, .F. ) ;
#7520 = CARTESIAN_POINT ( 'NONE',  ( -10.56836678998424439, 0.000000000000000000, 7.323486140140572864 ) ) ;
#7521 = CARTESIAN_POINT ( 'NONE',  ( -10.94028622754223967, 0.000000000000000000, 11.14038480894692995 ) ) ;
#7522 = LINE ( 'NONE', #20862, #46820 ) ;
#7523 = PLANE ( 'NONE',  #50468 ) ;
#7524 = VECTOR ( 'NONE', #43472, 999.9999999999998863 ) ;
#7525 = DIRECTION ( 'NONE',  ( 0.9999697198139515519, 0.000000000000000000, 0.007781995580013368816 ) ) ;
#7526 = ORIENTED_EDGE ( 'NONE', *, *, #11910, .F. ) ;
#7527 = VECTOR ( 'NONE', #40759, 999.9999999999998863 ) ;
#7528 = AXIS2_PLACEMENT_3D ( 'NONE', #34635, #17060, #47729 ) ;
#7529 = EDGE_LOOP ( 'NONE', ( #31090, #10802, #55890, #6979, #10366 ) ) ;
#7530 = DIRECTION ( 'NONE',  ( -0.5449076811759708816, 0.6444004775717707689, 0.5364919789714475140 ) ) ;
#7531 = PLANE ( 'NONE',  #55672 ) ;
#7532 = EDGE_CURVE ( 'NONE', #16077, #9942, #29626, .T. ) ;
#7533 = DIRECTION ( 'NONE',  ( 0.5364919789714477361, 0.6444004775717706579, 0.5449076811759711036 ) ) ;
#7534 = AXIS2_PLACEMENT_3D ( 'NONE', #42436, #16041, #46685 ) ;
#7535 = VECTOR ( 'NONE', #4616, 1000.000000000000227 ) ;
#7536 = DIRECTION ( 'NONE',  ( 0.007781995580012663651, 0.000000000000000000, -0.9999697198139515519 ) ) ;
#7537 = EDGE_CURVE ( 'NONE', #16969, #38002, #55717, .T. ) ;
#7538 = DIRECTION ( 'NONE',  ( 0.000000000000000000, 1.000000000000000000, 0.000000000000000000 ) ) ;
#7539 = FACE_OUTER_BOUND ( 'NONE', #23124, .T. ) ;
#7540 = EDGE_LOOP ( 'NONE', ( #53400, #33002, #3843, #377 ) ) ;
#7541 = DIRECTION ( 'NONE',  ( 0.000000000000000000, 1.000000000000000000, 0.000000000000000000 ) ) ;
#7542 = CARTESIAN_POINT ( 'NONE',  ( -15.06067899816041944, 0.000000000000000000, 3.225873159917031607 ) ) ;
#7543 = EDGE_LOOP ( 'NONE', ( #50998, #44873, #55700, #45754 ) ) ;
#7544 = DIRECTION ( 'NONE',  ( 0.6427681459581294776, -0.7660444431189769032, 0.005002170337467562802 ) ) ;
#7545 = LINE ( 'NONE', #8124, #49580 ) ;
#7546 = LINE ( 'NONE', #33127, #37183 ) ;
#7547 = EDGE_CURVE ( 'NONE', #33592, #30111, #9414, .T. ) ;
#7548 = VECTOR ( 'NONE', #42318, 1000.000000000000227 ) ;
#7549 = CARTESIAN_POINT ( 'NONE',  ( -12.10890871433051430, 0.000000000000000000, 7.880835412697054565 ) ) ;
#7550 = VECTOR ( 'NONE', #9001, 1000.000000000000227 ) ;
#7551 = CARTESIAN_POINT ( 'NONE',  ( -19.51855023662962196, 0.000000000000000000, 4.668509254383998552 ) ) ;
#7552 = ORIENTED_EDGE ( 'NONE', *, *, #52997, .T. ) ;
#7553 = EDGE_LOOP ( 'NONE', ( #33492, #38053, #42759, #5303 ) ) ;
#7554 = PLANE ( 'NONE',  #32994 ) ;
#7555 = CARTESIAN_POINT ( 'NONE',  ( -20.53083501583961734, 20.80479272279814040, 4.322231945293713906 ) ) ;
#7556 = CARTESIAN_POINT ( 'NONE',  ( -26.24927669643210848, 17.48927842923457021, -4.622014950999592031 ) ) ;
#7557 = VECTOR ( 'NONE', #2968, 1000.000000000000227 ) ;
#7558 = CARTESIAN_POINT ( 'NONE',  ( -18.76354595665420177, -0.1191753592594177458, 14.21882498613976331 ) ) ;
#7559 = LINE ( 'NONE', #24886, #13100 ) ;
#7560 = VECTOR ( 'NONE', #42053, 1000.000000000000227 ) ;
#7561 = CARTESIAN_POINT ( 'NONE',  ( -13.00144731260268038, 25.15188674009506542, -3.504651694023052766 ) ) ;
#7562 = FACE_OUTER_BOUND ( 'NONE', #21457, .T. ) ;
#7563 = CARTESIAN_POINT ( 'NONE',  ( -68.57937869370883277, -9.558884488700273963, 7.875383342262417763 ) ) ;
#7564 = VECTOR ( 'NONE', #31622, 1000.000000000000227 ) ;
#7565 = LINE ( 'NONE', #24896, #40125 ) ;
#7566 = ORIENTED_EDGE ( 'NONE', *, *, #38628, .T. ) ;
#7567 = DIRECTION ( 'NONE',  ( -0.9335804264972042965, 0.3583679495452938291, -0.000000000000000000 ) ) ;
#7568 = VECTOR ( 'NONE', #55167, 999.9999999999998863 ) ;
#7569 = AXIS2_PLACEMENT_3D ( 'NONE', #9032, #13008, #30634 ) ;
#7570 = EDGE_CURVE ( 'NONE', #47896, #33244, #18800, .T. ) ;
#7571 = ORIENTED_EDGE ( 'NONE', *, *, #2961, .T. ) ;
#7572 = ADVANCED_FACE ( 'NONE', ( #40652 ), #19049, .F. ) ;
#7573 = ADVANCED_FACE ( 'NONE', ( #53681 ), #40070, .F. ) ;
#7574 = VECTOR ( 'NONE', #36102, 1000.000000000000114 ) ;
#7575 = ORIENTED_EDGE ( 'NONE', *, *, #52634, .T. ) ;
#7576 = ORIENTED_EDGE ( 'NONE', *, *, #21982, .F. ) ;
#7577 = VECTOR ( 'NONE', #40866, 1000.000000000000114 ) ;
#7578 = EDGE_LOOP ( 'NONE', ( #7010, #33690, #55851, #53161 ) ) ;
#7579 = VERTEX_POINT ( 'NONE', #5719 ) ;
#7580 = CARTESIAN_POINT ( 'NONE',  ( -17.83139810946674686, -0.1191753592594197858, 13.85674710641801788 ) ) ;
#7581 = CARTESIAN_POINT ( 'NONE',  ( -13.23949410636475399, 0.000000000000000000, 8.041362949340008726 ) ) ;
#7582 = FACE_OUTER_BOUND ( 'NONE', #14446, .T. ) ;
#7583 = ORIENTED_EDGE ( 'NONE', *, *, #6950, .T. ) ;
#7584 = CARTESIAN_POINT ( 'NONE',  ( -9.040517713763286167, 0.000000000000000000, 5.858047935705506859 ) ) ;
#7585 = VERTEX_POINT ( 'NONE', #10566 ) ;
#7586 = CARTESIAN_POINT ( 'NONE',  ( -65.31549755956690717, -11.19770874131334182, 4.495433075559887470 ) ) ;
#7587 = ORIENTED_EDGE ( 'NONE', *, *, #37225, .T. ) ;
#7588 = EDGE_CURVE ( 'NONE', #53603, #53756, #36372, .T. ) ;
#7589 = CARTESIAN_POINT ( 'NONE',  ( -65.92002855750158119, -9.253925629004317699, -0.7138195548257249001 ) ) ;
#7590 = AXIS2_PLACEMENT_3D ( 'NONE', #8285, #25599, #12827 ) ;
#7591 = CARTESIAN_POINT ( 'NONE',  ( -13.08486533123210194, 0.000000000000000000, 1.963927175729152541 ) ) ;
#7592 = CARTESIAN_POINT ( 'NONE',  ( -24.96676581047183063, 18.24370688441070953, -4.565775476651154463 ) ) ;
#7593 = ORIENTED_EDGE ( 'NONE', *, *, #40873, .T. ) ;
#7594 = DIRECTION ( 'NONE',  ( 0.5449076811759707706, 0.6444004775717708799, -0.5364919789714476250 ) ) ;
#7595 = VECTOR ( 'NONE', #4743, 999.9999999999998863 ) ;
#7596 = ORIENTED_EDGE ( 'NONE', *, *, #37646, .T. ) ;
#7597 = DIRECTION ( 'NONE',  ( 0.5364919789714477361, 0.6444004775717706579, 0.5449076811759711036 ) ) ;
#7599 = VECTOR ( 'NONE', #46488, 1000.000000000000114 ) ;
#7598 = DIRECTION ( 'NONE',  ( -0.5364919789714478471, 0.6444004775717705469, -0.5449076811759709926 ) ) ;
#7600 = DIRECTION ( 'NONE',  ( 0.5449076811759707706, 0.6444004775717708799, -0.5364919789714476250 ) ) ;
#7601 = FACE_OUTER_BOUND ( 'NONE', #54326, .T. ) ;
#7602 = DIRECTION ( 'NONE',  ( -0.05705673239519651330, 0.9983709377222391712, 2.351258244848514932E-16 ) ) ;
#7603 = LINE ( 'NONE', #47071, #44822 ) ;
#7604 = CARTESIAN_POINT ( 'NONE',  ( -23.44005680416443838, 18.93270265044663603, 4.490773887887535842 ) ) ;
#7605 = AXIS2_PLACEMENT_3D ( 'NONE', #50017, #45229, #28171 ) ;
#7606 = CARTESIAN_POINT ( 'NONE',  ( -30.79567442779373110, 0.000000000000000000, 8.843406890442315316 ) ) ;
#7607 = VERTEX_POINT ( 'NONE', #39807 ) ;
#7608 = LINE ( 'NONE', #46491, #52800 ) ;
#7609 = ORIENTED_EDGE ( 'NONE', *, *, #3116, .T. ) ;
#7610 = AXIS2_PLACEMENT_3D ( 'NONE', #20739, #21595, #8231 ) ;
#7611 = DIRECTION ( 'NONE',  ( -0.7660212471507179544, -0.6427876096865405842, -0.005961354470445141482 ) ) ;
#7612 = FACE_OUTER_BOUND ( 'NONE', #54522, .T. ) ;
#7613 = CARTESIAN_POINT ( 'NONE',  ( -8.380637751107304467, 0.000000000000000000, 6.473697885849892586 ) ) ;
#7614 = EDGE_CURVE ( 'NONE', #7363, #39093, #36121, .T. ) ;
#7615 = CARTESIAN_POINT ( 'NONE',  ( -20.44938042942779433, 0.000000000000000000, 4.861271374810767654 ) ) ;
#7616 = DIRECTION ( 'NONE',  ( 0.000000000000000000, -1.000000000000000000, 0.000000000000000000 ) ) ;
#7617 = AXIS2_PLACEMENT_3D ( 'NONE', #51632, #26097, #20702 ) ;
#7618 = CARTESIAN_POINT ( 'NONE',  ( -17.59819193477204990, 0.000000000000000000, 10.05410896024298140 ) ) ;
#7619 = VECTOR ( 'NONE', #15502, 999.9999999999998863 ) ;
#7620 = CARTESIAN_POINT ( 'NONE',  ( 0.000000000000000000, 0.000000000000000000, 0.000000000000000000 ) ) ;
#7621 = ORIENTED_EDGE ( 'NONE', *, *, #38261, .T. ) ;
#7622 = DIRECTION ( 'NONE',  ( 0.9999697198139515519, 0.000000000000000000, 0.007781995580013368816 ) ) ;
#7623 = DIRECTION ( 'NONE',  ( 0.007781995580012663651, 0.000000000000000000, -0.9999697198139515519 ) ) ;
#7624 = DIRECTION ( 'NONE',  ( 0.005961354470445682716, -0.6427876096865404731, -0.7660212471507180654 ) ) ;
#7625 = CARTESIAN_POINT ( 'NONE',  ( -13.66524968089654379, -5.698858183938163791, 11.34277594356301222 ) ) ;
#7626 = EDGE_CURVE ( 'NONE', #51521, #3481, #884, .T. ) ;
#7627 = CARTESIAN_POINT ( 'NONE',  ( -17.36532418587302473, -0.1191753592594177458, 13.67570816655714516 ) ) ;
#7628 = CARTESIAN_POINT ( 'NONE',  ( -27.99767448711536133, 0.000000000000000000, 7.557179307314289218 ) ) ;
#7629 = EDGE_CURVE ( 'NONE', #33817, #48888, #14799, .T. ) ;
#7630 = LINE ( 'NONE', #7093, #25115 ) ;
#7631 = ADVANCED_FACE ( 'NONE', ( #30982 ), #10256, .F. ) ;
#7632 = LINE ( 'NONE', #25249, #50076 ) ;
#7633 = ORIENTED_EDGE ( 'NONE', *, *, #39599, .F. ) ;
#7634 = VECTOR ( 'NONE', #2690, 1000.000000000000227 ) ;
#7635 = DIRECTION ( 'NONE',  ( -0.1139275668495183386, 0.9934890585767658377, 4.694855797473113547E-16 ) ) ;
#7636 = DIRECTION ( 'NONE',  ( -0.005961354470445682716, -0.6427876096865404731, 0.7660212471507180654 ) ) ;
#7637 = VERTEX_POINT ( 'NONE', #44903 ) ;
#7638 = AXIS2_PLACEMENT_3D ( 'NONE', #34408, #55698, #47764 ) ;
#7639 = ORIENTED_EDGE ( 'NONE', *, *, #46679, .T. ) ;
#7640 = CARTESIAN_POINT ( 'NONE',  ( -15.56136093618090044, 0.000000000000000000, 7.853967631204984201 ) ) ;
#7641 = EDGE_CURVE ( 'NONE', #49508, #20663, #32123, .T. ) ;
#7642 = VECTOR ( 'NONE', #20020, 1000.000000000000227 ) ;
#7643 = VERTEX_POINT ( 'NONE', #35833 ) ;
#7644 = ADVANCED_FACE ( 'NONE', ( #44339 ), #53159, .F. ) ;
#7645 = VECTOR ( 'NONE', #38833, 999.9999999999998863 ) ;
#7646 = ORIENTED_EDGE ( 'NONE', *, *, #51174, .F. ) ;
#7647 = LINE ( 'NONE', #7106, #14789 ) ;
#7648 = EDGE_CURVE ( 'NONE', #8596, #2376, #23590, .T. ) ;
#7649 = ORIENTED_EDGE ( 'NONE', *, *, #672, .T. ) ;
#7650 = ORIENTED_EDGE ( 'NONE', *, *, #33647, .T. ) ;
#7651 = ORIENTED_EDGE ( 'NONE', *, *, #13029, .T. ) ;
#7652 = DIRECTION ( 'NONE',  ( -0.6427681459581293666, -0.7660444431189770143, -0.005002170337467561935 ) ) ;
#7653 = AXIS2_PLACEMENT_3D ( 'NONE', #19806, #36043, #2192 ) ;
#7654 = CARTESIAN_POINT ( 'NONE',  ( -66.04895207021591830, -9.268709830190596577, 5.126821739293232483 ) ) ;
#7655 = FACE_OUTER_BOUND ( 'NONE', #47512, .T. ) ;
#7656 = AXIS2_PLACEMENT_3D ( 'NONE', #48173, #4749, #45259 ) ;
#7657 = EDGE_CURVE ( 'NONE', #25423, #39170, #9723, .T. ) ;
#7658 = ORIENTED_EDGE ( 'NONE', *, *, #36965, .F. ) ;
#7659 = VERTEX_POINT ( 'NONE', #14520 ) ;
#7660 = ADVANCED_FACE ( 'NONE', ( #44065 ), #22496, .F. ) ;
#7661 = AXIS2_PLACEMENT_3D ( 'NONE', #29985, #8134, #30272 ) ;
#7662 = AXIS2_PLACEMENT_3D ( 'NONE', #211, #34889, #25251 ) ;
#7663 = FACE_OUTER_BOUND ( 'NONE', #11897, .T. ) ;
#7664 = CARTESIAN_POINT ( 'NONE',  ( -17.69449129132867071, 0.000000000000000000, 9.114689340549208652 ) ) ;
#7665 = ORIENTED_EDGE ( 'NONE', *, *, #27272, .T. ) ;
#7666 = DIRECTION ( 'NONE',  ( 0.7660212471507180654, -0.6427876096865404731, 0.005961354470445141482 ) ) ;
#7667 = ORIENTED_EDGE ( 'NONE', *, *, #42333, .F. ) ;
#7668 = DIRECTION ( 'NONE',  ( 0.7660212471507180654, -0.6427876096865404731, 0.005961354470445141482 ) ) ;
#7669 = DIRECTION ( 'NONE',  ( 0.007781995580012662783, 0.000000000000000000, -0.9999697198139514409 ) ) ;
#7670 = EDGE_LOOP ( 'NONE', ( #24439, #34011, #46905, #16126 ) ) ;
#7671 = CARTESIAN_POINT ( 'NONE',  ( -18.67619601524082285, 0.000000000000000000, 3.936400510096834893 ) ) ;
#7672 = VECTOR ( 'NONE', #11616, 999.9999999999998863 ) ;
#7673 = PLANE ( 'NONE',  #1862 ) ;
#7674 = ORIENTED_EDGE ( 'NONE', *, *, #18968, .F. ) ;
#7675 = CARTESIAN_POINT ( 'NONE',  ( 2.072287782118878319, 0.000000000000000000, -2.950529333540147015 ) ) ;
#7676 = DIRECTION ( 'NONE',  ( 0.005961354470445682716, -0.6427876096865404731, -0.7660212471507180654 ) ) ;
#7678 = AXIS2_PLACEMENT_3D ( 'NONE', #44896, #18196, #49142 ) ;
#7677 = DIRECTION ( 'NONE',  ( 0.000000000000000000, 0.000000000000000000, 1.000000000000000000 ) ) ;
#7679 = LINE ( 'NONE', #11379, #12888 ) ;
#7680 = ORIENTED_EDGE ( 'NONE', *, *, #35511, .F. ) ;
#7681 = AXIS2_PLACEMENT_3D ( 'NONE', #25854, #33795, #47415 ) ;
#7682 = DIRECTION ( 'NONE',  ( 0.5364919789714477361, 0.6444004775717706579, 0.5449076811759711036 ) ) ;
#7683 = CARTESIAN_POINT ( 'NONE',  ( 2.072287782118878319, 0.000000000000000000, -2.950529333540147015 ) ) ;
#7684 = CARTESIAN_POINT ( 'NONE',  ( -55.47117325737978888, 6.581829179614757663, -1.080525476705088916 ) ) ;
#7685 = ADVANCED_FACE ( 'NONE', ( #27031 ), #48887, .F. ) ;
#7686 = AXIS2_PLACEMENT_3D ( 'NONE', #49725, #45721, #28975 ) ;
#7687 = DIRECTION ( 'NONE',  ( 0.007781995580012662783, 0.000000000000000000, -0.9999697198139514409 ) ) ;
#7688 = DIRECTION ( 'NONE',  ( -0.005002170337468016433, -0.7660444431189770143, 0.6427681459581293666 ) ) ;
#7689 = CARTESIAN_POINT ( 'NONE',  ( -14.94916102560700821, 0.000000000000000000, 2.688082935172642962 ) ) ;
#7690 = CARTESIAN_POINT ( 'NONE',  ( -10.94028622754223967, 0.000000000000000000, 11.14038480894692995 ) ) ;
#7691 = AXIS2_PLACEMENT_3D ( 'NONE', #33586, #38411, #33038 ) ;
#7692 = ORIENTED_EDGE ( 'NONE', *, *, #43761, .T. ) ;
#7693 = FACE_OUTER_BOUND ( 'NONE', #7437, .T. ) ;
#7694 = DIRECTION ( 'NONE',  ( 0.6427681459581294776, -0.7660444431189769032, 0.005002170337467562802 ) ) ;
#7695 = ORIENTED_EDGE ( 'NONE', *, *, #31514, .T. ) ;
#7696 = VECTOR ( 'NONE', #4030, 999.9999999999998863 ) ;
#7697 = FACE_OUTER_BOUND ( 'NONE', #11247, .T. ) ;
#7698 = LINE ( 'NONE', #25030, #20918 ) ;
#7699 = VECTOR ( 'NONE', #45450, 1000.000000000000227 ) ;
#7700 = CARTESIAN_POINT ( 'NONE',  ( -26.13337879274045505, 0.000000000000000000, 6.833023547870798353 ) ) ;
#7701 = FACE_OUTER_BOUND ( 'NONE', #21765, .T. ) ;
#7702 = ADVANCED_FACE ( 'NONE', ( #23336 ), #2566, .F. ) ;
#7703 = DIRECTION ( 'NONE',  ( 0.007781995580012663651, -3.146120232559066537E-19, -0.9999697198139514409 ) ) ;
#7704 = ORIENTED_EDGE ( 'NONE', *, *, #18037, .F. ) ;
#7705 = AXIS2_PLACEMENT_3D ( 'NONE', #41837, #2935, #20268 ) ;
#7706 = VECTOR ( 'NONE', #37652, 999.9999999999998863 ) ;
#7707 = VERTEX_POINT ( 'NONE', #15352 ) ;
#7708 = CARTESIAN_POINT ( 'NONE',  ( -13.17065887352947762, -0.1191753592594197858, 12.04635770780929427 ) ) ;
#7709 = FACE_OUTER_BOUND ( 'NONE', #40577, .T. ) ;
#7710 = CARTESIAN_POINT ( 'NONE',  ( -18.81253076747439223, -3.594132820645663084, 4.074075289172853331 ) ) ;
#7711 = EDGE_LOOP ( 'NONE', ( #22797, #30837, #889, #7566 ) ) ;
#7712 = ADVANCED_FACE ( 'NONE', ( #19886 ), #7673, .F. ) ;
#7713 = CARTESIAN_POINT ( 'NONE',  ( -17.74404816805336793, 0.000000000000000000, 3.574322630375089460 ) ) ;
#7714 = ORIENTED_EDGE ( 'NONE', *, *, #11910, .T. ) ;
#7715 = DIRECTION ( 'NONE',  ( 0.007781995580012663651, -3.146120232559066537E-19, -0.9999697198139514409 ) ) ;
#7716 = EDGE_CURVE ( 'NONE', #46161, #28907, #50561, .T. ) ;
#7717 = VECTOR ( 'NONE', #8978, 999.9999999999998863 ) ;
#7718 = EDGE_LOOP ( 'NONE', ( #33667, #41199, #24264, #44118 ) ) ;
#7719 = EDGE_LOOP ( 'NONE', ( #11119, #23968, #39269, #22805 ) ) ;
#7720 = VERTEX_POINT ( 'NONE', #42324 ) ;
#7721 = VECTOR ( 'NONE', #45055, 999.9999999999998863 ) ;
#7722 = CARTESIAN_POINT ( 'NONE',  ( -18.11943520534269680, 3.038739411681508518, 8.906614157015832589 ) ) ;
#7723 = FACE_OUTER_BOUND ( 'NONE', #44067, .T. ) ;
#7724 = CARTESIAN_POINT ( 'NONE',  ( -16.06709938707323460, 0.000000000000000000, 13.13181314741652628 ) ) ;
#7725 = EDGE_CURVE ( 'NONE', #26525, #35209, #11658, .T. ) ;
#7726 = CARTESIAN_POINT ( 'NONE',  ( -18.96745105697236156, 0.7721120973665048792, 4.024899441011595691 ) ) ;
#7727 = VECTOR ( 'NONE', #36524, 1000.000000000000000 ) ;
#7728 = ORIENTED_EDGE ( 'NONE', *, *, #40811, .T. ) ;
#7729 = B_SPLINE_CURVE_WITH_KNOTS ( 'NONE', 3,
 ( #49222, #10335, #27661, #44987 ),
 .UNSPECIFIED., .F., .F.,
 ( 4, 4 ),
 ( 0.7012410636449952772, 0.7288427234739881522 ),
 .UNSPECIFIED. ) ;
#7730 = ORIENTED_EDGE ( 'NONE', *, *, #51861, .T. ) ;
#7731 = ADVANCED_FACE ( 'NONE', ( #32421 ), #2823, .F. ) ;
#7732 = ORIENTED_EDGE ( 'NONE', *, *, #44454, .T. ) ;
#7733 = VECTOR ( 'NONE', #23393, 1000.000000000000114 ) ;
#7734 = DIRECTION ( 'NONE',  ( 0.000000000000000000, -1.000000000000000000, 0.000000000000000000 ) ) ;
#7735 = AXIS2_PLACEMENT_3D ( 'NONE', #11713, #33315, #15406 ) ;
#7736 = CARTESIAN_POINT ( 'NONE',  ( -11.77243710274829525, -0.1191753592594197858, 11.50324088822667612 ) ) ;
#7737 = EDGE_LOOP ( 'NONE', ( #38684, #20971, #32519, #32847 ) ) ;
#7738 = VECTOR ( 'NONE', #40931, 1000.000000000000227 ) ;
#7739 = CARTESIAN_POINT ( 'NONE',  ( 2.072287782118878319, 0.000000000000000000, -2.950529333540147015 ) ) ;
#7740 = ORIENTED_EDGE ( 'NONE', *, *, #1289, .T. ) ;
#7741 = CARTESIAN_POINT ( 'NONE',  ( -14.66887761629205222, 0.000000000000000000, 12.58869632783390990 ) ) ;
#7742 = PLANE ( 'NONE',  #414 ) ;
#7743 = AXIS2_PLACEMENT_3D ( 'NONE', #52469, #49869, #45085 ) ;
#7744 = ORIENTED_EDGE ( 'NONE', *, *, #11158, .T. ) ;
#7745 = VECTOR ( 'NONE', #21506, 1000.000000000000114 ) ;
#7746 = DIRECTION ( 'NONE',  ( 0.000000000000000000, -1.000000000000000000, 0.000000000000000000 ) ) ;
#7747 = ORIENTED_EDGE ( 'NONE', *, *, #10751, .T. ) ;
#7748 = AXIS2_PLACEMENT_3D ( 'NONE', #50595, #7412, #34398 ) ;
#7749 = DIRECTION ( 'NONE',  ( 0.005961354470445682716, -0.6427876096865404731, -0.7660212471507180654 ) ) ;
#7750 = AXIS2_PLACEMENT_3D ( 'NONE', #20240, #50055, #46094 ) ;
#7751 = LINE ( 'NONE', #21374, #48326 ) ;
#7752 = ORIENTED_EDGE ( 'NONE', *, *, #40941, .F. ) ;
#7753 = CARTESIAN_POINT ( 'NONE',  ( -57.29829478218162109, -10.27834239552269757, 4.211285351864063224E-15 ) ) ;
#7754 = DIRECTION ( 'NONE',  ( -0.5449076811759708816, 0.6444004775717707689, 0.5364919789714475140 ) ) ;
#7755 = LINE ( 'NONE', #51182, #45924 ) ;
#7756 = CARTESIAN_POINT ( 'NONE',  ( -14.94760462649100496, 0.000000000000000000, 2.488088991209854051 ) ) ;
#7757 = ORIENTED_EDGE ( 'NONE', *, *, #30304, .F. ) ;
#7758 = EDGE_CURVE ( 'NONE', #47771, #2654, #29240, .T. ) ;
#7759 = VERTEX_POINT ( 'NONE', #36957 ) ;
#7760 = DIRECTION ( 'NONE',  ( 0.007781995580012663651, 0.000000000000000000, -0.9999697198139515519 ) ) ;
#7761 = DIRECTION ( 'NONE',  ( 0.007781995580012663651, 0.000000000000000000, -0.9999697198139515519 ) ) ;
#7762 = ADVANCED_FACE ( 'NONE', ( #24167 ), #15608, .T. ) ;
#7763 = LINE ( 'NONE', #1616, #38578 ) ;
#7764 = LINE ( 'NONE', #16265, #55727 ) ;
#7765 = CARTESIAN_POINT ( 'NONE',  ( -8.860905869600903983, 1.712176620043476140E-14, 3.600000000000000089 ) ) ;
#7766 = VECTOR ( 'NONE', #28159, 1000.000000000000227 ) ;
#7767 = ADVANCED_FACE ( 'NONE', ( #6843 ), #37793, .F. ) ;
#7768 = LINE ( 'NONE', #50639, #47624 ) ;
#7769 = ORIENTED_EDGE ( 'NONE', *, *, #12847, .T. ) ;
#7770 = AXIS2_PLACEMENT_3D ( 'NONE', #55488, #8359, #16594 ) ;
#7771 = EDGE_CURVE ( 'NONE', #20993, #235, #46558, .T. ) ;
#7772 = CARTESIAN_POINT ( 'NONE',  ( -12.81375377831746221, -1.975113310420657520, 4.900726287218082788 ) ) ;
#7773 = CARTESIAN_POINT ( 'NONE',  ( -17.26532721389163072, 0.000000000000000000, 13.67648636611514590 ) ) ;
#7774 = ORIENTED_EDGE ( 'NONE', *, *, #47717, .F. ) ;
#7775 = FACE_OUTER_BOUND ( 'NONE', #46896, .T. ) ;
#7776 = VECTOR ( 'NONE', #30622, 1000.000000000000114 ) ;
#7777 = VERTEX_POINT ( 'NONE', #32950 ) ;
#7778 = EDGE_CURVE ( 'NONE', #49949, #29930, #20147, .T. ) ;
#7779 = EDGE_CURVE ( 'NONE', #10997, #2403, #53973, .T. ) ;
#7780 = ADVANCED_FACE ( 'NONE', ( #28708 ), #11915, .F. ) ;
#7781 = FACE_OUTER_BOUND ( 'NONE', #12588, .T. ) ;
#7782 = DIRECTION ( 'NONE',  ( -0.5449076811759708816, 0.6444004775717707689, 0.5364919789714475140 ) ) ;
#7783 = AXIS2_PLACEMENT_3D ( 'NONE', #21602, #25857, #51421 ) ;
#7784 = CARTESIAN_POINT ( 'NONE',  ( -18.66354898467281132, 0.000000000000000000, 14.21960318569776582 ) ) ;
#7785 = CARTESIAN_POINT ( 'NONE',  ( -18.60232905608458509, 0.000000000000000000, 6.352973834913863804 ) ) ;
#7786 = CARTESIAN_POINT ( 'NONE',  ( -65.68175713575769237, 2.000000000000022204, -3.167379070712565969 ) ) ;
#7787 = ORIENTED_EDGE ( 'NONE', *, *, #9792, .T. ) ;
#7788 = AXIS2_PLACEMENT_3D ( 'NONE', #42387, #7443, #37550 ) ;
#7789 = AXIS2_PLACEMENT_3D ( 'NONE', #16302, #12036, #33371 ) ;
#7790 = ORIENTED_EDGE ( 'NONE', *, *, #54811, .T. ) ;
#7791 = DIRECTION ( 'NONE',  ( -0.005961354470445682716, -0.6427876096865404731, 0.7660212471507180654 ) ) ;
#7792 = DIRECTION ( 'NONE',  ( -0.6427681459581293666, -0.7660444431189770143, -0.005002170337467561935 ) ) ;
#7793 = PLANE ( 'NONE',  #35075 ) ;
#7794 = VECTOR ( 'NONE', #30262, 1000.000000000000000 ) ;
#7795 = CARTESIAN_POINT ( 'NONE',  ( -27.06552663992790997, 0.000000000000000000, 7.195101427592543786 ) ) ;
#7797 = LINE ( 'NONE', #25122, #23775 ) ;
#7796 = AXIS2_PLACEMENT_3D ( 'NONE', #39683, #31137, #39935 ) ;
#7798 = ADVANCED_FACE ( 'NONE', ( #7124 ), #15095, .F. ) ;
#7799 = LINE ( 'NONE', #38150, #38506 ) ;
#7800 = VECTOR ( 'NONE', #29068, 1000.000000000000000 ) ;
#7801 = ORIENTED_EDGE ( 'NONE', *, *, #38870, .T. ) ;
#7802 = DIRECTION ( 'NONE',  ( 0.007781995580012662783, 0.000000000000000000, -0.9999697198139514409 ) ) ;
#7803 = AXIS2_PLACEMENT_3D ( 'NONE', #28525, #15211, #36789 ) ;
#7804 = EDGE_CURVE ( 'NONE', #37945, #12623, #3118, .T. ) ;
#7805 = CARTESIAN_POINT ( 'NONE',  ( 2.072287782118878319, 0.000000000000000000, -2.950529333540147015 ) ) ;
#7806 = VECTOR ( 'NONE', #38858, 1000.000000000000227 ) ;
#7807 = PLANE ( 'NONE',  #5191 ) ;
#7808 = ORIENTED_EDGE ( 'NONE', *, *, #10634, .T. ) ;
#7809 = ADVANCED_FACE ( 'NONE', ( #6550 ), #2286, .F. ) ;
#7810 = DIRECTION ( 'NONE',  ( 0.5449076811759707706, 0.6444004775717708799, -0.5364919789714476250 ) ) ;
#7811 = PLANE ( 'NONE',  #45844 ) ;
#7812 = CARTESIAN_POINT ( 'NONE',  ( -17.39979014900826471, 0.000000000000000000, 5.254336061328594987 ) ) ;
#7813 = ORIENTED_EDGE ( 'NONE', *, *, #2738, .T. ) ;
#7814 = EDGE_CURVE ( 'NONE', #2673, #43270, #43171, .T. ) ;
#7815 = LINE ( 'NONE', #8934, #32002 ) ;
#7816 = ORIENTED_EDGE ( 'NONE', *, *, #4425, .T. ) ;
#7817 = VECTOR ( 'NONE', #36222, 1000.000000000000227 ) ;
#7818 = ORIENTED_EDGE ( 'NONE', *, *, #8788, .T. ) ;
#7819 = VERTEX_POINT ( 'NONE', #21839 ) ;
#7820 = VERTEX_POINT ( 'NONE', #30090 ) ;
#7821 = DIRECTION ( 'NONE',  ( 0.005961354470445682716, -0.6427876096865404731, -0.7660212471507180654 ) ) ;
#7822 = VECTOR ( 'NONE', #38724, 999.9999999999998863 ) ;
#7823 = ORIENTED_EDGE ( 'NONE', *, *, #35611, .T. ) ;
#7824 = FACE_OUTER_BOUND ( 'NONE', #38120, .T. ) ;
#7825 = VERTEX_POINT ( 'NONE', #51664 ) ;
#7826 = CARTESIAN_POINT ( 'NONE',  ( -19.70461351680143736, -0.03744543421978414194, 6.914475087243958207 ) ) ;
#7827 = ORIENTED_EDGE ( 'NONE', *, *, #17886, .F. ) ;
#7828 = VECTOR ( 'NONE', #20943, 1000.000000000000227 ) ;
#7829 = VERTEX_POINT ( 'NONE', #51935 ) ;
#7830 = VECTOR ( 'NONE', #8833, 1000.000000000000227 ) ;
#7831 = AXIS2_PLACEMENT_3D ( 'NONE', #23401, #44403, #31061 ) ;
#7832 = CARTESIAN_POINT ( 'NONE',  ( -19.42910703681909368, 21.15220053346460816, 4.255330291687501543 ) ) ;
#7833 = DIRECTION ( 'NONE',  ( -0.3620778797217455991, 0.000000000000000000, -0.9321478471874540261 ) ) ;
#7834 = CARTESIAN_POINT ( 'NONE',  ( -13.73672976910459909, 0.000000000000000000, 12.22661844811216270 ) ) ;
#7835 = DIRECTION ( 'NONE',  ( -0.005002170337468016433, -0.7660444431189770143, 0.6427681459581293666 ) ) ;
#7836 = PLANE ( 'NONE',  #45558 ) ;
#7837 = ORIENTED_EDGE ( 'NONE', *, *, #18861, .F. ) ;
#7838 = AXIS2_PLACEMENT_3D ( 'NONE', #54130, #53553, #14118 ) ;
#7839 = ORIENTED_EDGE ( 'NONE', *, *, #35281, .T. ) ;
#7840 = AXIS2_PLACEMENT_3D ( 'NONE', #28193, #10641, #45250 ) ;
#7841 = FACE_OUTER_BOUND ( 'NONE', #31554, .T. ) ;
#7842 = CARTESIAN_POINT ( 'NONE',  ( -17.19823980592947876, 0.000000000000000000, 5.055898516481810212 ) ) ;
#7843 = AXIS2_PLACEMENT_3D ( 'NONE', #4022, #2869, #37533 ) ;
#7844 = LINE ( 'NONE', #33649, #1590 ) ;
#7845 = VECTOR ( 'NONE', #18233, 999.9999999999998863 ) ;
#7846 = LINE ( 'NONE', #17182, #55856 ) ;
#7847 = PLANE ( 'NONE',  #25879 ) ;
#7848 = DIRECTION ( 'NONE',  ( -0.005961354470445682716, -0.6427876096865404731, 0.7660212471507180654 ) ) ;
#7849 = ORIENTED_EDGE ( 'NONE', *, *, #54878, .T. ) ;
#7850 = LINE ( 'NONE', #25706, #19318 ) ;
#7851 = DIRECTION ( 'NONE',  ( 0.007781995580012663651, 0.000000000000000000, -0.9999697198139515519 ) ) ;
#7852 = ORIENTED_EDGE ( 'NONE', *, *, #43049, .T. ) ;
#7853 = EDGE_CURVE ( 'NONE', #36877, #54764, #25283, .T. ) ;
#7854 = EDGE_CURVE ( 'NONE', #29009, #13585, #42587, .T. ) ;
#7855 = CARTESIAN_POINT ( 'NONE',  ( -18.67697421479882181, -0.1191753592594197858, 4.036397482078229793 ) ) ;
#7856 = DIRECTION ( 'NONE',  ( -0.6427681459581293666, -0.7660444431189770143, -0.005002170337467561935 ) ) ;
#7857 = CARTESIAN_POINT ( 'NONE',  ( -18.39746900504187010, 0.000000000000000000, 14.03700784672088808 ) ) ;
#7858 = LINE ( 'NONE', #3572, #4187 ) ;
#7859 = EDGE_CURVE ( 'NONE', #33225, #14263, #34089, .T. ) ;
#7860 = DIRECTION ( 'NONE',  ( -0.9999697198139514409, -0.000000000000000000, -0.007781995580013368816 ) ) ;
#7861 = VECTOR ( 'NONE', #24821, 1000.000000000000227 ) ;
#7862 = ORIENTED_EDGE ( 'NONE', *, *, #43668, .F. ) ;
#7863 = ORIENTED_EDGE ( 'NONE', *, *, #6975, .T. ) ;
#7864 = DIRECTION ( 'NONE',  ( 0.5364919789714477361, 0.6444004775717706579, 0.5449076811759711036 ) ) ;
#7865 = DIRECTION ( 'NONE',  ( 0.007781995580012663651, -3.146120232559066537E-19, -0.9999697198139514409 ) ) ;
#7866 = CARTESIAN_POINT ( 'NONE',  ( -24.27063949748155380, 0.000000000000000000, 6.308861732390097288 ) ) ;
#7867 = AXIS2_PLACEMENT_3D ( 'NONE', #2523, #40610, #15042 ) ;
#7868 = LINE ( 'NONE', #46748, #14672 ) ;
#7869 = AXIS2_PLACEMENT_3D ( 'NONE', #48199, #18115, #9309 ) ;
#7870 = CARTESIAN_POINT ( 'NONE',  ( -12.35938774090218217, -0.3560938001956556742, 1.670765785740375931 ) ) ;
#7871 = FACE_OUTER_BOUND ( 'NONE', #36528, .T. ) ;
#7872 = FACE_OUTER_BOUND ( 'NONE', #5626, .T. ) ;
#7873 = EDGE_CURVE ( 'NONE', #5052, #49012, #38319, .T. ) ;
#7875 = VECTOR ( 'NONE', #41069, 1000.000000000000227 ) ;
#7874 = CARTESIAN_POINT ( 'NONE',  ( -3.775690919409564028, -5.709557508479220722, 4.684980151765822498 ) ) ;
#7876 = FACE_OUTER_BOUND ( 'NONE', #20902, .T. ) ;
#7877 = EDGE_CURVE ( 'NONE', #42368, #35767, #43435, .T. ) ;
#7878 = DIRECTION ( 'NONE',  ( 0.9999697198139515519, 0.000000000000000000, 0.007781995580013368816 ) ) ;
#7879 = ORIENTED_EDGE ( 'NONE', *, *, #20523, .T. ) ;
#7880 = CARTESIAN_POINT ( 'NONE',  ( -17.12040860686058608, -2.137015261443160341, 3.463287256266506908 ) ) ;
#7881 = ORIENTED_EDGE ( 'NONE', *, *, #42500, .F. ) ;
#7882 = EDGE_CURVE ( 'NONE', #31801, #3456, #17294, .T. ) ;
#7883 = VECTOR ( 'NONE', #12710, 1000.000000000000227 ) ;
#7884 = ORIENTED_EDGE ( 'NONE', *, *, #29190, .F. ) ;
#7885 = EDGE_CURVE ( 'NONE', #11310, #37777, #52242, .T. ) ;
#7886 = AXIS2_PLACEMENT_3D ( 'NONE', #53879, #14997, #2486 ) ;
#7887 = EDGE_LOOP ( 'NONE', ( #50820, #53085, #15001, #46614 ) ) ;
#7888 = VECTOR ( 'NONE', #29579, 1000.000000000000227 ) ;
#7889 = VERTEX_POINT ( 'NONE', #34620 ) ;
#7890 = ORIENTED_EDGE ( 'NONE', *, *, #6216, .F. ) ;
#7891 = ORIENTED_EDGE ( 'NONE', *, *, #55975, .F. ) ;
#7892 = CARTESIAN_POINT ( 'NONE',  ( -12.13851405436063047, 0.000000000000000000, 11.68505802764555135 ) ) ;
#7893 = CARTESIAN_POINT ( 'NONE',  ( -20.41355881641904801, 1.905425754524007198, 7.937768888670418299 ) ) ;
#7894 = EDGE_CURVE ( 'NONE', #52808, #30962, #47403, .T. ) ;
#7895 = PLANE ( 'NONE',  #37559 ) ;
#7896 = ORIENTED_EDGE ( 'NONE', *, *, #406, .F. ) ;
#7897 = CARTESIAN_POINT ( 'NONE',  ( -10.00813838035478298, 0.000000000000000000, 10.77830692922518452 ) ) ;
#7898 = ORIENTED_EDGE ( 'NONE', *, *, #39788, .F. ) ;
#7899 = CARTESIAN_POINT ( 'NONE',  ( -13.23530239847019097, 0.000000000000000000, 7.502737486787267152 ) ) ;
#7900 = ORIENTED_EDGE ( 'NONE', *, *, #27041, .F. ) ;
#7901 = AXIS2_PLACEMENT_3D ( 'NONE', #41492, #41740, #23343 ) ;
#7902 = CARTESIAN_POINT ( 'NONE',  ( -66.72811894189939608, -9.346592750493281088, 4.538413701023873870 ) ) ;
#7903 = DIRECTION ( 'NONE',  ( -0.9999697198139514409, -0.000000000000000000, -0.007781995580013368816 ) ) ;
#7904 = VERTEX_POINT ( 'NONE', #47704 ) ;
#7905 = FACE_OUTER_BOUND ( 'NONE', #22206, .T. ) ;
#7906 = ORIENTED_EDGE ( 'NONE', *, *, #13612, .T. ) ;
#7907 = CARTESIAN_POINT ( 'NONE',  ( -26.13493519185646008, 0.000000000000000000, 7.033017491833586377 ) ) ;
#7908 = AXIS2_PLACEMENT_3D ( 'NONE', #22602, #26564, #43886 ) ;
#7909 = CARTESIAN_POINT ( 'NONE',  ( -18.25349690304924266, -3.432230869623160263, 9.405085406872181863 ) ) ;
#7910 = DIRECTION ( 'NONE',  ( 0.5364919789714477361, 0.6444004775717706579, 0.5449076811759711036 ) ) ;
#7911 = AXIS2_PLACEMENT_3D ( 'NONE', #45275, #32507, #31668 ) ;
#7912 = CARTESIAN_POINT ( 'NONE',  ( -16.27184006575258834, 0.000000000000000000, 5.432440043275593489 ) ) ;
#7913 = LINE ( 'NONE', #51610, #232 ) ;
#7914 = PLANE ( 'NONE',  #26704 ) ;
#7915 = LINE ( 'NONE', #7604, #47445 ) ;
#7916 = LINE ( 'NONE', #21534, #51304 ) ;
#7917 = ORIENTED_EDGE ( 'NONE', *, *, #1095, .F. ) ;
#7918 = CARTESIAN_POINT ( 'NONE',  ( -13.07066190154808361, 0.000000000000000000, 12.04713590736729678 ) ) ;
#7919 = EDGE_LOOP ( 'NONE', ( #53073, #48892, #48367, #18125 ) ) ;
#7920 = EDGE_CURVE ( 'NONE', #46912, #17870, #3680, .T. ) ;
#7921 = VECTOR ( 'NONE', #12992, 1000.000000000000227 ) ;
#7922 = DIRECTION ( 'NONE',  ( 0.6427681459581294776, -0.7660444431189769032, 0.005002170337467562802 ) ) ;
#7923 = DIRECTION ( 'NONE',  ( 0.9999697198139515519, 0.000000000000000000, 0.007781995580013368816 ) ) ;
#7924 = LINE ( 'NONE', #25236, #29597 ) ;
#7925 = FACE_OUTER_BOUND ( 'NONE', #49773, .T. ) ;
#7926 = CARTESIAN_POINT ( 'NONE',  ( 4.452747148193316740, -1.000000000000000000, 0.4159841754879232689 ) ) ;
#7927 = EDGE_CURVE ( 'NONE', #14368, #23927, #17590, .T. ) ;
#7928 = EDGE_CURVE ( 'NONE', #33489, #1369, #30673, .T. ) ;
#7929 = DIRECTION ( 'NONE',  ( 0.000000000000000000, -0.000000000000000000, -1.000000000000000000 ) ) ;
#7930 = ORIENTED_EDGE ( 'NONE', *, *, #2189, .T. ) ;
#7931 = LINE ( 'NONE', #37741, #33782 ) ;
#7932 = CARTESIAN_POINT ( 'NONE',  ( -13.01938178786498490, 0.000000000000000000, 5.457751425651659716 ) ) ;
#7933 = CARTESIAN_POINT ( 'NONE',  ( -18.19747506107908563, 0.000000000000000000, 14.03856424583689311 ) ) ;
#7934 = DIRECTION ( 'NONE',  ( 0.5364919789714477361, 0.6444004775717706579, 0.5449076811759711036 ) ) ;
#7935 = CARTESIAN_POINT ( 'NONE',  ( -0.5433539342177339249, -4.971938947471305603, 3.429430696091245068 ) ) ;
#7936 = PLANE ( 'NONE',  #32112 ) ;
#7937 = CARTESIAN_POINT ( 'NONE',  ( -9.739739374040562225, 0.000000000000000000, 1.989959719412870864 ) ) ;
#7938 = CARTESIAN_POINT ( 'NONE',  ( -19.60834386242827776, 0.000000000000000000, 4.298478389818581213 ) ) ;
#7939 = EDGE_LOOP ( 'NONE', ( #50306, #3806, #51586, #10282 ) ) ;
#7940 = FACE_OUTER_BOUND ( 'NONE', #4886, .T. ) ;
#7941 = CARTESIAN_POINT ( 'NONE',  ( -19.48672417669920875, -0.5179957512181557755, 4.434099782880741358 ) ) ;
#7942 = ORIENTED_EDGE ( 'NONE', *, *, #22890, .T. ) ;
#7943 = ORIENTED_EDGE ( 'NONE', *, *, #6636, .F. ) ;
#7944 = LINE ( 'NONE', #8203, #41887 ) ;
#7945 = ORIENTED_EDGE ( 'NONE', *, *, #22829, .F. ) ;
#7946 = CARTESIAN_POINT ( 'NONE',  ( -9.411683945191542833, -0.1191753592594181482, 6.693826601992417302 ) ) ;
#7947 = EDGE_CURVE ( 'NONE', #44961, #38597, #47126, .T. ) ;
#7948 = VECTOR ( 'NONE', #34517, 1000.000000000000227 ) ;
#7949 = ORIENTED_EDGE ( 'NONE', *, *, #29580, .T. ) ;
#7950 = EDGE_LOOP ( 'NONE', ( #7237, #39812, #42487, #19720 ) ) ;
#7951 = EDGE_LOOP ( 'NONE', ( #21293, #37944, #11501, #38896 ) ) ;
#7952 = EDGE_CURVE ( 'NONE', #12432, #9106, #47971, .T. ) ;
#7953 = FACE_OUTER_BOUND ( 'NONE', #6336, .T. ) ;
#7954 = CARTESIAN_POINT ( 'NONE',  ( -20.08254794625849371, -0.1191753592594172878, 4.582370052862001941 ) ) ;
#7955 = EDGE_CURVE ( 'NONE', #17655, #9986, #26126, .T. ) ;
#7956 = CARTESIAN_POINT ( 'NONE',  ( -26.13493519185646008, 0.000000000000000000, 7.033017491833586377 ) ) ;
#7957 = VECTOR ( 'NONE', #35349, 999.9999999999998863 ) ;
#7958 = ORIENTED_EDGE ( 'NONE', *, *, #53238, .F. ) ;
#7959 = EDGE_CURVE ( 'NONE', #33216, #21642, #34360, .T. ) ;
#7960 = ORIENTED_EDGE ( 'NONE', *, *, #41386, .F. ) ;
#7961 = DIRECTION ( 'NONE',  ( 0.000000000000000000, -1.000000000000000000, 0.000000000000000000 ) ) ;
#7962 = PLANE ( 'NONE',  #30916 ) ;
#7963 = ORIENTED_EDGE ( 'NONE', *, *, #21216, .F. ) ;
#7964 = DIRECTION ( 'NONE',  ( -0.000000000000000000, -0.000000000000000000, 1.000000000000000000 ) ) ;
#7965 = FACE_OUTER_BOUND ( 'NONE', #55178, .T. ) ;
#7966 = ORIENTED_EDGE ( 'NONE', *, *, #41593, .T. ) ;
#7967 = DIRECTION ( 'NONE',  ( 0.5449076811759707706, 0.6444004775717708799, -0.5364919789714476250 ) ) ;
#7968 = CARTESIAN_POINT ( 'NONE',  ( -17.93139508144814442, 0.000000000000000000, 13.85596890686001537 ) ) ;
#7969 = EDGE_LOOP ( 'NONE', ( #31139, #28607, #27451, #22838 ) ) ;
#7970 = CARTESIAN_POINT ( 'NONE',  ( -12.63184290468442228, -0.6798977022406560433, 1.766265584194925520 ) ) ;
#7971 = ADVANCED_FACE ( 'NONE', ( #38052 ), #3967, .F. ) ;
#7972 = CARTESIAN_POINT ( 'NONE',  ( -18.39746900504187010, 0.000000000000000000, 14.03700784672088808 ) ) ;
#7973 = EDGE_LOOP ( 'NONE', ( #22109, #11223, #27791, #55619 ) ) ;
#7974 = DIRECTION ( 'NONE',  ( 0.7660212471507180654, -0.6427876096865404731, 0.005961354470445141482 ) ) ;
#7975 = DIRECTION ( 'NONE',  ( 0.7660212471507180654, -0.6427876096865404731, 0.005961354470445141482 ) ) ;
#7976 = DIRECTION ( 'NONE',  ( 0.5449076811759707706, 0.6444004775717708799, -0.5364919789714476250 ) ) ;
#7977 = CARTESIAN_POINT ( 'NONE',  ( -15.40103151951671734, 0.000000000000000000, 12.95233060667165681 ) ) ;
#7978 = EDGE_CURVE ( 'NONE', #27927, #31613, #16455, .T. ) ;
#7979 = ORIENTED_EDGE ( 'NONE', *, *, #50759, .F. ) ;
#7980 = EDGE_CURVE ( 'NONE', #29025, #53596, #51103, .T. ) ;
#7981 = PLANE ( 'NONE',  #41897 ) ;
#7982 = CARTESIAN_POINT ( 'NONE',  ( -13.07066190154808361, 0.000000000000000000, 12.04713590736729678 ) ) ;
#7983 = DIRECTION ( 'NONE',  ( 0.9999697198139515519, 0.000000000000000000, 0.007781995580013368816 ) ) ;
#7984 = DIRECTION ( 'NONE',  ( 0.7660212471507180654, -0.6427876096865404731, 0.005961354470445141482 ) ) ;
#7985 = CARTESIAN_POINT ( 'NONE',  ( -16.84300024114363126, -0.1191753592594194527, 6.266662310446504236 ) ) ;
#7986 = EDGE_CURVE ( 'NONE', #53467, #40095, #39745, .T. ) ;
#7987 = DIRECTION ( 'NONE',  ( -0.5364919789714478471, 0.6444004775717705469, -0.5449076811759709926 ) ) ;
#7988 = PLANE ( 'NONE',  #31281 ) ;
#7989 = ORIENTED_EDGE ( 'NONE', *, *, #36421, .F. ) ;
#7990 = DIRECTION ( 'NONE',  ( 0.000000000000000000, -1.000000000000000000, 0.000000000000000000 ) ) ;
#7991 = VERTEX_POINT ( 'NONE', #18728 ) ;
#7992 = DIRECTION ( 'NONE',  ( -0.005002170337468016433, -0.7660444431189770143, 0.6427681459581293666 ) ) ;
#7993 = PLANE ( 'NONE',  #48123 ) ;
#7994 = VECTOR ( 'NONE', #51117, 999.9999999999998863 ) ;
#7995 = PLANE ( 'NONE',  #21316 ) ;
#7996 = PLANE ( 'NONE',  #27833 ) ;
#7997 = DIRECTION ( 'NONE',  ( -0.005961354470445682716, -0.6427876096865404731, 0.7660212471507180654 ) ) ;
#7998 = EDGE_CURVE ( 'NONE', #1435, #3706, #36309, .T. ) ;
#7999 = ORIENTED_EDGE ( 'NONE', *, *, #18609, .T. ) ;
#8000 = EDGE_LOOP ( 'NONE', ( #33377, #85, #13666, #22740 ) ) ;
#8001 = DIRECTION ( 'NONE',  ( 0.007781995580012663651, 0.000000000000000000, -0.9999697198139515519 ) ) ;
#8002 = CARTESIAN_POINT ( 'NONE',  ( -22.40556560354864146, -0.1191753592594197858, 5.484709000965211523 ) ) ;
#8003 = ORIENTED_EDGE ( 'NONE', *, *, #40168, .F. ) ;
#8004 = CARTESIAN_POINT ( 'NONE',  ( -16.95239757319887985, 0.000000000000000000, 7.473810192643190575 ) ) ;
#8005 = VERTEX_POINT ( 'NONE', #35212 ) ;
#8006 = PLANE ( 'NONE',  #43096 ) ;
#8007 = ORIENTED_EDGE ( 'NONE', *, *, #20818, .F. ) ;
#8008 = DIRECTION ( 'NONE',  ( 0.000000000000000000, -0.000000000000000000, -1.000000000000000000 ) ) ;
#8009 = ORIENTED_EDGE ( 'NONE', *, *, #29334, .F. ) ;
#8010 = ORIENTED_EDGE ( 'NONE', *, *, #22681, .T. ) ;
#8011 = VERTEX_POINT ( 'NONE', #559 ) ;
#8012 = LINE ( 'NONE', #16803, #3018 ) ;
#8013 = PLANE ( 'NONE',  #9626 ) ;
#8014 = DIRECTION ( 'NONE',  ( -0.5364919789714478471, 0.6444004775717705469, -0.5449076811759709926 ) ) ;
#8015 = PLANE ( 'NONE',  #49217 ) ;
#8016 = EDGE_CURVE ( 'NONE', #46316, #46703, #52774, .T. ) ;
#8017 = EDGE_LOOP ( 'NONE', ( #55679, #17682, #19596, #20289 ) ) ;
#8018 = EDGE_LOOP ( 'NONE', ( #21124, #51584, #49200, #6106 ) ) ;
#8019 = VERTEX_POINT ( 'NONE', #13879 ) ;
#8020 = DIRECTION ( 'NONE',  ( 0.7660212471507180654, -0.6427876096865404731, 0.005961354470445141482 ) ) ;
#8021 = DIRECTION ( 'NONE',  ( -0.9999697198139514409, -0.000000000000000000, -0.007781995580013368816 ) ) ;
#8022 = ORIENTED_EDGE ( 'NONE', *, *, #41391, .F. ) ;
#8023 = DIRECTION ( 'NONE',  ( 0.007781995580012662783, 0.000000000000000000, -0.9999697198139514409 ) ) ;
#8024 = VERTEX_POINT ( 'NONE', #5108 ) ;
#8025 = FACE_OUTER_BOUND ( 'NONE', #46393, .T. ) ;
#8026 = LINE ( 'NONE', #25072, #25809 ) ;
#8027 = EDGE_CURVE ( 'NONE', #44511, #5651, #31206, .T. ) ;
#8028 = AXIS2_PLACEMENT_3D ( 'NONE', #53918, #1683, #32370 ) ;
#8029 = ORIENTED_EDGE ( 'NONE', *, *, #15266, .F. ) ;
#8030 = FACE_OUTER_BOUND ( 'NONE', #33657, .T. ) ;
#8031 = ORIENTED_EDGE ( 'NONE', *, *, #34221, .F. ) ;
#8032 = EDGE_CURVE ( 'NONE', #22613, #21479, #35759, .T. ) ;
#8033 = ADVANCED_FACE ( 'NONE', ( #22437 ), #5643, .F. ) ;
#8034 = DIRECTION ( 'NONE',  ( -0.5364919789714478471, 0.6444004775717705469, -0.5449076811759709926 ) ) ;
#8035 = DIRECTION ( 'NONE',  ( 0.9999697198139515519, 0.000000000000000000, 0.007781995580013368816 ) ) ;
#8036 = ORIENTED_EDGE ( 'NONE', *, *, #41778, .F. ) ;
#8037 = CARTESIAN_POINT ( 'NONE',  ( -15.13495153988577968, 0.000000000000000000, 12.76973526769478084 ) ) ;
#8038 = DIRECTION ( 'NONE',  ( 0.007781995580012662783, 0.000000000000000000, -0.9999697198139514409 ) ) ;
#8039 = LINE ( 'NONE', #25350, #9662 ) ;
#8040 = CARTESIAN_POINT ( 'NONE',  ( -17.26532721389163072, 0.000000000000000000, 13.67648636611514590 ) ) ;
#8041 = ORIENTED_EDGE ( 'NONE', *, *, #44751, .F. ) ;
#8042 = ORIENTED_EDGE ( 'NONE', *, *, #45271, .F. ) ;
#8043 = EDGE_CURVE ( 'NONE', #44617, #54500, #17892, .T. ) ;
#8044 = FACE_OUTER_BOUND ( 'NONE', #21128, .T. ) ;
#8045 = DIRECTION ( 'NONE',  ( 0.5449076811759707706, 0.6444004775717708799, -0.5364919789714476250 ) ) ;
#8046 = CARTESIAN_POINT ( 'NONE',  ( -13.69550884268998914, 0.000000000000000000, 6.929817927798703536 ) ) ;
#8047 = DIRECTION ( 'NONE',  ( 0.005961354470445682716, -0.6427876096865404731, -0.7660212471507180654 ) ) ;
#8048 = EDGE_CURVE ( 'NONE', #45704, #20591, #14726, .T. ) ;
#8049 = LINE ( 'NONE', #51490, #28829 ) ;
#8050 = FACE_OUTER_BOUND ( 'NONE', #53557, .T. ) ;
#8051 = ORIENTED_EDGE ( 'NONE', *, *, #1487, .F. ) ;
#8052 = LINE ( 'NONE', #21083, #40700 ) ;
#8053 = FACE_OUTER_BOUND ( 'NONE', #19809, .T. ) ;
#8054 = DIRECTION ( 'NONE',  ( -0.6427681459581293666, -0.7660444431189770143, -0.005002170337467561935 ) ) ;
#8055 = ORIENTED_EDGE ( 'NONE', *, *, #4326, .T. ) ;
#8056 = DIRECTION ( 'NONE',  ( -0.005961354470445682716, -0.6427876096865404731, 0.7660212471507180654 ) ) ;
#8057 = VERTEX_POINT ( 'NONE', #49371 ) ;
#8058 = EDGE_CURVE ( 'NONE', #6678, #3929, #48532, .T. ) ;
#8059 = CARTESIAN_POINT ( 'NONE',  ( -16.53317331066696383, 0.000000000000000000, 13.31285208727739899 ) ) ;
#8060 = CARTESIAN_POINT ( 'NONE',  ( -19.61932540816901849, -0.1191753592594174127, 4.767728026807386499 ) ) ;
#8061 = DIRECTION ( 'NONE',  ( 0.9999697198139515519, 0.000000000000000000, 0.007781995580013368816 ) ) ;
#8062 = CARTESIAN_POINT ( 'NONE',  ( -22.62703048288702234, 4.495856970884011261, 13.04889539694818623 ) ) ;
#8063 = CARTESIAN_POINT ( 'NONE',  ( -69.53894961980590494, 1.999999999999173550, -7.108028418033228490 ) ) ;
#8064 = EDGE_CURVE ( 'NONE', #29959, #29873, #1664, .T. ) ;
#8065 = ORIENTED_EDGE ( 'NONE', *, *, #10157, .F. ) ;
#8066 = ORIENTED_EDGE ( 'NONE', *, *, #29158, .T. ) ;
#8067 = DIRECTION ( 'NONE',  ( 0.5364919789714477361, 0.6444004775717706579, 0.5449076811759711036 ) ) ;
#8068 = CARTESIAN_POINT ( 'NONE',  ( -20.54049170961573267, 0.000000000000000000, 4.660556269540326646 ) ) ;
#8069 = LINE ( 'NONE', #25647, #27811 ) ;
#8070 = LINE ( 'NONE', #3782, #13226 ) ;
#8071 = AXIS2_PLACEMENT_3D ( 'NONE', #38134, #42964, #3508 ) ;
#8072 = DIRECTION ( 'NONE',  ( 0.5364919789714477361, 0.6444004775717706579, 0.5449076811759711036 ) ) ;
#8073 = LINE ( 'NONE', #16876, #21275 ) ;
#8074 = ORIENTED_EDGE ( 'NONE', *, *, #14777, .T. ) ;
#8075 = PLANE ( 'NONE',  #54609 ) ;
#8076 = DIRECTION ( 'NONE',  ( 0.5364919789714477361, 0.6444004775717706579, 0.5449076811759711036 ) ) ;
#8077 = CARTESIAN_POINT ( 'NONE',  ( -12.33850799832341849, 0.000000000000000000, 11.68350162852954632 ) ) ;
#8078 = ORIENTED_EDGE ( 'NONE', *, *, #42633, .T. ) ;
#8079 = CARTESIAN_POINT ( 'NONE',  ( -10.74029228357944987, 0.000000000000000000, 11.14194120806293320 ) ) ;
#8080 = CARTESIAN_POINT ( 'NONE',  ( -16.81345671998191449, 0.000000000000000000, 3.412238694616132495 ) ) ;
#8081 = FACE_OUTER_BOUND ( 'NONE', #45703, .T. ) ;
#8082 = ORIENTED_EDGE ( 'NONE', *, *, #36826, .F. ) ;
#8083 = CARTESIAN_POINT ( 'NONE',  ( -19.73159679372954045, 0.000000000000000000, 6.344185612261842522 ) ) ;
#8084 = EDGE_CURVE ( 'NONE', #23572, #10480, #18141, .T. ) ;
#8085 = ADVANCED_FACE ( 'NONE', ( #26968 ), #4805, .F. ) ;
#8086 = VERTEX_POINT ( 'NONE', #44282 ) ;
#8087 = EDGE_LOOP ( 'NONE', ( #44632, #22603, #3903, #12119 ) ) ;
#8088 = ORIENTED_EDGE ( 'NONE', *, *, #26195, .T. ) ;
#8089 = VERTEX_POINT ( 'NONE', #22130 ) ;
#8090 = DIRECTION ( 'NONE',  ( 0.007781995580012663651, -3.146120232559066537E-19, -0.9999697198139514409 ) ) ;
#8092 = EDGE_CURVE ( 'NONE', #47173, #10102, #13603, .T. ) ;
#8091 = VERTEX_POINT ( 'NONE', #1086 ) ;
#8093 = CARTESIAN_POINT ( 'NONE',  ( -12.74324262096555849, 0.000000000000000000, 3.982572125272607622 ) ) ;
#8094 = EDGE_CURVE ( 'NONE', #7759, #27005, #18422, .T. ) ;
#8095 = EDGE_CURVE ( 'NONE', #14361, #33224, #31515, .T. ) ;
#8096 = ORIENTED_EDGE ( 'NONE', *, *, #7019, .F. ) ;
#8097 = FACE_OUTER_BOUND ( 'NONE', #53344, .T. ) ;
#8098 = ORIENTED_EDGE ( 'NONE', *, *, #55319, .F. ) ;
#8099 = ORIENTED_EDGE ( 'NONE', *, *, #7075, .F. ) ;
#8100 = EDGE_CURVE ( 'NONE', #44385, #26435, #9924, .T. ) ;
#8101 = DIRECTION ( 'NONE',  ( 0.007781995580012663651, -3.146120232559066537E-19, -0.9999697198139514409 ) ) ;
#8102 = LINE ( 'NONE', #25152, #36811 ) ;
#8103 = CARTESIAN_POINT ( 'NONE',  ( -28.93137873341882127, 0.000000000000000000, 8.119251130998824451 ) ) ;
#8104 = CARTESIAN_POINT ( 'NONE',  ( -11.45287710155235850, 1.257817950434005683, 1.090487161058584231 ) ) ;
#8105 = LINE ( 'NONE', #55799, #41940 ) ;
#8106 = ORIENTED_EDGE ( 'NONE', *, *, #55195, .F. ) ;
#8107 = PRESENTATION_LAYER_ASSIGNMENT (  '', '', ( #32581 ) ) ;
#8108 = ORIENTED_EDGE ( 'NONE', *, *, #10194, .T. ) ;
#8109 = EDGE_CURVE ( 'NONE', #22478, #32939, #31776, .T. ) ;
#8110 = PLANE ( 'NONE',  #6819 ) ;
#8111 = DIRECTION ( 'NONE',  ( 0.007781995580012662783, 0.000000000000000000, -0.9999697198139514409 ) ) ;
#8112 = ADVANCED_FACE ( 'NONE', ( #54443 ), #33179, .F. ) ;
#8113 = LINE ( 'NONE', #21730, #48738 ) ;
#8114 = FACE_OUTER_BOUND ( 'NONE', #6606, .T. ) ;
#8115 = ADVANCED_FACE ( 'NONE', ( #27814 ), #49907, .F. ) ;
#8116 = PLANE ( 'NONE',  #26757 ) ;
#8117 = DIRECTION ( 'NONE',  ( 0.007781995580012663651, -3.146120232559066537E-19, -0.9999697198139514409 ) ) ;
#8118 = ORIENTED_EDGE ( 'NONE', *, *, #54176, .F. ) ;
#8119 = FACE_OUTER_BOUND ( 'NONE', #29179, .T. ) ;
#8120 = DIRECTION ( 'NONE',  ( 0.5449076811759707706, 0.6444004775717708799, -0.5364919789714476250 ) ) ;
#8121 = VERTEX_POINT ( 'NONE', #54729 ) ;
#8122 = EDGE_CURVE ( 'NONE', #41133, #50088, #28333, .T. ) ;
#8123 = CARTESIAN_POINT ( 'NONE',  ( -16.48776067635779441, 0.000000000000000000, 7.477426104411200924 ) ) ;
#8124 = CARTESIAN_POINT ( 'NONE',  ( -10.84028925556084388, -0.1191753592594197858, 11.14116300850493246 ) ) ;
#8125 = PLANE ( 'NONE',  #50832 ) ;
#8126 = CARTESIAN_POINT ( 'NONE',  ( -15.40103151951671734, 0.000000000000000000, 12.95233060667165681 ) ) ;
#8127 = DIRECTION ( 'NONE',  ( 0.7660212471507180654, -0.6427876096865404731, 0.005961354470445141482 ) ) ;
#8128 = ORIENTED_EDGE ( 'NONE', *, *, #23016, .T. ) ;
#8129 = ORIENTED_EDGE ( 'NONE', *, *, #47519, .T. ) ;
#8130 = CARTESIAN_POINT ( 'NONE',  ( -15.03495456790438389, -0.1191753592594197858, 12.77051346725278158 ) ) ;
#8131 = DIRECTION ( 'NONE',  ( 0.005961354470445682716, -0.6427876096865404731, -0.7660212471507180654 ) ) ;
#8132 = LINE ( 'NONE', #15504, #7051 ) ;
#8133 = DIRECTION ( 'NONE',  ( -2.710505431213760161E-17, 4.336808689942016257E-16, -1.000000000000000000 ) ) ;
#8134 = DIRECTION ( 'NONE',  ( 0.7660212471507180654, -0.6427876096865404731, 0.005961354470445141482 ) ) ;
#8135 = CARTESIAN_POINT ( 'NONE',  ( -11.88054826722768276, 25.79903810567671130, -3.000000000000000000 ) ) ;
#8136 = CARTESIAN_POINT ( 'NONE',  ( -17.26532721389163072, 0.000000000000000000, 13.67648636611514590 ) ) ;
#8137 = FACE_OUTER_BOUND ( 'NONE', #22260, .T. ) ;
#8138 = CARTESIAN_POINT ( 'NONE',  ( -68.75329340164451253, -8.572274407770867910, 6.394134653913044808 ) ) ;
#8139 = PLANE ( 'NONE',  #37394 ) ;
#8140 = VERTEX_POINT ( 'NONE', #36587 ) ;
#8141 = CARTESIAN_POINT ( 'NONE',  ( -16.96165138597773137, 2.229229656569007290, 7.128348183318155229 ) ) ;
#8142 = EDGE_CURVE ( 'NONE', #45422, #51315, #1009, .T. ) ;
#8143 = ORIENTED_EDGE ( 'NONE', *, *, #40264, .F. ) ;
#8144 = EDGE_CURVE ( 'NONE', #26049, #7904, #28067, .T. ) ;
#8145 = EDGE_LOOP ( 'NONE', ( #35752, #53299, #5889, #49854 ) ) ;
#8146 = ORIENTED_EDGE ( 'NONE', *, *, #18738, .F. ) ;
#8147 = ORIENTED_EDGE ( 'NONE', *, *, #54315, .F. ) ;
#8148 = ORIENTED_EDGE ( 'NONE', *, *, #20545, .F. ) ;
#8149 = EDGE_LOOP ( 'NONE', ( #5634, #22556, #33229, #28921 ) ) ;
#8150 = DIRECTION ( 'NONE',  ( 0.5449076811759707706, 0.6444004775717708799, -0.5364919789714476250 ) ) ;
#8151 = DIRECTION ( 'NONE',  ( 0.005002170337468016433, -0.7660444431189770143, -0.6427681459581293666 ) ) ;
#8152 = DIRECTION ( 'NONE',  ( 0.005002170337468016433, -0.7660444431189770143, -0.6427681459581293666 ) ) ;
#8153 = EDGE_CURVE ( 'NONE', #2187, #19558, #28634, .T. ) ;
#8154 = EDGE_CURVE ( 'NONE', #23769, #12809, #54194, .T. ) ;
#8155 = EDGE_CURVE ( 'NONE', #39340, #49361, #2505, .T. ) ;
#8156 = VERTEX_POINT ( 'NONE', #45372 ) ;
#8157 = DIRECTION ( 'NONE',  ( -0.9999697198139514409, -0.000000000000000000, -0.007781995580013368816 ) ) ;
#8158 = ORIENTED_EDGE ( 'NONE', *, *, #52905, .F. ) ;
#8159 = DIRECTION ( 'NONE',  ( 0.007781995580012662783, 0.000000000000000000, -0.9999697198139514409 ) ) ;
#8160 = EDGE_CURVE ( 'NONE', #40567, #21134, #50193, .T. ) ;
#8161 = ORIENTED_EDGE ( 'NONE', *, *, #20936, .F. ) ;
#8162 = DIRECTION ( 'NONE',  ( 0.000000000000000000, -1.000000000000000000, 0.000000000000000000 ) ) ;
#8163 = FACE_OUTER_BOUND ( 'NONE', #23984, .T. ) ;
#8164 = CARTESIAN_POINT ( 'NONE',  ( -12.73462046044971174, 0.000000000000000000, 2.874643015499314558 ) ) ;
#8165 = EDGE_LOOP ( 'NONE', ( #23731, #38820, #45759, #45818 ) ) ;
#8166 = DIRECTION ( 'NONE',  ( -0.005002170337468016433, -0.7660444431189770143, 0.6427681459581293666 ) ) ;
#8167 = ORIENTED_EDGE ( 'NONE', *, *, #27917, .F. ) ;
#8168 = PLANE ( 'NONE',  #4660 ) ;
#8169 = CARTESIAN_POINT ( 'NONE',  ( -18.13481810573821562, 0.000000000000000000, 5.987280043424108911 ) ) ;
#8170 = ADVANCED_FACE ( 'NONE', ( #23793 ), #45651, .F. ) ;
#8171 = VECTOR ( 'NONE', #44237, 999.9999999999998863 ) ;
#8172 = DIRECTION ( 'NONE',  ( -1.000000000000000000, 0.000000000000000000, 0.000000000000000000 ) ) ;
#8173 = CARTESIAN_POINT ( 'NONE',  ( -10.90062170024363297, 0.000000000000000000, 6.043578232596257038 ) ) ;
#8174 = LINE ( 'NONE', #41945, #20218 ) ;
#8175 = PLANE ( 'NONE',  #1328 ) ;
#8176 = EDGE_CURVE ( 'NONE', #23263, #29692, #11301, .T. ) ;
#8177 = LINE ( 'NONE', #55047, #3047 ) ;
#8178 = CARTESIAN_POINT ( 'NONE',  ( -70.57153585115312922, -8.780779913117141788, -8.550077602493740159 ) ) ;
#8179 = ORIENTED_EDGE ( 'NONE', *, *, #48619, .F. ) ;
#8180 = DIRECTION ( 'NONE',  ( 0.000000000000000000, -0.000000000000000000, -1.000000000000000000 ) ) ;
#8181 = ORIENTED_EDGE ( 'NONE', *, *, #22370, .F. ) ;
#8182 = EDGE_CURVE ( 'NONE', #28225, #33592, #2755, .T. ) ;
#8183 = FACE_OUTER_BOUND ( 'NONE', #22695, .T. ) ;
#8184 = DIRECTION ( 'NONE',  ( 0.005002170337468016433, -0.7660444431189770143, -0.6427681459581293666 ) ) ;
#8185 = CARTESIAN_POINT ( 'NONE',  ( -10.27421835998572064, 0.000000000000000000, 10.96090226820206048 ) ) ;
#8186 = LINE ( 'NONE', #25495, #8637 ) ;
#8187 = FACE_OUTER_BOUND ( 'NONE', #2863, .T. ) ;
#8188 = ADVANCED_FACE ( 'NONE', ( #7062 ), #24360, .F. ) ;
#8189 = CARTESIAN_POINT ( 'NONE',  ( -1.086233639165236964, 0.000000000000000000, -2.796443541562362078 ) ) ;
#8190 = ORIENTED_EDGE ( 'NONE', *, *, #17450, .T. ) ;
#8191 = CARTESIAN_POINT ( 'NONE',  ( -14.43915895993578502, 0.000000000000000000, 8.770691019667511412 ) ) ;
#8192 = LINE ( 'NONE', #21550, #15853 ) ;
#8193 = DIRECTION ( 'NONE',  ( -0.005961354470445682716, -0.6427876096865404731, 0.7660212471507180654 ) ) ;
#8194 = DIRECTION ( 'NONE',  ( 0.007781995580012663651, -3.146120232559066537E-19, -0.9999697198139514409 ) ) ;
#8195 = DIRECTION ( 'NONE',  ( -0.5449076811759708816, 0.6444004775717707689, 0.5364919789714475140 ) ) ;
#8196 = LINE ( 'NONE', #43404, #42237 ) ;
#8197 = CARTESIAN_POINT ( 'NONE',  ( 4.912750499197526821, -1.131233082521083455, -2.061810099490656079 ) ) ;
#8198 = ORIENTED_EDGE ( 'NONE', *, *, #27030, .F. ) ;
#8199 = LINE ( 'NONE', #16716, #1337 ) ;
#8200 = CARTESIAN_POINT ( 'NONE',  ( -16.81267852042391198, -0.1191753592594197858, 3.312241722634738039 ) ) ;
#8201 = EDGE_LOOP ( 'NONE', ( #28961, #36035, #38286, #20791 ) ) ;
#8202 = ORIENTED_EDGE ( 'NONE', *, *, #48286, .T. ) ;
#8203 = CARTESIAN_POINT ( 'NONE',  ( -15.08393937872457791, -3.594132820645662196, 2.625763770285873377 ) ) ;
#8204 = EDGE_LOOP ( 'NONE', ( #25923, #13500, #41157, #46833 ) ) ;
#8205 = VECTOR ( 'NONE', #32973, 1000.000000000000000 ) ;
#8206 = VERTEX_POINT ( 'NONE', #31959 ) ;
#8207 = EDGE_LOOP ( 'NONE', ( #50054, #36499, #17631, #55686, #8855, #33481, #38964, #30023, #15521, #966, #853, #44657, #16811, #11888, #5681, #16108, #42187, #49212, #17983, #44204, #10008, #55510, #27109, #38459, #53833, #37444, #11051, #36435, #24752, #6989, #52277, #25982, #41057, #22494, #20552, #55853, #13948, #25433, #46256, #38646, #25003, #42449, #22631, #27397, #8108, #14040, #21896 ) ) ;
#8208 = EDGE_LOOP ( 'NONE', ( #21419, #6416, #542, #50568 ) ) ;
#8209 = LINE ( 'NONE', #42841, #47510 ) ;
#8210 = ORIENTED_EDGE ( 'NONE', *, *, #43779, .T. ) ;
#8211 = CARTESIAN_POINT ( 'NONE',  ( -12.23851102634202448, -0.1191753592594197858, 11.68427982808754884 ) ) ;
#8212 = DIRECTION ( 'NONE',  ( -0.000000000000000000, -1.000000000000000000, -0.000000000000000000 ) ) ;
#8213 = EDGE_CURVE ( 'NONE', #7098, #42447, #6149, .T. ) ;
#8214 = ORIENTED_EDGE ( 'NONE', *, *, #24597, .T. ) ;
#8215 = ORIENTED_EDGE ( 'NONE', *, *, #15158, .T. ) ;
#8216 = EDGE_CURVE ( 'NONE', #40269, #55983, #18916, .T. ) ;
#8217 = EDGE_CURVE ( 'NONE', #42498, #30608, #39917, .T. ) ;
#8218 = DIRECTION ( 'NONE',  ( -0.005002170337468016433, -0.7660444431189770143, 0.6427681459581293666 ) ) ;
#8219 = DIRECTION ( 'NONE',  ( -0.9999697198139514409, -0.000000000000000000, -0.007781995580013368816 ) ) ;
#8220 = ORIENTED_EDGE ( 'NONE', *, *, #1870, .T. ) ;
#8221 = LINE ( 'NONE', #12759, #33687 ) ;
#8222 = DIRECTION ( 'NONE',  ( 0.5364919789714477361, 0.6444004775717706579, 0.5449076811759711036 ) ) ;
#8223 = ORIENTED_EDGE ( 'NONE', *, *, #14640, .T. ) ;
#8224 = DIRECTION ( 'NONE',  ( 0.000000000000000000, -1.000000000000000000, 0.000000000000000000 ) ) ;
#8225 = EDGE_LOOP ( 'NONE', ( #6025, #6205, #40997, #54655 ) ) ;
#8226 = CARTESIAN_POINT ( 'NONE',  ( -10.90636980725419924, 0.000000000000000000, 6.782197639111785747 ) ) ;
#8227 = DIRECTION ( 'NONE',  ( 0.007781995580012663651, -3.146120232559066537E-19, -0.9999697198139514409 ) ) ;
#8228 = ORIENTED_EDGE ( 'NONE', *, *, #18691, .T. ) ;
#8229 = CARTESIAN_POINT ( 'NONE',  ( -21.45130150109525502, -2.298917212465658721, 5.140387614241637593 ) ) ;
#8230 = CARTESIAN_POINT ( 'NONE',  ( 2.072287782118878319, 0.000000000000000000, -2.950529333540147015 ) ) ;
#8231 = DIRECTION ( 'NONE',  ( 0.000000000000000000, -0.000000000000000000, -1.000000000000000000 ) ) ;
#8232 = CARTESIAN_POINT ( 'NONE',  ( -12.67473335678518787, -2.946525016555661125, 1.710608413933282446 ) ) ;
#8233 = ORIENTED_EDGE ( 'NONE', *, *, #40287, .F. ) ;
#8234 = VECTOR ( 'NONE', #48610, 1000.000000000000227 ) ;
#8235 = LINE ( 'NONE', #21598, #52760 ) ;
#8236 = PLANE ( 'NONE',  #49606 ) ;
#8237 = PLANE ( 'NONE',  #53008 ) ;
#8238 = CARTESIAN_POINT ( 'NONE',  ( -20.34615672165342914, -0.4026555460309505508, 5.262860474000830457 ) ) ;
#8239 = EDGE_CURVE ( 'NONE', #22811, #19098, #31113, .T. ) ;
#8240 = FACE_OUTER_BOUND ( 'NONE', #37728, .T. ) ;
#8241 = CARTESIAN_POINT ( 'NONE',  ( -17.78010129026580444, -1.813211359398158029, 3.729865337533703862 ) ) ;
#8242 = AXIS2_PLACEMENT_3D ( 'NONE', #33472, #33736, #2777 ) ;
#8243 = LINE ( 'NONE', #25863, #24068 ) ;
#8244 = ORIENTED_EDGE ( 'NONE', *, *, #20286, .F. ) ;
#8245 = ADVANCED_FACE ( 'NONE', ( #23454 ), #9552, .F. ) ;
#8246 = FACE_OUTER_BOUND ( 'NONE', #29920, .T. ) ;
#8247 = VERTEX_POINT ( 'NONE', #49576 ) ;
#8248 = CARTESIAN_POINT ( 'NONE',  ( -23.33849165029409889, 0.000000000000000000, 5.946783852668351855 ) ) ;
#8249 = DIRECTION ( 'NONE',  ( 0.000000000000000000, -0.000000000000000000, -1.000000000000000000 ) ) ;
#8250 = EDGE_CURVE ( 'NONE', #1446, #50929, #997, .T. ) ;
#8251 = CARTESIAN_POINT ( 'NONE',  ( -13.49066169485000977, -4.403642575758160760, 9.149290569145874130 ) ) ;
#8252 = DIRECTION ( 'NONE',  ( -0.5449076811759708816, 0.6444004775717707689, 0.5364919789714475140 ) ) ;
#8253 = DIRECTION ( 'NONE',  ( 0.6427681459581294776, -0.7660444431189769032, 0.005002170337467562802 ) ) ;
#8254 = VERTEX_POINT ( 'NONE', #36490 ) ;
#8255 = VERTEX_POINT ( 'NONE', #40502 ) ;
#8256 = DIRECTION ( 'NONE',  ( 0.000000000000000000, 0.000000000000000000, -1.000000000000000000 ) ) ;
#8257 = DIRECTION ( 'NONE',  ( 0.007781995580012663651, -3.146120232559066537E-19, -0.9999697198139514409 ) ) ;
#8258 = EDGE_LOOP ( 'NONE', ( #30365, #32129, #5093, #11207 ) ) ;
#8259 = FACE_OUTER_BOUND ( 'NONE', #46435, .T. ) ;
#8260 = AXIS2_PLACEMENT_3D ( 'NONE', #273, #52537, #47996 ) ;
#8261 = VECTOR ( 'NONE', #27021, 1000.000000000000000 ) ;
#8262 = EDGE_LOOP ( 'NONE', ( #26177, #48371, #21766, #18816 ) ) ;
#8263 = CARTESIAN_POINT ( 'NONE',  ( -14.51981575693820581, -0.1191753592594177180, 6.284741869286547100 ) ) ;
#8264 = ORIENTED_EDGE ( 'NONE', *, *, #40320, .F. ) ;
#8265 = DIRECTION ( 'NONE',  ( 0.000000000000000000, -0.000000000000000000, -1.000000000000000000 ) ) ;
#8266 = ORIENTED_EDGE ( 'NONE', *, *, #44650, .T. ) ;
#8267 = EDGE_LOOP ( 'NONE', ( #26895, #44707, #29685, #35578 ) ) ;
#8268 = ORIENTED_EDGE ( 'NONE', *, *, #16534, .T. ) ;
#8269 = LINE ( 'NONE', #52294, #34784 ) ;
#8270 = EDGE_CURVE ( 'NONE', #46401, #35585, #39665, .T. ) ;
#8271 = PLANE ( 'NONE',  #7843 ) ;
#8272 = CARTESIAN_POINT ( 'NONE',  ( -15.32150246818737394, 0.000000000000000000, 2.733018303394165294 ) ) ;
#8273 = ADVANCED_FACE ( 'NONE', ( #14380 ), #26872, .F. ) ;
#8275 = DIRECTION ( 'NONE',  ( 0.5449076811759707706, 0.6444004775717708799, -0.5364919789714476250 ) ) ;
#8274 = VECTOR ( 'NONE', #10488, 1000.000000000000000 ) ;
#8276 = ORIENTED_EDGE ( 'NONE', *, *, #42192, .T. ) ;
#8277 = ORIENTED_EDGE ( 'NONE', *, *, #46863, .F. ) ;
#8278 = EDGE_CURVE ( 'NONE', #12964, #7991, #27714, .T. ) ;
#8279 = ADVANCED_FACE ( 'NONE', ( #22341 ), #53809, .F. ) ;
#8280 = VECTOR ( 'NONE', #45642, 1000.000000000000227 ) ;
#8281 = VERTEX_POINT ( 'NONE', #1286 ) ;
#8282 = DIRECTION ( 'NONE',  ( 0.7660212471507180654, -0.6427876096865404731, 0.005961354470445141482 ) ) ;
#8283 = CARTESIAN_POINT ( 'NONE',  ( -12.76204334111325700, 0.000000000000000000, 6.398424288781984437 ) ) ;
#8284 = ORIENTED_EDGE ( 'NONE', *, *, #40489, .T. ) ;
#8285 = CARTESIAN_POINT ( 'NONE',  ( -58.00000000000000711, -9.333333333333333925, 7.102951435054649637E-15 ) ) ;
#8286 = VERTEX_POINT ( 'NONE', #744 ) ;
#8287 = CARTESIAN_POINT ( 'NONE',  ( -13.08486533123210194, 0.000000000000000000, 1.963927175729152541 ) ) ;
#8288 = LINE ( 'NONE', #42384, #9509 ) ;
#8289 = VERTEX_POINT ( 'NONE', #18062 ) ;
#8290 = CARTESIAN_POINT ( 'NONE',  ( -15.52211495245506256, 0.000000000000000000, 2.810943005112377158 ) ) ;
#8291 = ORIENTED_EDGE ( 'NONE', *, *, #19449, .F. ) ;
#8292 = EDGE_CURVE ( 'NONE', #21743, #21718, #52685, .T. ) ;
#8293 = LINE ( 'NONE', #8888, #10954 ) ;
#8294 = CARTESIAN_POINT ( 'NONE',  ( -18.67697421479882181, -0.1191753592594197858, 4.036397482078229793 ) ) ;
#8295 = ORIENTED_EDGE ( 'NONE', *, *, #18344, .T. ) ;
#8296 = B_SPLINE_CURVE_WITH_KNOTS ( 'NONE', 3,
 ( #11566, #28883, #46181, #7283 ),
 .UNSPECIFIED., .F., .F.,
 ( 4, 4 ),
 ( 0.000000000000000000, 0.0003349204823136315776 ),
 .UNSPECIFIED. ) ;
#8297 = DIRECTION ( 'NONE',  ( 0.005002170337468016433, -0.7660444431189770143, -0.6427681459581293666 ) ) ;
#8298 = CARTESIAN_POINT ( 'NONE',  ( -14.66887761629205222, 0.000000000000000000, 12.58869632783390990 ) ) ;
#8299 = CARTESIAN_POINT ( 'NONE',  ( -11.20636620717317378, 0.000000000000000000, 11.32298014792380414 ) ) ;
#8300 = ORIENTED_EDGE ( 'NONE', *, *, #50078, .T. ) ;
#8301 = AXIS2_PLACEMENT_3D ( 'NONE', #24329, #41902, #37110 ) ;
#8302 = VECTOR ( 'NONE', #37716, 1000.000000000000227 ) ;
#8303 = DIRECTION ( 'NONE',  ( -0.5364919789714478471, 0.6444004775717705469, -0.5449076811759709926 ) ) ;
#8304 = CARTESIAN_POINT ( 'NONE',  ( -8.476662044498805670, -0.1191753592594181482, 5.962439019012909291 ) ) ;
#8305 = CARTESIAN_POINT ( 'NONE',  ( -9.295220851736454293, 0.000000000000000000, 4.578743553985232140 ) ) ;
#8306 = DIRECTION ( 'NONE',  ( 0.5449076811759707706, 0.6444004775717708799, -0.5364919789714476250 ) ) ;
#8307 = LINE ( 'NONE', #21666, #27942 ) ;
#8308 = DIRECTION ( 'NONE',  ( 0.005961354470445682716, -0.6427876096865404731, -0.7660212471507180654 ) ) ;
#8309 = AXIS2_PLACEMENT_3D ( 'NONE', #37566, #37025, #50891 ) ;
#8310 = ORIENTED_EDGE ( 'NONE', *, *, #39769, .T. ) ;
#8311 = DIRECTION ( 'NONE',  ( 0.000000000000000000, -1.000000000000000000, 0.000000000000000000 ) ) ;
#8312 = DIRECTION ( 'NONE',  ( 0.005961354470445682716, -0.6427876096865404731, -0.7660212471507180654 ) ) ;
#8313 = DIRECTION ( 'NONE',  ( 0.000000000000000000, -0.000000000000000000, -1.000000000000000000 ) ) ;
#8314 = VERTEX_POINT ( 'NONE', #18627 ) ;
#8315 = DIRECTION ( 'NONE',  ( 0.5364919789714477361, 0.6444004775717706579, 0.5449076811759711036 ) ) ;
#8316 = FACE_OUTER_BOUND ( 'NONE', #46071, .T. ) ;
#8317 = ORIENTED_EDGE ( 'NONE', *, *, #36134, .T. ) ;
#8318 = CARTESIAN_POINT ( 'NONE',  ( -9.075990533167328067, 0.000000000000000000, 10.41622904950343909 ) ) ;
#8319 = LINE ( 'NONE', #12865, #23313 ) ;
#8320 = EDGE_CURVE ( 'NONE', #21187, #11287, #5298, .T. ) ;
#8321 = CARTESIAN_POINT ( 'NONE',  ( -23.33693525117809386, 0.000000000000000000, 5.746789908705562944 ) ) ;
#8322 = VECTOR ( 'NONE', #16672, 999.9999999999998863 ) ;
#8323 = CARTESIAN_POINT ( 'NONE',  ( -65.89105554006435739, 1.999999999999976685, 3.962576710808226377 ) ) ;
#8324 = ORIENTED_EDGE ( 'NONE', *, *, #38680, .T. ) ;
#8325 = EDGE_LOOP ( 'NONE', ( #15393, #45057, #35257, #5569 ) ) ;
#8326 = CARTESIAN_POINT ( 'NONE',  ( -67.91322597425605068, -0.6009552942202146530, 4.584835828370202648 ) ) ;
#8327 = CARTESIAN_POINT ( 'NONE',  ( -20.77325648630311150, -3.108426967578157729, 9.852428232502697725 ) ) ;
#8328 = DIRECTION ( 'NONE',  ( 0.007781995580012662783, 0.000000000000000000, -0.9999697198139514409 ) ) ;
#8329 = EDGE_CURVE ( 'NONE', #23836, #3819, #14095, .T. ) ;
#8330 = LINE ( 'NONE', #39839, #20233 ) ;
#8331 = FACE_OUTER_BOUND ( 'NONE', #14888, .T. ) ;
#8332 = LINE ( 'NONE', #50918, #54837 ) ;
#8334 = EDGE_CURVE ( 'NONE', #29513, #12044, #9840, .T. ) ;
#8333 = EDGE_LOOP ( 'NONE', ( #38836, #3214, #53226, #34597, #48275, #21251, #1697, #31551 ) ) ;
#8335 = LINE ( 'NONE', #46680, #24699 ) ;
#8336 = EDGE_CURVE ( 'NONE', #24506, #8726, #48997, .T. ) ;
#8337 = DIRECTION ( 'NONE',  ( 0.5449076811759707706, 0.6444004775717708799, -0.5364919789714476250 ) ) ;
#8338 = ORIENTED_EDGE ( 'NONE', *, *, #15832, .T. ) ;
#8339 = LINE ( 'NONE', #52615, #13856 ) ;
#8340 = EDGE_CURVE ( 'NONE', #6097, #45628, #44452, .T. ) ;
#8341 = LINE ( 'NONE', #38443, #44064 ) ;
#8342 = DIRECTION ( 'NONE',  ( -0.9999697198139514409, -0.000000000000000000, -0.007781995580013368816 ) ) ;
#8343 = EDGE_LOOP ( 'NONE', ( #3533, #24771, #17697, #15473 ) ) ;
#8344 = VECTOR ( 'NONE', #363, 1000.000000000000114 ) ;
#8345 = VECTOR ( 'NONE', #48166, 1000.000000000000114 ) ;
#8346 = PLANE ( 'NONE',  #15773 ) ;
#8347 = ADVANCED_FACE ( 'NONE', ( #40196 ), #17539, .F. ) ;
#8348 = ORIENTED_EDGE ( 'NONE', *, *, #20952, .T. ) ;
#8349 = EDGE_CURVE ( 'NONE', #15384, #6272, #51886, .T. ) ;
#8350 = ORIENTED_EDGE ( 'NONE', *, *, #55858, .T. ) ;
#8351 = EDGE_LOOP ( 'NONE', ( #34754, #5942, #41855, #26309 ) ) ;
#8352 = VECTOR ( 'NONE', #13613, 999.9999999999998863 ) ;
#8353 = EDGE_LOOP ( 'NONE', ( #9660, #15273, #2319, #4141 ) ) ;
#8354 = FACE_OUTER_BOUND ( 'NONE', #28839, .T. ) ;
#8355 = ORIENTED_EDGE ( 'NONE', *, *, #44825, .F. ) ;
#8356 = CARTESIAN_POINT ( 'NONE',  ( -24.26908309836554878, 0.000000000000000000, 6.108867788427308376 ) ) ;
#8357 = EDGE_CURVE ( 'NONE', #32587, #47105, #4757, .T. ) ;
#8358 = ORIENTED_EDGE ( 'NONE', *, *, #864, .F. ) ;
#8359 = DIRECTION ( 'NONE',  ( 0.7660212471507180654, -0.6427876096865404731, 0.005961354470445141482 ) ) ;
#8360 = ORIENTED_EDGE ( 'NONE', *, *, #3998, .T. ) ;
#8362 = VECTOR ( 'NONE', #43978, 999.9999999999998863 ) ;
#8361 = LINE ( 'NONE', #26811, #43713 ) ;
#8363 = ORIENTED_EDGE ( 'NONE', *, *, #44809, .F. ) ;
#8364 = EDGE_CURVE ( 'NONE', #17269, #38033, #18098, .T. ) ;
#8365 = LINE ( 'NONE', #33934, #51081 ) ;
#8366 = DIRECTION ( 'NONE',  ( 0.007781995580012662783, 0.000000000000000000, -0.9999697198139514409 ) ) ;
#8367 = DIRECTION ( 'NONE',  ( -0.005002170337468016433, -0.7660444431189770143, 0.6427681459581293666 ) ) ;
#8368 = DIRECTION ( 'NONE',  ( 0.000000000000000000, -1.000000000000000000, 0.000000000000000000 ) ) ;
#8369 = DIRECTION ( 'NONE',  ( 0.8531650599175529814, -0.4028455766673920135, -0.3313982828793697877 ) ) ;
#8370 = ORIENTED_EDGE ( 'NONE', *, *, #18167, .F. ) ;
#8371 = EDGE_LOOP ( 'NONE', ( #27481, #28256, #25584, #41917 ) ) ;
#8372 = DIRECTION ( 'NONE',  ( -0.005002170337468016433, -0.7660444431189770143, 0.6427681459581293666 ) ) ;
#8373 = DIRECTION ( 'NONE',  ( -0.6427681459581293666, -0.7660444431189770143, -0.005002170337467561935 ) ) ;
#8374 = VECTOR ( 'NONE', #33051, 999.9999999999998863 ) ;
#8375 = FACE_OUTER_BOUND ( 'NONE', #29807, .T. ) ;
#8376 = LINE ( 'NONE', #2983, #48597 ) ;
#8377 = DIRECTION ( 'NONE',  ( 0.007781995580012663651, -3.146120232559066537E-19, -0.9999697198139514409 ) ) ;
#8378 = PLANE ( 'NONE',  #50407 ) ;
#8379 = ORIENTED_EDGE ( 'NONE', *, *, #53984, .F. ) ;
#8381 = DIRECTION ( 'NONE',  ( 0.9999697198139515519, 0.000000000000000000, 0.007781995580013368816 ) ) ;
#8380 = VECTOR ( 'NONE', #47252, 999.9999999999998863 ) ;
#8382 = CARTESIAN_POINT ( 'NONE',  ( -19.60834386242827776, 0.000000000000000000, 4.298478389818581213 ) ) ;
#8383 = ORIENTED_EDGE ( 'NONE', *, *, #28599, .F. ) ;
#8384 = VECTOR ( 'NONE', #1055, 999.9999999999998863 ) ;
#8385 = VECTOR ( 'NONE', #3123, 1000.000000000000000 ) ;
#8386 = DIRECTION ( 'NONE',  ( 0.000000000000000000, -0.000000000000000000, -1.000000000000000000 ) ) ;
#8387 = CARTESIAN_POINT ( 'NONE',  ( -12.80458192191714595, 0.000000000000000000, 11.86454056839041726 ) ) ;
#8388 = EDGE_CURVE ( 'NONE', #11826, #25841, #34871, .T. ) ;
#8389 = DIRECTION ( 'NONE',  ( 0.005002170337468016433, -0.7660444431189770143, -0.6427681459581293666 ) ) ;
#8390 = LINE ( 'NONE', #43040, #6024 ) ;
#8391 = VERTEX_POINT ( 'NONE', #13303 ) ;
#8392 = AXIS2_PLACEMENT_3D ( 'NONE', #14436, #27475, #40566 ) ;
#8393 = VECTOR ( 'NONE', #36600, 1000.000000000000227 ) ;
#8394 = ORIENTED_EDGE ( 'NONE', *, *, #34056, .T. ) ;
#8395 = DIRECTION ( 'NONE',  ( -0.5449076811759708816, 0.6444004775717707689, 0.5364919789714475140 ) ) ;
#8396 = CARTESIAN_POINT ( 'NONE',  ( -16.06709938707323460, 0.000000000000000000, 13.13181314741652628 ) ) ;
#8397 = CARTESIAN_POINT ( 'NONE',  ( -15.86710544311044302, 0.000000000000000000, 13.13336954653252953 ) ) ;
#8398 = CARTESIAN_POINT ( 'NONE',  ( -12.16789073767994900, -0.1191753592594193972, 2.609724395548954412 ) ) ;
#8399 = VECTOR ( 'NONE', #48691, 999.9999999999998863 ) ;
#8400 = FACE_OUTER_BOUND ( 'NONE', #15587, .T. ) ;
#8401 = CARTESIAN_POINT ( 'NONE',  ( -12.76336099550253600, 0.000000000000000000, 6.567740048076958104 ) ) ;
#8402 = DIRECTION ( 'NONE',  ( 0.000000000000000000, -1.000000000000000000, 0.000000000000000000 ) ) ;
#8404 = ADVANCED_FACE ( 'NONE', ( #35172 ), #43933, .F. ) ;
#8403 = ORIENTED_EDGE ( 'NONE', *, *, #25804, .T. ) ;
#8405 = CARTESIAN_POINT ( 'NONE',  ( -20.54049170961573267, 0.000000000000000000, 4.660556269540326646 ) ) ;
#8406 = CARTESIAN_POINT ( 'NONE',  ( -13.27703486227003893, -3.108426967578160838, 1.939397253021431400 ) ) ;
#8407 = FACE_OUTER_BOUND ( 'NONE', #52557, .T. ) ;
#8408 = ORIENTED_EDGE ( 'NONE', *, *, #24307, .T. ) ;
#8409 = DIRECTION ( 'NONE',  ( 0.6427681459581294776, -0.7660444431189769032, 0.005002170337467562802 ) ) ;
#8410 = ORIENTED_EDGE ( 'NONE', *, *, #15159, .F. ) ;
#8411 = EDGE_CURVE ( 'NONE', #47831, #2828, #21797, .T. ) ;
#8412 = AXIS2_PLACEMENT_3D ( 'NONE', #22463, #35493, #13912 ) ;
#8413 = EDGE_LOOP ( 'NONE', ( #39143, #33989, #4320, #48718 ) ) ;
#8414 = ADVANCED_FACE ( 'NONE', ( #25785 ), #16997, .F. ) ;
#8415 = ORIENTED_EDGE ( 'NONE', *, *, #3840, .F. ) ;
#8416 = ORIENTED_EDGE ( 'NONE', *, *, #15624, .T. ) ;
#8417 = EDGE_LOOP ( 'NONE', ( #21887, #54431, #12401, #47696 ) ) ;
#8418 = VERTEX_POINT ( 'NONE', #43392 ) ;
#8419 = AXIS2_PLACEMENT_3D ( 'NONE', #51071, #15585, #30588 ) ;
#8420 = CARTESIAN_POINT ( 'NONE',  ( -25.20123094555300369, 0.000000000000000000, 6.470945668149052032 ) ) ;
#8421 = PLANE ( 'NONE',  #53797 ) ;
#8422 = CARTESIAN_POINT ( 'NONE',  ( 4.848100717410755323, 0.000000000000000000, -2.162384853247615535 ) ) ;
#8423 = AXIS2_PLACEMENT_3D ( 'NONE', #4996, #733, #22599 ) ;
#8424 = EDGE_CURVE ( 'NONE', #6407, #41644, #30875, .T. ) ;
#8425 = VECTOR ( 'NONE', #31152, 999.9999999999998863 ) ;
#8426 = ORIENTED_EDGE ( 'NONE', *, *, #24722, .F. ) ;
#8427 = LINE ( 'NONE', #13273, #49430 ) ;
#8428 = EDGE_LOOP ( 'NONE', ( #40136, #19229, #6713, #29587 ) ) ;
#8429 = DIRECTION ( 'NONE',  ( 0.000000000000000000, 1.000000000000000000, 0.000000000000000000 ) ) ;
#8430 = EDGE_LOOP ( 'NONE', ( #40416, #24, #53357, #48947 ) ) ;
#8431 = ADVANCED_FACE ( 'NONE', ( #4488 ), #39701, .F. ) ;
#8432 = VECTOR ( 'NONE', #29682, 999.9999999999998863 ) ;
#8433 = VECTOR ( 'NONE', #8844, 999.9999999999998863 ) ;
#8434 = CARTESIAN_POINT ( 'NONE',  ( 2.072287782118878319, 0.000000000000000000, -2.950529333540147015 ) ) ;
#8435 = DIRECTION ( 'NONE',  ( 0.9999697198139515519, 0.000000000000000000, 0.007781995580013368816 ) ) ;
#8436 = DIRECTION ( 'NONE',  ( -0.005961354470445682716, -0.6427876096865404731, 0.7660212471507180654 ) ) ;
#8437 = ORIENTED_EDGE ( 'NONE', *, *, #25767, .T. ) ;
#8438 = PLANE ( 'NONE',  #51887 ) ;
#8439 = EDGE_LOOP ( 'NONE', ( #5470, #19775, #13802, #51372 ) ) ;
#8440 = DIRECTION ( 'NONE',  ( -0.5449076811759708816, 0.6444004775717707689, 0.5364919789714475140 ) ) ;
#8441 = FACE_OUTER_BOUND ( 'NONE', #39149, .T. ) ;
#8442 = VECTOR ( 'NONE', #18637, 999.9999999999998863 ) ;
#8443 = FACE_OUTER_BOUND ( 'NONE', #34123, .T. ) ;
#8444 = LINE ( 'NONE', #3049, #2285 ) ;
#8445 = DIRECTION ( 'NONE',  ( 0.000000000000000000, -0.000000000000000000, -1.000000000000000000 ) ) ;
#8446 = DIRECTION ( 'NONE',  ( 0.7660212471507180654, -0.6427876096865404731, 0.005961354470445141482 ) ) ;
#8447 = CARTESIAN_POINT ( 'NONE',  ( -18.87699506648361947, 1.743523803501505709, 7.075206662320437268 ) ) ;
#8448 = CARTESIAN_POINT ( 'NONE',  ( -70.12381838982661009, -8.729438269679169693, -8.047023921085742160 ) ) ;
#8449 = ORIENTED_EDGE ( 'NONE', *, *, #734, .F. ) ;
#8450 = DIRECTION ( 'NONE',  ( 0.9999697198139515519, 0.000000000000000000, 0.007781995580013368816 ) ) ;
#8451 = ORIENTED_EDGE ( 'NONE', *, *, #49248, .T. ) ;
#8452 = ADVANCED_FACE ( 'NONE', ( #9291 ), #47348, .F. ) ;
#8453 = VECTOR ( 'NONE', #15682, 1000.000000000000114 ) ;
#8454 = DIRECTION ( 'NONE',  ( 0.9999697198139515519, 0.000000000000000000, 0.007781995580013368816 ) ) ;
#8455 = CARTESIAN_POINT ( 'NONE',  ( 2.072287782118878319, 0.000000000000000000, -2.950529333540147015 ) ) ;
#8456 = DIRECTION ( 'NONE',  ( 0.7660212471507180654, -0.6427876096865404731, 0.005961354470445141482 ) ) ;
#8457 = EDGE_CURVE ( 'NONE', #14391, #45314, #39116, .T. ) ;
#8458 = VECTOR ( 'NONE', #55685, 1000.000000000000227 ) ;
#8459 = CARTESIAN_POINT ( 'NONE',  ( -19.27402565828830205, 0.000000000000000000, 7.255736689840353471 ) ) ;
#8460 = DIRECTION ( 'NONE',  ( -0.5364919789714478471, 0.6444004775717705469, -0.5449076811759709926 ) ) ;
#8461 = DIRECTION ( 'NONE',  ( 0.9999697198139515519, 0.000000000000000000, 0.007781995580013368816 ) ) ;
#8462 = LINE ( 'NONE', #9296, #13935 ) ;
#8463 = ORIENTED_EDGE ( 'NONE', *, *, #8464, .T. ) ;
#8464 = EDGE_CURVE ( 'NONE', #25146, #26810, #30043, .T. ) ;
#8465 = VECTOR ( 'NONE', #38160, 999.9999999999998863 ) ;
#8466 = CARTESIAN_POINT ( 'NONE',  ( -19.36956794502930634, 19.74319977116263303, 4.294846203288412489 ) ) ;
#8467 = CARTESIAN_POINT ( 'NONE',  ( -12.28749583716221316, -3.594132820645663084, 1.539530131120636858 ) ) ;
#8468 = CARTESIAN_POINT ( 'NONE',  ( -10.94028622754223967, 0.000000000000000000, 11.14038480894692995 ) ) ;
#8469 = EDGE_CURVE ( 'NONE', #4723, #36189, #31156, .T. ) ;
#8470 = ADVANCED_FACE ( 'NONE', ( #25494 ), #42801, .F. ) ;
#8471 = EDGE_CURVE ( 'NONE', #7098, #19098, #55895, .T. ) ;
#8472 = VECTOR ( 'NONE', #10334, 1000.000000000000227 ) ;
#8473 = VECTOR ( 'NONE', #22453, 1000.000000000000114 ) ;
#8474 = DIRECTION ( 'NONE',  ( 0.9999697198139515519, 0.000000000000000000, 0.007781995580013368816 ) ) ;
#8475 = DIRECTION ( 'NONE',  ( 0.000000000000000000, 0.000000000000000000, -1.000000000000000000 ) ) ;
#8476 = FACE_OUTER_BOUND ( 'NONE', #28182, .T. ) ;
#8477 = LINE ( 'NONE', #48197, #7486 ) ;
#8478 = ORIENTED_EDGE ( 'NONE', *, *, #18011, .F. ) ;
#8479 = VECTOR ( 'NONE', #25897, 999.9999999999998863 ) ;
#8480 = CARTESIAN_POINT ( 'NONE',  ( -23.33849165029409889, 0.000000000000000000, 5.946783852668351855 ) ) ;
#8481 = VECTOR ( 'NONE', #18376, 999.9999999999998863 ) ;
#8482 = CARTESIAN_POINT ( 'NONE',  ( -14.66887761629205222, 0.000000000000000000, 12.58869632783390990 ) ) ;
#8483 = ORIENTED_EDGE ( 'NONE', *, *, #37229, .F. ) ;
#8484 = VERTEX_POINT ( 'NONE', #51620 ) ;
#8485 = CARTESIAN_POINT ( 'NONE',  ( -19.07271405993623503, 0.000000000000000000, 7.087977329661382164 ) ) ;
#8486 = ORIENTED_EDGE ( 'NONE', *, *, #25176, .F. ) ;
#8487 = EDGE_CURVE ( 'NONE', #56078, #51473, #56166, .T. ) ;
#8488 = EDGE_CURVE ( 'NONE', #37937, #55170, #36273, .T. ) ;
#8489 = ORIENTED_EDGE ( 'NONE', *, *, #1132, .T. ) ;
#8490 = ORIENTED_EDGE ( 'NONE', *, *, #16918, .T. ) ;
#8491 = ORIENTED_EDGE ( 'NONE', *, *, #49208, .T. ) ;
#8492 = AXIS2_PLACEMENT_3D ( 'NONE', #35328, #52625, #40129 ) ;
#8493 = ADVANCED_FACE ( 'NONE', ( #22920 ), #27455, .F. ) ;
#8494 = DIRECTION ( 'NONE',  ( 0.6246952433987894571, -0.7422098413412800966, -0.2426528472758541777 ) ) ;
#8495 = ORIENTED_EDGE ( 'NONE', *, *, #18531, .T. ) ;
#8496 = DIRECTION ( 'NONE',  ( 0.9659258262890682012, -0.2588190451025213501, 0.000000000000000000 ) ) ;
#8497 = LINE ( 'NONE', #4518, #10382 ) ;
#8498 = VECTOR ( 'NONE', #44826, 999.9999999999998863 ) ;
#8499 = ADVANCED_FACE ( 'NONE', ( #40241 ), #5895, .F. ) ;
#8500 = EDGE_LOOP ( 'NONE', ( #55471, #4414, #41927, #18713 ) ) ;
#8501 = ORIENTED_EDGE ( 'NONE', *, *, #25648, .T. ) ;
#8502 = VECTOR ( 'NONE', #16442, 1000.000000000000227 ) ;
#8503 = ADVANCED_FACE ( 'NONE', ( #53025 ), #36533, .F. ) ;
#8504 = CARTESIAN_POINT ( 'NONE',  ( -49.27554558092695913, 2.476975532698160620, 5.000000000000000000 ) ) ;
#8505 = EDGE_LOOP ( 'NONE', ( #49915, #42704, #29212, #51509 ) ) ;
#8506 = VECTOR ( 'NONE', #54551, 1000.000000000000227 ) ;
#8507 = DIRECTION ( 'NONE',  ( -0.5364919789714478471, 0.6444004775717705469, -0.5449076811759709926 ) ) ;
#8508 = DIRECTION ( 'NONE',  ( -0.9999697198139514409, -0.000000000000000000, -0.007781995580013368816 ) ) ;
#8509 = EDGE_LOOP ( 'NONE', ( #42846, #33146, #48883, #54111 ) ) ;
#8510 = CARTESIAN_POINT ( 'NONE',  ( -21.47263955680318404, 0.000000000000000000, 5.022634149262071190 ) ) ;
#8511 = AXIS2_PLACEMENT_3D ( 'NONE', #1091, #52514, #31780 ) ;
#8512 = ORIENTED_EDGE ( 'NONE', *, *, #39081, .F. ) ;
#8513 = CARTESIAN_POINT ( 'NONE',  ( -21.47341775636118655, -0.1191753592594197858, 5.122631121243466090 ) ) ;
#8514 = AXIS2_PLACEMENT_3D ( 'NONE', #38301, #22615, #16435 ) ;
#8515 = DIRECTION ( 'NONE',  ( 0.5364919789714477361, 0.6444004775717706579, 0.5449076811759711036 ) ) ;
#8516 = VECTOR ( 'NONE', #51290, 1000.000000000000227 ) ;
#8517 = ORIENTED_EDGE ( 'NONE', *, *, #38534, .T. ) ;
#8518 = DIRECTION ( 'NONE',  ( 0.9999697198139515519, 0.000000000000000000, 0.007781995580013368816 ) ) ;
#8519 = DIRECTION ( 'NONE',  ( 0.9999697198139515519, 0.000000000000000000, 0.007781995580013368816 ) ) ;
#8520 = CARTESIAN_POINT ( 'NONE',  ( -12.10603466082523028, 0.000000000000000000, 7.511525709439289322 ) ) ;
#8521 = CARTESIAN_POINT ( 'NONE',  ( -16.89925026227929195, -0.1191753592594197858, 13.49466922669627422 ) ) ;
#8522 = ORIENTED_EDGE ( 'NONE', *, *, #8870, .F. ) ;
#8523 = DIRECTION ( 'NONE',  ( 0.9999697198139515519, 0.000000000000000000, 0.007781995580013368816 ) ) ;
#8524 = CARTESIAN_POINT ( 'NONE',  ( -18.79527752321125789, 2.229229656569007734, 3.911531714474451249 ) ) ;
#8525 = CARTESIAN_POINT ( 'NONE',  ( -15.10787738939381519, -0.8417996532631553119, 3.931881018872667166 ) ) ;
#8526 = DIRECTION ( 'NONE',  ( 0.007781995580012663651, -3.146120232559066537E-19, -0.9999697198139514409 ) ) ;
#8527 = DIRECTION ( 'NONE',  ( 0.9999697198139515519, 0.000000000000000000, 0.007781995580013368816 ) ) ;
#8528 = CARTESIAN_POINT ( 'NONE',  ( -14.43053679941993650, 0.000000000000000000, 7.662761909894217460 ) ) ;
#8529 = FACE_OUTER_BOUND ( 'NONE', #11270, .T. ) ;
#8530 = LINE ( 'NONE', #39480, #8473 ) ;
#8531 = CARTESIAN_POINT ( 'NONE',  ( -20.54204810873173415, 0.000000000000000000, 4.860550213503115558 ) ) ;
#8532 = VECTOR ( 'NONE', #25668, 999.9999999999998863 ) ;
#8533 = VERTEX_POINT ( 'NONE', #15252 ) ;
#8534 = CARTESIAN_POINT ( 'NONE',  ( 0.000000000000000000, 0.000000000000000000, 0.000000000000000000 ) ) ;
#8535 = LINE ( 'NONE', #48557, #9689 ) ;
#8536 = ORIENTED_EDGE ( 'NONE', *, *, #54787, .F. ) ;
#8537 = DIRECTION ( 'NONE',  ( 0.005961354470445682716, -0.6427876096865404731, -0.7660212471507180654 ) ) ;
#8538 = DIRECTION ( 'NONE',  ( 0.005002170337468016433, -0.7660444431189770143, -0.6427681459581293666 ) ) ;
#8539 = VECTOR ( 'NONE', #13490, 1000.000000000000227 ) ;
#8540 = EDGE_CURVE ( 'NONE', #52907, #46963, #5597, .T. ) ;
#8541 = ADVANCED_FACE ( 'NONE', ( #36841 ), #18954, .F. ) ;
#8542 = PLANE ( 'NONE',  #13730 ) ;
#8543 = AXIS2_PLACEMENT_3D ( 'NONE', #33097, #50417, #6698 ) ;
#8544 = ADVANCED_FACE ( 'NONE', ( #45083 ), #1331, .F. ) ;
#8545 = DIRECTION ( 'NONE',  ( 0.5364919789714477361, 0.6444004775717706579, 0.5449076811759711036 ) ) ;
#8546 = FACE_OUTER_BOUND ( 'NONE', #7173, .T. ) ;
#8547 = VERTEX_POINT ( 'NONE', #6187 ) ;
#8548 = ORIENTED_EDGE ( 'NONE', *, *, #49689, .F. ) ;
#8549 = CARTESIAN_POINT ( 'NONE',  ( -9.778419723998514002, 0.000000000000000000, 6.960301621058782473 ) ) ;
#8550 = VECTOR ( 'NONE', #17719, 999.9999999999998863 ) ;
#8551 = LINE ( 'NONE', #29857, #25896 ) ;
#8552 = ORIENTED_EDGE ( 'NONE', *, *, #20658, .T. ) ;
#8553 = AXIS2_PLACEMENT_3D ( 'NONE', #47200, #26456, #3759 ) ;
#8554 = DIRECTION ( 'NONE',  ( 0.005002170337468016433, -0.7660444431189770143, -0.6427681459581293666 ) ) ;
#8555 = EDGE_LOOP ( 'NONE', ( #54942, #44710, #47319, #46606, #24688, #25642, #25519, #9963, #53675, #22278, #47759, #29937, #5388, #20429, #42126, #40703, #32041, #55171, #55584, #5591, #31627, #32561, #27281, #4628, #12436, #50794, #27262 ) ) ;
#8556 = DIRECTION ( 'NONE',  ( 0.7660212471507180654, -0.6427876096865404731, 0.005961354470445141482 ) ) ;
#8557 = ORIENTED_EDGE ( 'NONE', *, *, #28084, .F. ) ;
#8558 = LINE ( 'NONE', #25890, #34729 ) ;
#8559 = EDGE_CURVE ( 'NONE', #49125, #593, #53326, .T. ) ;
#8560 = AXIS2_PLACEMENT_3D ( 'NONE', #13842, #9303, #27196 ) ;
#8561 = ORIENTED_EDGE ( 'NONE', *, *, #13361, .T. ) ;
#8562 = VECTOR ( 'NONE', #56184, 1000.000000000000114 ) ;
#8563 = ORIENTED_EDGE ( 'NONE', *, *, #21234, .F. ) ;
#8564 = ORIENTED_EDGE ( 'NONE', *, *, #50679, .F. ) ;
#8565 = DIRECTION ( 'NONE',  ( -0.5364919789714478471, 0.6444004775717705469, -0.5449076811759709926 ) ) ;
#8566 = DIRECTION ( 'NONE',  ( 0.000000000000000000, -0.000000000000000000, -1.000000000000000000 ) ) ;
#8567 = LINE ( 'NONE', #25900, #26655 ) ;
#8568 = EDGE_CURVE ( 'NONE', #39978, #45002, #19495, .T. ) ;
#8569 = DIRECTION ( 'NONE',  ( 0.6427681459581294776, -0.7660444431189769032, 0.005002170337467562802 ) ) ;
#8570 = ORIENTED_EDGE ( 'NONE', *, *, #14136, .T. ) ;
#8571 = EDGE_LOOP ( 'NONE', ( #29218, #19174, #41864, #7236 ) ) ;
#8572 = EDGE_CURVE ( 'NONE', #11724, #40325, #23490, .T. ) ;
#8573 = VECTOR ( 'NONE', #42169, 1000.000000000000000 ) ;
#8574 = ORIENTED_EDGE ( 'NONE', *, *, #38534, .F. ) ;
#8575 = EDGE_CURVE ( 'NONE', #42504, #16374, #40806, .T. ) ;
#8576 = DIRECTION ( 'NONE',  ( 0.005961354470445682716, -0.6427876096865404731, -0.7660212471507180654 ) ) ;
#8577 = VECTOR ( 'NONE', #14259, 1000.000000000000114 ) ;
#8578 = ORIENTED_EDGE ( 'NONE', *, *, #24544, .F. ) ;
#8579 = DIRECTION ( 'NONE',  ( -0.005002170337468016433, -0.7660444431189770143, 0.6427681459581293666 ) ) ;
#8580 = EDGE_CURVE ( 'NONE', #22414, #44511, #5336, .T. ) ;
#8581 = ORIENTED_EDGE ( 'NONE', *, *, #49039, .F. ) ;
#8582 = VECTOR ( 'NONE', #26679, 1000.000000000000227 ) ;
#8583 = CARTESIAN_POINT ( 'NONE',  ( -16.06709938707323460, 0.000000000000000000, 13.13181314741652628 ) ) ;
#8584 = CARTESIAN_POINT ( 'NONE',  ( -16.81190032086591302, 0.000000000000000000, 3.212244750653343583 ) ) ;
#8585 = ORIENTED_EDGE ( 'NONE', *, *, #20410, .F. ) ;
#8586 = ADVANCED_FACE ( 'NONE', ( #10724 ), #49034, .F. ) ;
#8587 = DIRECTION ( 'NONE',  ( -0.005002170337468016433, -0.7660444431189770143, 0.6427681459581293666 ) ) ;
#8588 = EDGE_LOOP ( 'NONE', ( #14549, #49847, #50979, #28258 ) ) ;
#8589 = CARTESIAN_POINT ( 'NONE',  ( -12.66126816957386225, -0.1191753592594177180, 6.299205516358588497 ) ) ;
#8590 = VECTOR ( 'NONE', #23737, 1000.000000000000114 ) ;
#8591 = EDGE_LOOP ( 'NONE', ( #52626, #52815, #16821, #39420 ) ) ;
#8592 = PLANE ( 'NONE',  #55852 ) ;
#8593 = DIRECTION ( 'NONE',  ( -0.5364919789714478471, 0.6444004775717705469, -0.5449076811759709926 ) ) ;
#8594 = AXIS2_PLACEMENT_3D ( 'NONE', #41104, #5622, #22950 ) ;
#8595 = DIRECTION ( 'NONE',  ( 0.005961354470445682716, -0.6427876096865404731, -0.7660212471507180654 ) ) ;
#8596 = VERTEX_POINT ( 'NONE', #39956 ) ;
#8597 = VECTOR ( 'NONE', #24245, 999.9999999999998863 ) ;
#8598 = CARTESIAN_POINT ( 'NONE',  ( -17.21925308359982409, -4.403642575758160760, 10.59760208803285408 ) ) ;
#8599 = PLANE ( 'NONE',  #40086 ) ;
#8600 = LINE ( 'NONE', #17675, #34895 ) ;
#8601 = DIRECTION ( 'NONE',  ( 0.007781995580012663651, -3.146120232559066537E-19, -0.9999697198139514409 ) ) ;
#8602 = FACE_OUTER_BOUND ( 'NONE', #46917, .T. ) ;
#8603 = DIRECTION ( 'NONE',  ( 0.5449076811759707706, 0.6444004775717708799, -0.5364919789714476250 ) ) ;
#8604 = VECTOR ( 'NONE', #138, 999.9999999999998863 ) ;
#8605 = VECTOR ( 'NONE', #3827, 1000.000000000000227 ) ;
#8606 = LINE ( 'NONE', #38979, #4986 ) ;
#8607 = VERTEX_POINT ( 'NONE', #18369 ) ;
#8608 = DIRECTION ( 'NONE',  ( 0.000000000000000000, -0.000000000000000000, -1.000000000000000000 ) ) ;
#8609 = CARTESIAN_POINT ( 'NONE',  ( -18.60520310958986911, 0.000000000000000000, 6.722283538171627271 ) ) ;
#8610 = LINE ( 'NONE', #25942, #45909 ) ;
#8611 = ORIENTED_EDGE ( 'NONE', *, *, #40090, .T. ) ;
#8612 = LINE ( 'NONE', #25944, #18397 ) ;
#8613 = LINE ( 'NONE', #53, #5956 ) ;
#8614 = ORIENTED_EDGE ( 'NONE', *, *, #19636, .F. ) ;
#8615 = ADVANCED_FACE ( 'NONE', ( #10137 ), #1041, .F. ) ;
#8616 = DIRECTION ( 'NONE',  ( -0.7660212471507179544, -0.6427876096865405842, -0.005961354470445141482 ) ) ;
#8617 = EDGE_CURVE ( 'NONE', #29855, #9917, #27180, .T. ) ;
#8618 = EDGE_CURVE ( 'NONE', #38231, #40568, #49868, .T. ) ;
#8619 = PLANE ( 'NONE',  #43233 ) ;
#8620 = CARTESIAN_POINT ( 'NONE',  ( -68.46813845749102256, 2.000000000003206324, 5.359670781636787673 ) ) ;
#8621 = VECTOR ( 'NONE', #14224, 999.9999999999998863 ) ;
#8622 = EDGE_LOOP ( 'NONE', ( #43415, #40654, #49427, #31594 ) ) ;
#8623 = ORIENTED_EDGE ( 'NONE', *, *, #42193, .T. ) ;
#8624 = VECTOR ( 'NONE', #24911, 1000.000000000000114 ) ;
#8625 = LINE ( 'NONE', #33897, #43940 ) ;
#8626 = CARTESIAN_POINT ( 'NONE',  ( -16.82575592011193422, -0.1191753592594187450, 4.050804090899914556 ) ) ;
#8627 = CARTESIAN_POINT ( 'NONE',  ( -16.57549827929610942, -1.489407457353159048, 3.272287659357408618 ) ) ;
#8628 = AXIS2_PLACEMENT_3D ( 'NONE', #35099, #16929, #21469 ) ;
#8629 = CARTESIAN_POINT ( 'NONE',  ( -12.96689773671041124, -0.5179957512181551094, 2.568834445894457197 ) ) ;
#8630 = DIRECTION ( 'NONE',  ( -0.9999697198139514409, -0.000000000000000000, -0.007781995580013368816 ) ) ;
#8631 = CARTESIAN_POINT ( 'NONE',  ( -15.86710544311044302, 0.000000000000000000, 13.13336954653252953 ) ) ;
#8632 = AXIS2_PLACEMENT_3D ( 'NONE', #42862, #51106, #16753 ) ;
#8633 = ORIENTED_EDGE ( 'NONE', *, *, #17150, .T. ) ;
#8634 = DIRECTION ( 'NONE',  ( 0.5364919789714477361, 0.6444004775717706579, 0.5449076811759711036 ) ) ;
#8635 = EDGE_CURVE ( 'NONE', #18328, #15829, #7546, .T. ) ;
#8636 = DIRECTION ( 'NONE',  ( 0.005961354470445682716, -0.6427876096865404731, -0.7660212471507180654 ) ) ;
#8637 = VECTOR ( 'NONE', #55056, 1000.000000000000114 ) ;
#8639 = VERTEX_POINT ( 'NONE', #11251 ) ;
#8638 = VECTOR ( 'NONE', #27370, 999.9999999999998863 ) ;
#8640 = VECTOR ( 'NONE', #49745, 1000.000000000000227 ) ;
#8641 = FACE_OUTER_BOUND ( 'NONE', #31850, .T. ) ;
#8642 = CARTESIAN_POINT ( 'NONE',  ( -25.83279121425626812, 17.74370688441070953, 4.657440554554202805 ) ) ;
#8643 = LINE ( 'NONE', #34466, #33881 ) ;
#8644 = VECTOR ( 'NONE', #54816, 1000.000000000000000 ) ;
#8645 = ORIENTED_EDGE ( 'NONE', *, *, #56069, .T. ) ;
#8646 = CARTESIAN_POINT ( 'NONE',  ( -9.978413667961302025, 0.000000000000000000, 6.958745221942781001 ) ) ;
#8647 = ORIENTED_EDGE ( 'NONE', *, *, #29814, .F. ) ;
#8648 = EDGE_CURVE ( 'NONE', #5931, #43311, #37661, .T. ) ;
#8649 = AXIS2_PLACEMENT_3D ( 'NONE', #17485, #12103, #33980 ) ;
#8650 = ORIENTED_EDGE ( 'NONE', *, *, #18083, .F. ) ;
#8651 = VECTOR ( 'NONE', #56094, 1000.000000000000227 ) ;
#8652 = ORIENTED_EDGE ( 'NONE', *, *, #26573, .F. ) ;
#8653 = EDGE_CURVE ( 'NONE', #45048, #7373, #50442, .T. ) ;
#8654 = ORIENTED_EDGE ( 'NONE', *, *, #54748, .T. ) ;
#8655 = DIRECTION ( 'NONE',  ( -0.5364919789714478471, 0.6444004775717705469, -0.5449076811759709926 ) ) ;
#8656 =( REPRESENTATION_RELATIONSHIP ('NONE','NONE', #51076, #3156 ) REPRESENTATION_RELATIONSHIP_WITH_TRANSFORMATION ( #34577 )SHAPE_REPRESENTATION_RELATIONSHIP( ) );
#8657 = EDGE_LOOP ( 'NONE', ( #14516, #47040, #12647, #45777 ) ) ;
#8658 = CARTESIAN_POINT ( 'NONE',  ( -13.19204130227259952, 23.30979644128433748, -3.679643887444146610 ) ) ;
#8659 = ORIENTED_EDGE ( 'NONE', *, *, #46405, .F. ) ;
#8660 = FACE_OUTER_BOUND ( 'NONE', #8351, .T. ) ;
#8661 = ADVANCED_FACE ( 'NONE', ( #46165 ), #29121, .F. ) ;
#8662 = EDGE_LOOP ( 'NONE', ( #33918, #34280, #11078, #53494 ) ) ;
#8663 = CARTESIAN_POINT ( 'NONE',  ( -15.88130887279446490, 0.000000000000000000, 3.050160814894388839 ) ) ;
#8664 = EDGE_LOOP ( 'NONE', ( #46053, #34172, #25975, #6755 ) ) ;
#8665 = VECTOR ( 'NONE', #7865, 1000.000000000000227 ) ;
#8666 = CARTESIAN_POINT ( 'NONE',  ( -23.33771345073609638, -0.1191753592594197858, 5.846786880686956955 ) ) ;
#8667 = AXIS2_PLACEMENT_3D ( 'NONE', #283, #43464, #16788 ) ;
#8668 = CARTESIAN_POINT ( 'NONE',  ( -19.45503627000849889, 0.000000000000000000, 7.556996783084074742 ) ) ;
#8669 = CARTESIAN_POINT ( 'NONE',  ( -12.99007897266819889, -5.536956232915667186, 1.750451042126190737 ) ) ;
#8670 = FACE_OUTER_BOUND ( 'NONE', #25400, .T. ) ;
#8671 = PLANE ( 'NONE',  #42847 ) ;
#8672 = AXIS2_PLACEMENT_3D ( 'NONE', #11540, #15775, #49862 ) ;
#8673 = ORIENTED_EDGE ( 'NONE', *, *, #55119, .F. ) ;
#8674 = EDGE_CURVE ( 'NONE', #50858, #45180, #46535, .T. ) ;
#8675 = ORIENTED_EDGE ( 'NONE', *, *, #46672, .F. ) ;
#8676 = CARTESIAN_POINT ( 'NONE',  ( -7.074322581158991596, -1.816507792529950871, 8.780998638722685712 ) ) ;
#8677 = LINE ( 'NONE', #43853, #29413 ) ;
#8678 = AXIS2_PLACEMENT_3D ( 'NONE', #56155, #31146, #35412 ) ;
#8679 = ADVANCED_FACE ( 'NONE', ( #7268 ), #50972, .F. ) ;
#8680 = EDGE_CURVE ( 'NONE', #53576, #11173, #24575, .T. ) ;
#8681 = CARTESIAN_POINT ( 'NONE',  ( -62.23823698199103660, 6.658783344088824663, 3.000000000000000000 ) ) ;
#8682 = VECTOR ( 'NONE', #55102, 999.9999999999998863 ) ;
#8683 = VECTOR ( 'NONE', #12123, 1000.000000000000114 ) ;
#8684 = CARTESIAN_POINT ( 'NONE',  ( -10.67188722122801892, 0.000000000000000000, 2.352037599134615409 ) ) ;
#8685 = CARTESIAN_POINT ( 'NONE',  ( -14.40047860997783147, 0.000000000000000000, 3.800349118021597583 ) ) ;
#8686 = DIRECTION ( 'NONE',  ( -0.5364919789714478471, 0.6444004775717705469, -0.5449076811759709926 ) ) ;
#8687 = VERTEX_POINT ( 'NONE', #28287 ) ;
#8688 = DIRECTION ( 'NONE',  ( 0.007781995580012663651, 0.000000000000000000, -0.9999697198139515519 ) ) ;
#8689 = ADVANCED_FACE ( 'NONE', ( #3571 ), #20630, .F. ) ;
#8690 = DIRECTION ( 'NONE',  ( 0.005002170337468016433, -0.7660444431189770143, -0.6427681459581293666 ) ) ;
#8691 = ORIENTED_EDGE ( 'NONE', *, *, #41234, .T. ) ;
#8692 = VECTOR ( 'NONE', #8460, 1000.000000000000000 ) ;
#8693 = CARTESIAN_POINT ( 'NONE',  ( -14.20280369269832832, 0.000000000000000000, 12.40765738797303719 ) ) ;
#8694 = LINE ( 'NONE', #17192, #10635 ) ;
#8695 = VECTOR ( 'NONE', #28179, 999.9999999999998863 ) ;
#8696 = EDGE_CURVE ( 'NONE', #23033, #2866, #20878, .T. ) ;
#8697 = VECTOR ( 'NONE', #519, 1000.000000000000227 ) ;
#8698 = LINE ( 'NONE', #51564, #11429 ) ;
#8699 = ADVANCED_FACE ( 'NONE', ( #41892 ), #46737, .F. ) ;
#8700 = FACE_OUTER_BOUND ( 'NONE', #27072, .T. ) ;
#8701 = AXIS2_PLACEMENT_3D ( 'NONE', #20278, #54937, #50927 ) ;
#8702 = ORIENTED_EDGE ( 'NONE', *, *, #21580, .F. ) ;
#8703 = VECTOR ( 'NONE', #20811, 1000.000000000000114 ) ;
#8704 = VERTEX_POINT ( 'NONE', #25175 ) ;
#8705 = FACE_OUTER_BOUND ( 'NONE', #23367, .T. ) ;
#8706 = CARTESIAN_POINT ( 'NONE',  ( -22.65298538027628794, 19.57956863862976249, -4.449819841089008854 ) ) ;
#8707 = DIRECTION ( 'NONE',  ( 0.5449076811759707706, 0.6444004775717708799, -0.5364919789714476250 ) ) ;
#8708 = ADVANCED_FACE ( 'NONE', ( #38200 ), #42483, .F. ) ;
#8709 = LINE ( 'NONE', #35116, #20978 ) ;
#8710 = CARTESIAN_POINT ( 'NONE',  ( -13.07066190154808361, 0.000000000000000000, 12.04713590736729678 ) ) ;
#8711 = DIRECTION ( 'NONE',  ( -0.1139275668495183386, 0.9934890585767658377, 4.694855797473113547E-16 ) ) ;
#8712 = CARTESIAN_POINT ( 'NONE',  ( -8.456006654281710055, -0.1191753592594182315, 5.223935624422267665 ) ) ;
#8713 = VERTEX_POINT ( 'NONE', #2992 ) ;
#8714 = VECTOR ( 'NONE', #19913, 999.9999999999998863 ) ;
#8715 = EDGE_CURVE ( 'NONE', #6448, #22624, #20323, .T. ) ;
#8716 = PLANE ( 'NONE',  #39554 ) ;
#8717 = CARTESIAN_POINT ( 'NONE',  ( -14.61616047585631151, 0.000000000000000000, 5.814656994489392439 ) ) ;
#8718 = VECTOR ( 'NONE', #44570, 1000.000000000000227 ) ;
#8719 = EDGE_LOOP ( 'NONE', ( #24315, #30733, #2582, #42175 ) ) ;
#8720 = DIRECTION ( 'NONE',  ( 0.005002170337468016433, -0.7660444431189770143, -0.6427681459581293666 ) ) ;
#8721 = ORIENTED_EDGE ( 'NONE', *, *, #30895, .T. ) ;
#8722 = LINE ( 'NONE', #3326, #27704 ) ;
#8723 = VECTOR ( 'NONE', #344, 1000.000000000000227 ) ;
#8724 = ORIENTED_EDGE ( 'NONE', *, *, #3203, .F. ) ;
#8725 = AXIS2_PLACEMENT_3D ( 'NONE', #54815, #6298, #54267 ) ;
#8726 = VERTEX_POINT ( 'NONE', #45605 ) ;
#8727 = ORIENTED_EDGE ( 'NONE', *, *, #12704, .T. ) ;
#8728 = AXIS2_PLACEMENT_3D ( 'NONE', #14003, #5479, #40113 ) ;
#8729 = ORIENTED_EDGE ( 'NONE', *, *, #45254, .F. ) ;
#8730 = VECTOR ( 'NONE', #7833, 1000.000000000000000 ) ;
#8731 = VERTEX_POINT ( 'NONE', #24320 ) ;
#8732 = EDGE_LOOP ( 'NONE', ( #41591, #33045, #42578, #36819 ) ) ;
#8733 = DIRECTION ( 'NONE',  ( 0.007781995580012663651, 0.000000000000000000, -0.9999697198139515519 ) ) ;
#8734 = FACE_OUTER_BOUND ( 'NONE', #1468, .T. ) ;
#8735 = CARTESIAN_POINT ( 'NONE',  ( -18.52672451560416178, -0.1191753592594156363, 9.946879876886450589 ) ) ;
#8736 = VECTOR ( 'NONE', #31084, 1000.000000000000000 ) ;
#8737 = VECTOR ( 'NONE', #2692, 1000.000000000000114 ) ;
#8738 = EDGE_LOOP ( 'NONE', ( #43371, #13469, #16977, #50736 ) ) ;
#8739 = DIRECTION ( 'NONE',  ( -0.005002170337468016433, -0.7660444431189770143, 0.6427681459581293666 ) ) ;
#8740 = EDGE_CURVE ( 'NONE', #54423, #55875, #41627, .T. ) ;
#8741 = ORIENTED_EDGE ( 'NONE', *, *, #19180, .T. ) ;
#8742 = ORIENTED_EDGE ( 'NONE', *, *, #22753, .T. ) ;
#8743 = VECTOR ( 'NONE', #10805, 1000.000000000000227 ) ;
#8744 = VECTOR ( 'NONE', #41895, 1000.000000000000227 ) ;
#8745 = PLANE ( 'NONE',  #5836 ) ;
#8746 = LINE ( 'NONE', #30020, #49547 ) ;
#8747 = ORIENTED_EDGE ( 'NONE', *, *, #29596, .F. ) ;
#8748 = DIRECTION ( 'NONE',  ( 1.000000000000000000, 0.000000000000000000, 0.000000000000000000 ) ) ;
#8749 = ORIENTED_EDGE ( 'NONE', *, *, #28103, .F. ) ;
#8750 = ADVANCED_FACE ( 'NONE', ( #54989 ), #37357, .F. ) ;
#8751 = CARTESIAN_POINT ( 'NONE',  ( -19.12962290826653700, 0.000000000000000000, 14.40064212555863854 ) ) ;
#8752 = DIRECTION ( 'NONE',  ( 0.005961354470445682716, -0.6427876096865404731, -0.7660212471507180654 ) ) ;
#8753 = EDGE_CURVE ( 'NONE', #55515, #23328, #53181, .T. ) ;
#8754 = EDGE_CURVE ( 'NONE', #48148, #53080, #52338, .T. ) ;
#8755 = AXIS2_PLACEMENT_3D ( 'NONE', #43885, #4998, #51835 ) ;
#8756 = DIRECTION ( 'NONE',  ( -0.9321478471874540261, 0.000000000000000000, 0.3620778797217457656 ) ) ;
#8757 = CARTESIAN_POINT ( 'NONE',  ( -15.86710544311044302, 0.000000000000000000, 13.13336954653252953 ) ) ;
#8758 = CARTESIAN_POINT ( 'NONE',  ( 0.3726814890124213187, -6.521129970779321994, -1.535787955176781389E-15 ) ) ;
#8759 = CARTESIAN_POINT ( 'NONE',  ( -17.29614092396359126, -0.1191753592594168992, 4.785807585647434692 ) ) ;
#8760 = DIRECTION ( 'NONE',  ( -0.5364919789714478471, 0.6444004775717705469, -0.5449076811759709926 ) ) ;
#8761 = CARTESIAN_POINT ( 'NONE',  ( -67.08542992444135677, -8.381013491352103273, 2.158836163547856124 ) ) ;
#8762 = EDGE_LOOP ( 'NONE', ( #38245, #27201, #20780, #43137 ) ) ;
#8763 = LINE ( 'NONE', #30624, #27437 ) ;
#8764 = VECTOR ( 'NONE', #17064, 999.9999999999998863 ) ;
#8765 = LINE ( 'NONE', #42541, #51015 ) ;
#8766 = CARTESIAN_POINT ( 'NONE',  ( -23.33771345073609638, -0.1191753592594197858, 5.846786880686956955 ) ) ;
#8767 = EDGE_CURVE ( 'NONE', #43300, #9606, #22518, .T. ) ;
#8769 = CARTESIAN_POINT ( 'NONE',  ( -27.06552663992790997, 0.000000000000000000, 7.195101427592543786 ) ) ;
#8768 = VECTOR ( 'NONE', #18240, 999.9999999999998863 ) ;
#8770 = CARTESIAN_POINT ( 'NONE',  ( -13.47827057769550585, 0.000000000000000000, 4.715516107368122434 ) ) ;
#8771 = PLANE ( 'NONE',  #34956 ) ;
#8772 = ADVANCED_FACE ( 'NONE', ( #26764 ), #48057, .F. ) ;
#8773 = DIRECTION ( 'NONE',  ( 0.000000000000000000, -1.000000000000000000, 0.000000000000000000 ) ) ;
#8774 = VECTOR ( 'NONE', #29722, 999.9999999999998863 ) ;
#8775 = PLANE ( 'NONE',  #4860 ) ;
#8776 = PRODUCT_CONTEXT ( 'NONE', #26081, 'mechanical' ) ;
#8777 = ORIENTED_EDGE ( 'NONE', *, *, #47036, .F. ) ;
#8778 = CARTESIAN_POINT ( 'NONE',  ( -20.04530058363958389, -1.165603555308155626, 6.381161231016116986 ) ) ;
#8779 = CARTESIAN_POINT ( 'NONE',  ( -18.67775241435682432, 0.000000000000000000, 4.136394454059623804 ) ) ;
#8780 = LINE ( 'NONE', #30053, #42689 ) ;
#8781 = ADVANCED_FACE ( 'NONE', ( #1182 ), #27051, .F. ) ;
#8782 = AXIS2_PLACEMENT_3D ( 'NONE', #48955, #43566, #26521 ) ;
#8783 = PLANE ( 'NONE',  #18229 ) ;
#8784 = LINE ( 'NONE', #21248, #24891 ) ;
#8785 = DIRECTION ( 'NONE',  ( 0.007781995580012663651, -3.146120232559066537E-19, -0.9999697198139514409 ) ) ;
#8786 = DIRECTION ( 'NONE',  ( -0.000000000000000000, -0.000000000000000000, 1.000000000000000000 ) ) ;
#8787 = VECTOR ( 'NONE', #9322, 1000.000000000000227 ) ;
#8788 = EDGE_CURVE ( 'NONE', #37046, #54767, #13441, .T. ) ;
#8790 = CARTESIAN_POINT ( 'NONE',  ( -22.40634380310664397, 0.000000000000000000, 5.584705972946605534 ) ) ;
#8789 = AXIS2_PLACEMENT_3D ( 'NONE', #9226, #35360, #4692 ) ;
#8791 = CARTESIAN_POINT ( 'NONE',  ( -10.74029228357944987, 0.000000000000000000, 11.14194120806293320 ) ) ;
#8792 = ORIENTED_EDGE ( 'NONE', *, *, #13650, .T. ) ;
#8793 = DIRECTION ( 'NONE',  ( -0.5449076811759708816, 0.6444004775717707689, 0.5364919789714475140 ) ) ;
#8794 = ORIENTED_EDGE ( 'NONE', *, *, #38562, .T. ) ;
#8795 = VECTOR ( 'NONE', #48834, 1000.000000000000227 ) ;
#8796 = ORIENTED_EDGE ( 'NONE', *, *, #12125, .T. ) ;
#8797 = ORIENTED_EDGE ( 'NONE', *, *, #45589, .F. ) ;
#8798 = ORIENTED_EDGE ( 'NONE', *, *, #15832, .F. ) ;
#8799 = ORIENTED_EDGE ( 'NONE', *, *, #24102, .T. ) ;
#8800 = DIRECTION ( 'NONE',  ( 0.5364919789714477361, 0.6444004775717706579, 0.5449076811759711036 ) ) ;
#8801 = DIRECTION ( 'NONE',  ( 0.000000000000000000, -1.000000000000000000, 0.000000000000000000 ) ) ;
#8802 = AXIS2_PLACEMENT_3D ( 'NONE', #33977, #37956, #51299 ) ;
#8803 = VERTEX_POINT ( 'NONE', #39825 ) ;
#8804 = EDGE_CURVE ( 'NONE', #3505, #30407, #25429, .T. ) ;
#8805 = AXIS2_PLACEMENT_3D ( 'NONE', #9944, #845, #47505 ) ;
#8806 = ADVANCED_FACE ( 'NONE', ( #348 ), #4904, .F. ) ;
#8807 = CARTESIAN_POINT ( 'NONE',  ( -15.86710544311044302, 0.000000000000000000, 13.13336954653252953 ) ) ;
#8809 = EDGE_CURVE ( 'NONE', #53459, #16329, #30715, .T. ) ;
#8808 = ORIENTED_EDGE ( 'NONE', *, *, #36036, .F. ) ;
#8810 = CARTESIAN_POINT ( 'NONE',  ( -16.75527768274136875, 0.000000000000000000, 7.844676295016960843 ) ) ;
#8811 = CARTESIAN_POINT ( 'NONE',  ( -19.33760068587298164, 21.49370688441072019, -4.657437592157546824 ) ) ;
#8812 = ORIENTED_EDGE ( 'NONE', *, *, #28786, .F. ) ;
#8813 = CARTESIAN_POINT ( 'NONE',  ( -10.74029228357944987, 0.000000000000000000, 11.14194120806293320 ) ) ;
#8814 = EDGE_CURVE ( 'NONE', #41178, #13383, #10001, .T. ) ;
#8815 = ADVANCED_FACE ( 'NONE', ( #29723 ), #26467, .F. ) ;
#8816 = EDGE_CURVE ( 'NONE', #49529, #19075, #47020, .T. ) ;
#8817 = ORIENTED_EDGE ( 'NONE', *, *, #2561, .T. ) ;
#8818 = AXIS2_PLACEMENT_3D ( 'NONE', #16839, #43691, #35213 ) ;
#8819 = CARTESIAN_POINT ( 'NONE',  ( -25.85160320928759248, 17.67349956316208193, 4.606045228336897779 ) ) ;
#8820 = CARTESIAN_POINT ( 'NONE',  ( -28.93060053386082231, -0.1191753592594197858, 8.019254159017428663 ) ) ;
#8821 = VECTOR ( 'NONE', #31799, 1000.000000000000000 ) ;
#8822 = ORIENTED_EDGE ( 'NONE', *, *, #2857, .F. ) ;
#8823 = LINE ( 'NONE', #21841, #11331 ) ;
#8824 = FACE_OUTER_BOUND ( 'NONE', #8225, .T. ) ;
#8825 = DIRECTION ( 'NONE',  ( -0.005002170337468016433, -0.7660444431189770143, 0.6427681459581293666 ) ) ;
#8826 = DIRECTION ( 'NONE',  ( 0.5364919789714477361, 0.6444004775717706579, 0.5449076811759711036 ) ) ;
#8827 = ORIENTED_EDGE ( 'NONE', *, *, #1850, .T. ) ;
#8828 = B_SPLINE_CURVE_WITH_KNOTS ( 'NONE', 3,
 ( #45864, #37071, #54372, #34757 ),
 .UNSPECIFIED., .F., .F.,
 ( 4, 4 ),
 ( 0.6233793831165909127, 0.6485820559972910182 ),
 .UNSPECIFIED. ) ;
#8829 = LINE ( 'NONE', #38332, #21026 ) ;
#8830 = FACE_OUTER_BOUND ( 'NONE', #11920, .T. ) ;
#8831 = LINE ( 'NONE', #3429, #33060 ) ;
#8832 = EDGE_CURVE ( 'NONE', #41466, #23008, #52867, .T. ) ;
#8833 = DIRECTION ( 'NONE',  ( -0.9999697198139514409, -0.000000000000000000, -0.007781995580013368816 ) ) ;
#8834 = CARTESIAN_POINT ( 'NONE',  ( -13.63673279712320507, -0.1191753592594197858, 12.22739664767016521 ) ) ;
#8835 = PLANE ( 'NONE',  #20374 ) ;
#8836 = CARTESIAN_POINT ( 'NONE',  ( -8.875996589204540044, 0.000000000000000000, 10.41778544861944233 ) ) ;
#8837 = EDGE_CURVE ( 'NONE', #11293, #51591, #35557, .T. ) ;
#8838 = CARTESIAN_POINT ( 'NONE',  ( -11.27023153255588284, -0.1191753592594177180, 6.679362954920378570 ) ) ;
#8839 = LINE ( 'NONE', #26143, #16817 ) ;
#8840 =( NAMED_UNIT ( * ) PLANE_ANGLE_UNIT ( ) SI_UNIT ( $, .RADIAN. ) );
#8841 = EDGE_CURVE ( 'NONE', #21438, #55768, #9745, .T. ) ;
#8842 = DIRECTION ( 'NONE',  ( 0.5364919789714477361, 0.6444004775717706579, 0.5449076811759711036 ) ) ;
#8843 = ORIENTED_EDGE ( 'NONE', *, *, #27748, .F. ) ;
#8844 = DIRECTION ( 'NONE',  ( -0.8531650599175527594, 0.4028455766673922356, 0.3313982828793700652 ) ) ;
#8845 = DIRECTION ( 'NONE',  ( -0.5364919789714478471, 0.6444004775717705469, -0.5449076811759709926 ) ) ;
#8846 = ADVANCED_FACE ( 'NONE', ( #44360 ), #8125, .F. ) ;
#8847 = CARTESIAN_POINT ( 'NONE',  ( -29.86197018149027116, 0.000000000000000000, 8.281335066757780083 ) ) ;
#8848 = LINE ( 'NONE', #39188, #7888 ) ;
#8849 = CARTESIAN_POINT ( 'NONE',  ( -14.10280672071693431, -0.1191753592594197858, 12.40843558753103792 ) ) ;
#8850 = ORIENTED_EDGE ( 'NONE', *, *, #10807, .T. ) ;
#8851 = VECTOR ( 'NONE', #28230, 1000.000000000000227 ) ;
#8852 = ORIENTED_EDGE ( 'NONE', *, *, #33743, .F. ) ;
#8853 = LINE ( 'NONE', #43463, #24090 ) ;
#8854 = DIRECTION ( 'NONE',  ( 0.8531650599175527594, 0.4028455766673922356, -0.3313982828793700652 ) ) ;
#8855 = ORIENTED_EDGE ( 'NONE', *, *, #37906, .T. ) ;
#8856 = CARTESIAN_POINT ( 'NONE',  ( -14.46888367232926420, 0.000000000000000000, 12.59025272694991315 ) ) ;
#8857 = AXIS2_PLACEMENT_3D ( 'NONE', #46722, #3560, #55506 ) ;
#8858 = ORIENTED_EDGE ( 'NONE', *, *, #52601, .T. ) ;
#8859 = CARTESIAN_POINT ( 'NONE',  ( -19.91360065290022519, -5.375054281893163477, 13.23843028808050981 ) ) ;
#8860 = ORIENTED_EDGE ( 'NONE', *, *, #49996, .T. ) ;
#8861 = FACE_OUTER_BOUND ( 'NONE', #55273, .T. ) ;
#8862 = VERTEX_POINT ( 'NONE', #31600 ) ;
#8863 = ORIENTED_EDGE ( 'NONE', *, *, #16499, .F. ) ;
#8864 = ORIENTED_EDGE ( 'NONE', *, *, #11237, .T. ) ;
#8865 = FACE_OUTER_BOUND ( 'NONE', #3686, .T. ) ;
#8866 = CARTESIAN_POINT ( 'NONE',  ( -12.33850799832341849, 0.000000000000000000, 11.68350162852954632 ) ) ;
#8867 = DIRECTION ( 'NONE',  ( 0.9999697198139515519, 0.000000000000000000, 0.007781995580013368816 ) ) ;
#8868 = FACE_OUTER_BOUND ( 'NONE', #53846, .T. ) ;
#8869 = ORIENTED_EDGE ( 'NONE', *, *, #42354, .F. ) ;
#8871 = ORIENTED_EDGE ( 'NONE', *, *, #28830, .F. ) ;
#8870 = EDGE_CURVE ( 'NONE', #31757, #25455, #5742, .T. ) ;
#8872 = EDGE_LOOP ( 'NONE', ( #26246, #26589, #9553, #44748 ) ) ;
#8873 = EDGE_CURVE ( 'NONE', #14416, #54500, #31856, .T. ) ;
#8874 = CARTESIAN_POINT ( 'NONE',  ( -18.66354898467281132, 0.000000000000000000, 14.21960318569776582 ) ) ;
#8875 = EDGE_LOOP ( 'NONE', ( #9908, #53592, #49225, #388 ) ) ;
#8876 = FACE_OUTER_BOUND ( 'NONE', #32982, .T. ) ;
#8877 = VERTEX_POINT ( 'NONE', #45208 ) ;
#8878 = FACE_OUTER_BOUND ( 'NONE', #29743, .T. ) ;
#8879 = CARTESIAN_POINT ( 'NONE',  ( -11.87243407472968926, 0.000000000000000000, 11.50246268866867361 ) ) ;
#8880 = EDGE_CURVE ( 'NONE', #1004, #40111, #7147, .T. ) ;
#8881 = EDGE_CURVE ( 'NONE', #24619, #50967, #49993, .T. ) ;
#8882 = EDGE_CURVE ( 'NONE', #37125, #23998, #23888, .T. ) ;
#8883 = ORIENTED_EDGE ( 'NONE', *, *, #44777, .F. ) ;
#8884 = DIRECTION ( 'NONE',  ( 0.9999697198139515519, 0.000000000000000000, 0.007781995580013368816 ) ) ;
#8885 = ORIENTED_EDGE ( 'NONE', *, *, #20979, .F. ) ;
#8886 = ADVANCED_FACE ( 'NONE', ( #50287 ), #6575, .F. ) ;
#8887 = VECTOR ( 'NONE', #42559, 1000.000000000000000 ) ;
#8888 = CARTESIAN_POINT ( 'NONE',  ( -21.97156659400807044, 4.819660872929010687, 13.32570833076115946 ) ) ;
#8889 = ORIENTED_EDGE ( 'NONE', *, *, #53359, .T. ) ;
#8890 = CARTESIAN_POINT ( 'NONE',  ( -9.956977639035045513, 0.000000000000000000, 4.204261539843453299 ) ) ;
#8891 = LINE ( 'NONE', #52320, #42014 ) ;
#8892 = LINE ( 'NONE', #48041, #38247 ) ;
#8893 = VERTEX_POINT ( 'NONE', #15635 ) ;
#8894 = LINE ( 'NONE', #8598, #11126 ) ;
#8895 = AXIS2_PLACEMENT_3D ( 'NONE', #44998, #19963, #54586 ) ;
#8896 = DIRECTION ( 'NONE',  ( 0.000000000000000000, -1.000000000000000000, 0.000000000000000000 ) ) ;
#8897 = DIRECTION ( 'NONE',  ( -0.6427681459581293666, -0.7660444431189770143, -0.005002170337467561935 ) ) ;
#8898 = DIRECTION ( 'NONE',  ( 0.5449076811759707706, 0.6444004775717708799, -0.5364919789714476250 ) ) ;
#8899 = DIRECTION ( 'NONE',  ( -0.6246952433987894571, 0.7422098413412802076, 0.2426528472758539834 ) ) ;
#8901 = EDGE_CURVE ( 'NONE', #13096, #21986, #36393, .T. ) ;
#8900 = DIRECTION ( 'NONE',  ( -0.2426528472758542054, 0.7422098413412800966, -0.6246952433987894571 ) ) ;
#8902 = DIRECTION ( 'NONE',  ( 0.9999697198139515519, 0.000000000000000000, 0.007781995580013368816 ) ) ;
#8903 = ORIENTED_EDGE ( 'NONE', *, *, #40879, .T. ) ;
#8904 = DIRECTION ( 'NONE',  ( -0.005961354470445682716, -0.6427876096865404731, 0.7660212471507180654 ) ) ;
#8905 = CARTESIAN_POINT ( 'NONE',  ( -26.21622229497770817, 17.48042152905857449, -4.621141326338904065 ) ) ;
#8906 = EDGE_CURVE ( 'NONE', #14383, #54636, #53444, .T. ) ;
#8907 = DIRECTION ( 'NONE',  ( 0.5364919789714477361, 0.6444004775717706579, 0.5449076811759711036 ) ) ;
#8908 = ORIENTED_EDGE ( 'NONE', *, *, #36382, .T. ) ;
#8909 = LINE ( 'NONE', #21929, #3933 ) ;
#8910 = ORIENTED_EDGE ( 'NONE', *, *, #11620, .F. ) ;
#8911 = PLANE ( 'NONE',  #47949 ) ;
#8912 = ADVANCED_FACE ( 'NONE', ( #45744 ), #2311, .F. ) ;
#8913 = LINE ( 'NONE', #5464, #42060 ) ;
#8914 = CARTESIAN_POINT ( 'NONE',  ( -21.47341775636118655, -0.1191753592594197858, 5.122631121243466090 ) ) ;
#8915 = EDGE_CURVE ( 'NONE', #34779, #35810, #27607, .T. ) ;
#8916 = LINE ( 'NONE', #22523, #4804 ) ;
#8917 = ORIENTED_EDGE ( 'NONE', *, *, #51725, .T. ) ;
#8918 = ORIENTED_EDGE ( 'NONE', *, *, #36572, .T. ) ;
#8919 = DIRECTION ( 'NONE',  ( 0.007781995580012663651, 0.000000000000000000, -0.9999697198139515519 ) ) ;
#8920 = LINE ( 'NONE', #31609, #28633 ) ;
#8921 = DIRECTION ( 'NONE',  ( 0.007781995580012662783, 0.000000000000000000, -0.9999697198139514409 ) ) ;
#8922 = CARTESIAN_POINT ( 'NONE',  ( -26.13493519185646008, 0.000000000000000000, 7.033017491833586377 ) ) ;
#8923 = CARTESIAN_POINT ( 'NONE',  ( -22.40556560354864146, -0.1191753592594197858, 5.484709000965211523 ) ) ;
#8924 = CARTESIAN_POINT ( 'NONE',  ( -15.40600537535590142, -3.917936722690661178, 9.096149048148156169 ) ) ;
#8925 = ORIENTED_EDGE ( 'NONE', *, *, #46253, .T. ) ;
#8926 = CARTESIAN_POINT ( 'NONE',  ( -18.39746900504187010, 0.000000000000000000, 14.03700784672088808 ) ) ;
#8927 = DIRECTION ( 'NONE',  ( 0.8660254037844380415, 0.5000000000000011102, 0.000000000000000000 ) ) ;
#8928 = ORIENTED_EDGE ( 'NONE', *, *, #29439, .T. ) ;
#8929 = CARTESIAN_POINT ( 'NONE',  ( -15.10091574723437802, 0.000000000000000000, 8.396209005525733460 ) ) ;
#8930 = DIRECTION ( 'NONE',  ( 0.5449076811759707706, 0.6444004775717708799, -0.5364919789714476250 ) ) ;
#8931 = CARTESIAN_POINT ( 'NONE',  ( -12.13851405436063047, 0.000000000000000000, 11.68505802764555135 ) ) ;
#8932 = ORIENTED_EDGE ( 'NONE', *, *, #40884, .F. ) ;
#8933 = VECTOR ( 'NONE', #25019, 999.9999999999998863 ) ;
#8934 = CARTESIAN_POINT ( 'NONE',  ( -19.22961988024793101, -0.1191753592594177458, 14.39986392600063603 ) ) ;
#8935 = ORIENTED_EDGE ( 'NONE', *, *, #7006, .F. ) ;
#8936 = ORIENTED_EDGE ( 'NONE', *, *, #44246, .T. ) ;
#8937 = ORIENTED_EDGE ( 'NONE', *, *, #29156, .T. ) ;
#8938 = EDGE_LOOP ( 'NONE', ( #29865, #52081, #53566, #15654 ) ) ;
#8939 = DIRECTION ( 'NONE',  ( 0.000000000000000000, -1.000000000000000000, 0.000000000000000000 ) ) ;
#8940 = ORIENTED_EDGE ( 'NONE', *, *, #18960, .T. ) ;
#8941 = CARTESIAN_POINT ( 'NONE',  ( -12.68893542602017988, 23.60026475436954740, -3.594889907554657427 ) ) ;
#8942 = EDGE_CURVE ( 'NONE', #53450, #21341, #19347, .T. ) ;
#8943 = EDGE_LOOP ( 'NONE', ( #40478, #26337, #29664, #33700 ) ) ;
#8944 = DIRECTION ( 'NONE',  ( -0.6427681459581293666, -0.7660444431189770143, -0.005002170337467561935 ) ) ;
#8945 = VERTEX_POINT ( 'NONE', #44930 ) ;
#8946 = DIRECTION ( 'NONE',  ( 0.007781995580012663651, -3.146120232559066537E-19, -0.9999697198139514409 ) ) ;
#8947 = ORIENTED_EDGE ( 'NONE', *, *, #37432, .T. ) ;
#8948 = EDGE_CURVE ( 'NONE', #2320, #45947, #19647, .T. ) ;
#8949 = EDGE_CURVE ( 'NONE', #49206, #9950, #49168, .T. ) ;
#8950 = PLANE ( 'NONE',  #1184 ) ;
#8951 = CARTESIAN_POINT ( 'NONE',  ( -17.59067451224156642, 1.905425754524006532, 3.453954036298156005 ) ) ;
#8952 = LINE ( 'NONE', #47257, #50326 ) ;
#8953 = DIRECTION ( 'NONE',  ( -0.9999697198139514409, -0.000000000000000000, -0.007781995580013368816 ) ) ;
#8954 = LINE ( 'NONE', #26255, #46441 ) ;
#8955 = ORIENTED_EDGE ( 'NONE', *, *, #28545, .F. ) ;
#8956 = ORIENTED_EDGE ( 'NONE', *, *, #53156, .F. ) ;
#8957 = CARTESIAN_POINT ( 'NONE',  ( -9.771353962598668730, 0.000000000000000000, 6.052366455248280097 ) ) ;
#8958 = CARTESIAN_POINT ( 'NONE',  ( -11.32921355590532109, 0.000000000000000000, 1.408251937772285300 ) ) ;
#8959 = CARTESIAN_POINT ( 'NONE',  ( -15.95701152500570608, -0.03739765774599677212, 3.018190368296854498 ) ) ;
#8960 = DIRECTION ( 'NONE',  ( -0.5364919789714478471, 0.6444004775717705469, -0.5449076811759709926 ) ) ;
#8961 = CARTESIAN_POINT ( 'NONE',  ( 2.072287782118878319, 0.000000000000000000, -2.950529333540147015 ) ) ;
#8962 = LINE ( 'NONE', #52397, #30485 ) ;
#8963 = ORIENTED_EDGE ( 'NONE', *, *, #33272, .T. ) ;
#8964 = DIRECTION ( 'NONE',  ( 0.5364919789714477361, 0.6444004775717706579, 0.5449076811759711036 ) ) ;
#8965 = CARTESIAN_POINT ( 'NONE',  ( -56.20083583094844926, 4.876814673940706335, 2.999999999999993339 ) ) ;
#8966 = VERTEX_POINT ( 'NONE', #28731 ) ;
#8967 = AXIS2_PLACEMENT_3D ( 'NONE', #8059, #3770, #34189 ) ;
#8968 = FACE_OUTER_BOUND ( 'NONE', #12976, .T. ) ;
#8969 = CARTESIAN_POINT ( 'NONE',  ( -64.10539783498545319, 7.375519243179410545, 3.000000000000000000 ) ) ;
#8970 = CARTESIAN_POINT ( 'NONE',  ( -12.09873015469866253, 0.000000000000000000, 6.572912358960970813 ) ) ;
#8971 = EDGE_CURVE ( 'NONE', #35486, #11724, #23613, .T. ) ;
#8972 = DIRECTION ( 'NONE',  ( 0.9999697198139515519, 0.000000000000000000, 0.007781995580013368816 ) ) ;
#8973 = DIRECTION ( 'NONE',  ( 0.5364919789714477361, 0.6444004775717706579, 0.5449076811759711036 ) ) ;
#8974 = EDGE_LOOP ( 'NONE', ( #4960, #8088, #41504 ) ) ;
#8975 = ADVANCED_FACE ( 'NONE', ( #6044 ), #19907, .F. ) ;
#8976 = VERTEX_POINT ( 'NONE', #36143 ) ;
#8977 = CARTESIAN_POINT ( 'NONE',  ( -14.00280974873554030, 0.000000000000000000, 12.40921378708904044 ) ) ;
#8978 = DIRECTION ( 'NONE',  ( 0.5364919789714477361, 0.6444004775717706579, 0.5449076811759711036 ) ) ;
#8979 = DIRECTION ( 'NONE',  ( 0.5364919789714477361, 0.6444004775717706579, 0.5449076811759711036 ) ) ;
#8980 = FACE_OUTER_BOUND ( 'NONE', #25387, .T. ) ;
#8981 = ADVANCED_FACE ( 'NONE', ( #15370 ), #36684, .F. ) ;
#8982 = CARTESIAN_POINT ( 'NONE',  ( -45.77156441860526570, 4.499999999999973355, 5.000000000000000000 ) ) ;
#8983 = CARTESIAN_POINT ( 'NONE',  ( -13.01702680972596227, 25.14289191323709360, -3.508089884283071669 ) ) ;
#8984 = PLANE ( 'NONE',  #28397 ) ;
#8985 = ORIENTED_EDGE ( 'NONE', *, *, #9455, .T. ) ;
#8986 = LINE ( 'NONE', #26287, #30520 ) ;
#8987 = DIRECTION ( 'NONE',  ( 0.007781995580012662783, 0.000000000000000000, -0.9999697198139514409 ) ) ;
#8988 = VERTEX_POINT ( 'NONE', #1748 ) ;
#8989 = DIRECTION ( 'NONE',  ( 0.005961354470445682716, -0.6427876096865404731, -0.7660212471507180654 ) ) ;
#8990 = ORIENTED_EDGE ( 'NONE', *, *, #37009, .T. ) ;
#8991 = CARTESIAN_POINT ( 'NONE',  ( -21.64218843024125860, 20.16315252982854034, -4.391944182239861050 ) ) ;
#8992 = B_SPLINE_CURVE_WITH_KNOTS ( 'NONE', 3,
 ( #20664, #12696, #42239, #37704, #42518, #41655, #16970, #55027, #37391, #11582, #16118, #7586, #29458, #51325, #55561, #24914 ),
 .UNSPECIFIED., .F., .F.,
 ( 4, 2, 2, 2, 2, 2, 2, 4 ),
 ( 3.469446951953618041E-18, 0.001965516910292332883, 0.003931033820584662296, 0.007862067641169319387, 0.009827584551461647500, 0.01179310146175397735, 0.01375861837204630372, 0.01572413528233863184 ),
 .UNSPECIFIED. ) ;
#8993 = CARTESIAN_POINT ( 'NONE',  ( -20.54049170961573267, 0.000000000000000000, 4.660556269540326646 ) ) ;
#8994 = ORIENTED_EDGE ( 'NONE', *, *, #45650, .T. ) ;
#8995 = VERTEX_POINT ( 'NONE', #19070 ) ;
#8996 = EDGE_LOOP ( 'NONE', ( #615, #32549, #31545, #48006 ) ) ;
#8997 = VERTEX_POINT ( 'NONE', #14821 ) ;
#8998 = ORIENTED_EDGE ( 'NONE', *, *, #16462, .F. ) ;
#8999 = ORIENTED_EDGE ( 'NONE', *, *, #26082, .F. ) ;
#9000 = DIRECTION ( 'NONE',  ( -0.5449076811759708816, 0.6444004775717707689, 0.5364919789714475140 ) ) ;
#9001 = DIRECTION ( 'NONE',  ( -0.9999697198139514409, -0.000000000000000000, -0.007781995580013368816 ) ) ;
#9002 = EDGE_CURVE ( 'NONE', #2126, #44201, #32149, .T. ) ;
#9003 = PLANE ( 'NONE',  #26743 ) ;
#9004 = VERTEX_POINT ( 'NONE', #37814 ) ;
#9005 = CARTESIAN_POINT ( 'NONE',  ( -8.063280706518755281, 0.000000000000000000, 6.234985089866581731 ) ) ;
#9006 = VERTEX_POINT ( 'NONE', #3440 ) ;
#9007 = ORIENTED_EDGE ( 'NONE', *, *, #23512, .T. ) ;
#9008 = ADVANCED_FACE ( 'NONE', ( #51125 ), #34384, .F. ) ;
#9009 = CARTESIAN_POINT ( 'NONE',  ( 5.488878160879001378, 0.000000000000000000, 2.420140035803472589 ) ) ;
#9010 = DIRECTION ( 'NONE',  ( -0.7660212471507179544, -0.6427876096865405842, -0.005961354470445141482 ) ) ;
#9011 = DIRECTION ( 'NONE',  ( 0.9999697198139515519, 0.000000000000000000, 0.007781995580013368816 ) ) ;
#9012 = VERTEX_POINT ( 'NONE', #34112 ) ;
#9013 = CARTESIAN_POINT ( 'NONE',  ( -16.95814568020944435, 0.000000000000000000, 8.212429599158721061 ) ) ;
#9014 = ORIENTED_EDGE ( 'NONE', *, *, #2184, .F. ) ;
#9015 = DIRECTION ( 'NONE',  ( 0.005002170337468016433, -0.7660444431189770143, -0.6427681459581293666 ) ) ;
#9016 = CARTESIAN_POINT ( 'NONE',  ( -15.40103151951671734, 0.000000000000000000, 12.95233060667165681 ) ) ;
#9017 = ADVANCED_FACE ( 'NONE', ( #29849 ), #54828, .F. ) ;
#9018 = CARTESIAN_POINT ( 'NONE',  ( -14.46888367232926420, 0.000000000000000000, 12.59025272694991315 ) ) ;
#9019 = CARTESIAN_POINT ( 'NONE',  ( -17.28938333041720554, 2.067327705546507133, 6.989941716411668615 ) ) ;
#9020 = CARTESIAN_POINT ( 'NONE',  ( -13.69838289619527494, 0.000000000000000000, 7.299127631056469667 ) ) ;
#9021 = DIRECTION ( 'NONE',  ( 0.000000000000000000, 0.000000000000000000, 1.000000000000000000 ) ) ;
#9022 = DIRECTION ( 'NONE',  ( 0.6246952433987893460, 0.7422098413412802076, -0.2426528472758539279 ) ) ;
#9023 = CARTESIAN_POINT ( 'NONE',  ( -68.15152480690021264, -11.52292790806604117, 6.355103916287435872 ) ) ;
#9024 = ORIENTED_EDGE ( 'NONE', *, *, #20232, .F. ) ;
#9025 = DIRECTION ( 'NONE',  ( 0.007781995580012663651, 0.000000000000000000, -0.9999697198139515519 ) ) ;
#9026 = DIRECTION ( 'NONE',  ( 0.000000000000000000, -0.000000000000000000, -1.000000000000000000 ) ) ;
#9027 = CARTESIAN_POINT ( 'NONE',  ( -20.06177075545399191, 0.000000000000000000, 14.76272000528038220 ) ) ;
#9028 = CARTESIAN_POINT ( 'NONE',  ( -8.318202594104366909, -8.005327475259342407, 0.01269879923549658424 ) ) ;
#9029 = CARTESIAN_POINT ( 'NONE',  ( 2.072287782118878319, 0.000000000000000000, -2.950529333540147015 ) ) ;
#9030 = DIRECTION ( 'NONE',  ( -0.6427681459581293666, -0.7660444431189770143, -0.005002170337467561935 ) ) ;
#9031 = FACE_OUTER_BOUND ( 'NONE', #2109, .T. ) ;
#9032 = CARTESIAN_POINT ( 'NONE',  ( -27.99923088623136636, 0.000000000000000000, 7.757173251277078130 ) ) ;
#9033 = ORIENTED_EDGE ( 'NONE', *, *, #12521, .F. ) ;
#9034 = DIRECTION ( 'NONE',  ( 0.007781995580012662783, 0.000000000000000000, -0.9999697198139514409 ) ) ;
#9035 = PLANE ( 'NONE',  #3164 ) ;
#9036 = DIRECTION ( 'NONE',  ( 0.005961354470445682716, -0.6427876096865404731, -0.7660212471507180654 ) ) ;
#9037 = AXIS2_PLACEMENT_3D ( 'NONE', #24645, #15855, #33203 ) ;
#9038 = DIRECTION ( 'NONE',  ( -0.9999697198139514409, -0.000000000000000000, -0.007781995580013368816 ) ) ;
#9039 = EDGE_CURVE ( 'NONE', #21762, #23836, #2842, .T. ) ;
#9040 = LINE ( 'NONE', #13317, #33036 ) ;
#9041 = CARTESIAN_POINT ( 'NONE',  ( -4.360905869600901319, 1.733607939028554791E-14, -3.600000000000000089 ) ) ;
#9042 = DIRECTION ( 'NONE',  ( 0.5449076811759707706, 0.6444004775717708799, -0.5364919789714476250 ) ) ;
#9043 = DIRECTION ( 'NONE',  ( -0.2426528472758542054, 0.7422098413412800966, -0.6246952433987894571 ) ) ;
#9044 = EDGE_LOOP ( 'NONE', ( #16926, #18672, #23571, #3270 ) ) ;
#9045 = DIRECTION ( 'NONE',  ( 0.9999697198139515519, 0.000000000000000000, 0.007781995580013368816 ) ) ;
#9046 = EDGE_CURVE ( 'NONE', #56189, #17210, #51687, .T. ) ;
#9047 = EDGE_LOOP ( 'NONE', ( #54406, #54994, #35135, #38059 ) ) ;
#9048 = EDGE_CURVE ( 'NONE', #18658, #11310, #12531, .T. ) ;
#9049 = EDGE_CURVE ( 'NONE', #18417, #12427, #47187, .T. ) ;
#9050 = VERTEX_POINT ( 'NONE', #42885 ) ;
#9051 = ORIENTED_EDGE ( 'NONE', *, *, #19766, .T. ) ;
#9052 = ORIENTED_EDGE ( 'NONE', *, *, #26458, .T. ) ;
#9053 = ORIENTED_EDGE ( 'NONE', *, *, #25183, .T. ) ;
#9054 = LINE ( 'NONE', #51917, #12423 ) ;
#9055 = ADVANCED_FACE ( 'NONE', ( #47429 ), #50584, .T. ) ;
#9056 = FACE_OUTER_BOUND ( 'NONE', #2396, .T. ) ;
#9058 = EDGE_CURVE ( 'NONE', #10554, #3178, #21321, .T. ) ;
#9057 = EDGE_LOOP ( 'NONE', ( #32793, #41873, #28124, #16894 ) ) ;
#9059 = EDGE_LOOP ( 'NONE', ( #51760, #45692, #22280, #48158 ) ) ;
#9060 = EDGE_CURVE ( 'NONE', #54876, #34978, #16778, .T. ) ;
#9061 = FACE_OUTER_BOUND ( 'NONE', #34598, .T. ) ;
#9062 = ORIENTED_EDGE ( 'NONE', *, *, #107, .T. ) ;
#9063 = CARTESIAN_POINT ( 'NONE',  ( -50.27554558092695913, 4.209026340267034705, 5.000000000000000000 ) ) ;
#9064 = CARTESIAN_POINT ( 'NONE',  ( -15.88130887279446490, 0.000000000000000000, 3.050160814894388839 ) ) ;
#9065 = VERTEX_POINT ( 'NONE', #3701 ) ;
#9066 = DIRECTION ( 'NONE',  ( 0.005002170337468016433, -0.7660444431189770143, -0.6427681459581293666 ) ) ;
#9067 = ADVANCED_FACE ( 'NONE', ( #33810 ), #7993, .F. ) ;
#9068 = ORIENTED_EDGE ( 'NONE', *, *, #9896, .T. ) ;
#9069 = LINE ( 'NONE', #42586, #1918 ) ;
#9070 = ADVANCED_FACE ( 'NONE', ( #12792 ), #25303, .F. ) ;
#9071 = DIRECTION ( 'NONE',  ( 0.5449076811759707706, 0.6444004775717708799, -0.5364919789714476250 ) ) ;
#9072 = FACE_OUTER_BOUND ( 'NONE', #12106, .T. ) ;
#9073 = ORIENTED_EDGE ( 'NONE', *, *, #14413, .T. ) ;
#9074 = DIRECTION ( 'NONE',  ( -0.5364919789714478471, 0.6444004775717705469, -0.5449076811759709926 ) ) ;
#9075 = DIRECTION ( 'NONE',  ( -0.7660212471507179544, -0.6427876096865405842, -0.005961354470445141482 ) ) ;
#9076 = CARTESIAN_POINT ( 'NONE',  ( 0.000000000000000000, -1.000000000000000000, 2.125000000000000000 ) ) ;
#9077 = ORIENTED_EDGE ( 'NONE', *, *, #4454, .F. ) ;
#9078 = LINE ( 'NONE', #30679, #47375 ) ;
#9079 = EDGE_LOOP ( 'NONE', ( #41764, #30926, #43119, #51582 ) ) ;
#9080 = CARTESIAN_POINT ( 'NONE',  ( -13.17065887352947762, -0.1191753592594197858, 12.04635770780929427 ) ) ;
#9081 = CARTESIAN_POINT ( 'NONE',  ( -10.40568786923371469, 0.000000000000000000, 2.154103167823834042 ) ) ;
#9082 = CARTESIAN_POINT ( 'NONE',  ( -61.56892328330737030, 6.937430383826147740, 2.999999999999993339 ) ) ;
#9083 = DIRECTION ( 'NONE',  ( 0.007781995580012663651, 0.000000000000000000, -0.9999697198139515519 ) ) ;
#9084 = DIRECTION ( 'NONE',  ( 0.3535533905932738974, -0.6123724356957929160, -0.7071067811865487940 ) ) ;
#9085 = CARTESIAN_POINT ( 'NONE',  ( -16.33317936670417225, 0.000000000000000000, 13.31440848639340224 ) ) ;
#9086 = CARTESIAN_POINT ( 'NONE',  ( -11.70612789434414402, -0.1191753592594183703, 2.982650010574726451 ) ) ;
#9087 = CARTESIAN_POINT ( 'NONE',  ( -13.07066190154808361, 0.000000000000000000, 12.04713590736729678 ) ) ;
#9088 = DIRECTION ( 'NONE',  ( 0.5449076811759707706, 0.6444004775717708799, -0.5364919789714476250 ) ) ;
#9089 = VERTEX_POINT ( 'NONE', #20172 ) ;
#9090 = DIRECTION ( 'NONE',  ( 0.9999697198139515519, 0.000000000000000000, 0.007781995580013368816 ) ) ;
#9091 = FACE_OUTER_BOUND ( 'NONE', #215, .T. ) ;
#9092 = DIRECTION ( 'NONE',  ( 0.000000000000000000, -1.000000000000000000, 0.000000000000000000 ) ) ;
#9093 = CARTESIAN_POINT ( 'NONE',  ( -9.568213099748072992, 0.000000000000000000, 2.360626646347695257 ) ) ;
#9094 = EDGE_CURVE ( 'NONE', #35036, #13331, #20757, .T. ) ;
#9095 = DIRECTION ( 'NONE',  ( -0.005961354470445682716, -0.6427876096865404731, 0.7660212471507180654 ) ) ;
#9096 = CARTESIAN_POINT ( 'NONE',  ( -17.93139508144814442, 0.000000000000000000, 13.85596890686001537 ) ) ;
#9097 = VERTEX_POINT ( 'NONE', #38072 ) ;
#9098 = VECTOR ( 'NONE', #19163, 999.9999999999998863 ) ;
#9099 = ORIENTED_EDGE ( 'NONE', *, *, #55382, .F. ) ;
#9100 = PLANE ( 'NONE',  #45858 ) ;
#9101 = CARTESIAN_POINT ( 'NONE',  ( -13.12303101290966545, -0.1191753592594181482, 5.926279901332813793 ) ) ;
#9102 = EDGE_LOOP ( 'NONE', ( #43894, #7159, #32465, #48009 ) ) ;
#9103 = EDGE_CURVE ( 'NONE', #40648, #14557, #7399, .T. ) ;
#9104 = EDGE_CURVE ( 'NONE', #4182, #29456, #3145, .T. ) ;
#9105 = DIRECTION ( 'NONE',  ( 0.000000000000000000, -0.000000000000000000, -1.000000000000000000 ) ) ;
#9106 = VERTEX_POINT ( 'NONE', #46579 ) ;
#9107 = DIRECTION ( 'NONE',  ( 0.005961354470445682716, -0.6427876096865404731, -0.7660212471507180654 ) ) ;
#9108 = ORIENTED_EDGE ( 'NONE', *, *, #44510, .T. ) ;
#9109 = DIRECTION ( 'NONE',  ( 0.5449076811759707706, 0.6444004775717708799, -0.5364919789714476250 ) ) ;
#9110 = EDGE_CURVE ( 'NONE', #26525, #44524, #7698, .T. ) ;
#9111 = ORIENTED_EDGE ( 'NONE', *, *, #20318, .T. ) ;
#9112 = VERTEX_POINT ( 'NONE', #26992 ) ;
#9113 = ORIENTED_EDGE ( 'NONE', *, *, #54915, .T. ) ;
#9114 = DIRECTION ( 'NONE',  ( 0.005961354470445682716, -0.6427876096865404731, -0.7660212471507180654 ) ) ;
#9115 = CARTESIAN_POINT ( 'NONE',  ( -27.56460882755735398, 16.74384151918395247, 4.673983433494172779 ) ) ;
#9116 = CARTESIAN_POINT ( 'NONE',  ( -10.27421835998572064, 0.000000000000000000, 10.96090226820206048 ) ) ;
#9117 = CARTESIAN_POINT ( 'NONE',  ( -20.84899999561040573, -2.137015261443159009, 4.911598775153488639 ) ) ;
#9118 = ADVANCED_FACE ( 'NONE', ( #5137 ), #39488, .F. ) ;
#9119 = EDGE_LOOP ( 'NONE', ( #24399, #24303, #18799, #44028 ) ) ;
#9120 = ORIENTED_EDGE ( 'NONE', *, *, #28862, .T. ) ;
#9121 = EDGE_CURVE ( 'NONE', #18181, #51395, #43455, .T. ) ;
#9122 = PLANE ( 'NONE',  #15508 ) ;
#9123 = ORIENTED_EDGE ( 'NONE', *, *, #21047, .F. ) ;
#9124 = CARTESIAN_POINT ( 'NONE',  ( -18.23403687816160712, -0.1191753592594172323, 5.886504871884708834 ) ) ;
#9125 = ORIENTED_EDGE ( 'NONE', *, *, #37405, .F. ) ;
#9126 = FACE_OUTER_BOUND ( 'NONE', #20305, .T. ) ;
#9127 = CARTESIAN_POINT ( 'NONE',  ( -30.79567442779373110, 0.000000000000000000, 8.843406890442315316 ) ) ;
#9128 = EDGE_CURVE ( 'NONE', #46056, #44974, #40026, .T. ) ;
#9129 = EDGE_LOOP ( 'NONE', ( #24949, #23083, #19995, #46392 ) ) ;
#9130 = VECTOR ( 'NONE', #10820, 1000.000000000000227 ) ;
#9131 = DIRECTION ( 'NONE',  ( 0.5364919789714477361, 0.6444004775717706579, 0.5449076811759711036 ) ) ;
#9132 = VERTEX_POINT ( 'NONE', #48848 ) ;
#9133 = VECTOR ( 'NONE', #55671, 999.9999999999998863 ) ;
#9134 = CARTESIAN_POINT ( 'NONE',  ( -18.59215049645273510, 0.000000000000000000, 5.045050781177780941 ) ) ;
#9135 = ORIENTED_EDGE ( 'NONE', *, *, #55863, .F. ) ;
#9136 = LINE ( 'NONE', #48613, #33110 ) ;
#9137 = DIRECTION ( 'NONE',  ( 0.9999697198139515519, 0.000000000000000000, 0.007781995580013368816 ) ) ;
#9138 = LINE ( 'NONE', #39811, #21020 ) ;
#9139 = ORIENTED_EDGE ( 'NONE', *, *, #21364, .T. ) ;
#9140 = CARTESIAN_POINT ( 'NONE',  ( -15.88053067323646417, -0.1191753592594197858, 2.950163842912994383 ) ) ;
#9141 = CARTESIAN_POINT ( 'NONE',  ( -13.08486533123210194, 0.000000000000000000, 1.963927175729152541 ) ) ;
#9142 = PLANE ( 'NONE',  #22194 ) ;
#9143 = FACE_OUTER_BOUND ( 'NONE', #13193, .T. ) ;
#9144 = FACE_OUTER_BOUND ( 'NONE', #9059, .T. ) ;
#9145 = DIRECTION ( 'NONE',  ( 0.000000000000000000, 0.000000000000000000, -1.000000000000000000 ) ) ;
#9146 = PRESENTATION_STYLE_ASSIGNMENT (( #26459 ) ) ;
#9147 = ORIENTED_EDGE ( 'NONE', *, *, #30358, .F. ) ;
#9148 = CARTESIAN_POINT ( 'NONE',  ( -26.13493519185646008, 0.000000000000000000, 7.033017491833586377 ) ) ;
#9149 = PLANE ( 'NONE',  #493 ) ;
#9150 = CARTESIAN_POINT ( 'NONE',  ( -17.93139508144814442, 0.000000000000000000, 13.85596890686001537 ) ) ;
#9151 = ORIENTED_EDGE ( 'NONE', *, *, #22186, .F. ) ;
#9152 = DIRECTION ( 'NONE',  ( -0.6427681459581293666, -0.7660444431189770143, -0.005002170337467561935 ) ) ;
#9153 = CARTESIAN_POINT ( 'NONE',  ( -19.59569683186026268, 0.000000000000000000, 14.58168106541950948 ) ) ;
#9154 = ORIENTED_EDGE ( 'NONE', *, *, #4706, .T. ) ;
#9155 = ADVANCED_FACE ( 'NONE', ( #26691 ), #5403, .F. ) ;
#9156 = DIRECTION ( 'NONE',  ( 0.6427681459581294776, -0.7660444431189769032, 0.005002170337467562802 ) ) ;
#9157 = VECTOR ( 'NONE', #40642, 1000.000000000000114 ) ;
#9158 = DIRECTION ( 'NONE',  ( 0.000000000000000000, -1.000000000000000000, 0.000000000000000000 ) ) ;
#9159 = EDGE_CURVE ( 'NONE', #23847, #3660, #271, .T. ) ;
#9160 = PLANE ( 'NONE',  #4244 ) ;
#9161 = CARTESIAN_POINT ( 'NONE',  ( -70.06679111606356969, 0.1333700068432634167, -7.579899494734611665 ) ) ;
#9162 = VERTEX_POINT ( 'NONE', #26147 ) ;
#9163 = VERTEX_POINT ( 'NONE', #35237 ) ;
#9164 = ADVANCED_FACE ( 'NONE', ( #9091 ), #22459, .F. ) ;
#9165 = LINE ( 'NONE', #9451, #11303 ) ;
#9166 = CARTESIAN_POINT ( 'NONE',  ( -22.40634380310664397, 0.000000000000000000, 5.584705972946605534 ) ) ;
#9167 = LINE ( 'NONE', #12330, #52285 ) ;
#9168 = EDGE_CURVE ( 'NONE', #36770, #24378, #44013, .T. ) ;
#9169 = ADVANCED_FACE ( 'NONE', ( #4552 ), #9677, .F. ) ;
#9170 = EDGE_CURVE ( 'NONE', #5706, #6357, #35489, .T. ) ;
#9171 = CARTESIAN_POINT ( 'NONE',  ( -11.63054826722768453, 25.36602540378449788, -3.000000000000000000 ) ) ;
#9172 = DIRECTION ( 'NONE',  ( 0.000000000000000000, -1.000000000000000000, 0.000000000000000000 ) ) ;
#9173 = VECTOR ( 'NONE', #43690, 1000.000000000000227 ) ;
#9174 = DIRECTION ( 'NONE',  ( -0.005002170337468016433, -0.7660444431189770143, 0.6427681459581293666 ) ) ;
#9176 = EDGE_CURVE ( 'NONE', #37711, #42922, #30409, .T. ) ;
#9175 = ORIENTED_EDGE ( 'NONE', *, *, #53550, .T. ) ;
#9177 = CARTESIAN_POINT ( 'NONE',  ( -19.32961685222932147, 0.000000000000000000, 14.39908572644263351 ) ) ;
#9178 = AXIS2_PLACEMENT_3D ( 'NONE', #8468, #4768, #25797 ) ;
#9179 = FACE_OUTER_BOUND ( 'NONE', #24666, .T. ) ;
#9180 = VERTEX_POINT ( 'NONE', #21865 ) ;
#9181 = CARTESIAN_POINT ( 'NONE',  ( -69.29909153375579933, -8.902711886016962950, -7.496705766434924811 ) ) ;
#9182 = DIRECTION ( 'NONE',  ( 0.7660212471507180654, -0.6427876096865404731, 0.005961354470445141482 ) ) ;
#9183 = CARTESIAN_POINT ( 'NONE',  ( -17.18829999102435124, 0.000000000000000000, 3.778653647413541261 ) ) ;
#9184 = ORIENTED_EDGE ( 'NONE', *, *, #5299, .T. ) ;
#9185 = LINE ( 'NONE', #18254, #13074 ) ;
#9186 = ADVANCED_FACE ( 'NONE', ( #39767 ), #17614, .F. ) ;
#9187 = ORIENTED_EDGE ( 'NONE', *, *, #11569, .T. ) ;
#9189 = VERTEX_POINT ( 'NONE', #21612 ) ;
#9188 = EDGE_CURVE ( 'NONE', #50536, #14368, #34954, .T. ) ;
#9190 = ORIENTED_EDGE ( 'NONE', *, *, #12247, .T. ) ;
#9191 = EDGE_CURVE ( 'NONE', #55170, #547, #4299, .T. ) ;
#9192 = ORIENTED_EDGE ( 'NONE', *, *, #20954, .F. ) ;
#9193 = CARTESIAN_POINT ( 'NONE',  ( -15.68624088420942542, -3.756034771668162797, 2.854552609374020999 ) ) ;
#9194 = EDGE_LOOP ( 'NONE', ( #31975, #8812, #51814, #6619 ) ) ;
#9195 = CARTESIAN_POINT ( 'NONE',  ( 0.3726814890124213187, -6.521129970779321994, -1.535787955176781389E-15 ) ) ;
#9196 = VECTOR ( 'NONE', #3075, 1000.000000000000227 ) ;
#9197 = EDGE_CURVE ( 'NONE', #34282, #49846, #25870, .T. ) ;
#9198 = VECTOR ( 'NONE', #39997, 1000.000000000000227 ) ;
#9199 = ORIENTED_EDGE ( 'NONE', *, *, #9176, .F. ) ;
#9200 = PLANE ( 'NONE',  #51300 ) ;
#9201 = VERTEX_POINT ( 'NONE', #48561 ) ;
#9202 = FACE_OUTER_BOUND ( 'NONE', #52144, .T. ) ;
#9203 = VERTEX_POINT ( 'NONE', #26400 ) ;
#9204 = EDGE_CURVE ( 'NONE', #4025, #6097, #43716, .T. ) ;
#9205 = DIRECTION ( 'NONE',  ( 0.007781995580012662783, 0.000000000000000000, -0.9999697198139514409 ) ) ;
#9206 = PLANE ( 'NONE',  #7831 ) ;
#9207 = CARTESIAN_POINT ( 'NONE',  ( 1.086233639165236964, 0.000000000000000000, 2.796443541562362078 ) ) ;
#9208 = FACE_OUTER_BOUND ( 'NONE', #9391, .T. ) ;
#9209 = DIRECTION ( 'NONE',  ( 0.9999697198139515519, 0.000000000000000000, 0.007781995580013368816 ) ) ;
#9210 = VERTEX_POINT ( 'NONE', #4832 ) ;
#9211 = ORIENTED_EDGE ( 'NONE', *, *, #1371, .F. ) ;
#9212 = LINE ( 'NONE', #8676, #444 ) ;
#9213 = CARTESIAN_POINT ( 'NONE',  ( -12.80458192191714595, 0.000000000000000000, 11.86454056839041726 ) ) ;
#9214 = AXIS2_PLACEMENT_3D ( 'NONE', #39988, #5099, #23258 ) ;
#9215 = DIRECTION ( 'NONE',  ( -0.9999697198139514409, -0.000000000000000000, -0.007781995580013368816 ) ) ;
#9216 = CARTESIAN_POINT ( 'NONE',  ( -18.86354292863559579, 0.000000000000000000, 14.21804678658176080 ) ) ;
#9217 = CARTESIAN_POINT ( 'NONE',  ( 2.072287782118878319, 0.000000000000000000, -2.950529333540147015 ) ) ;
#9218 = LINE ( 'NONE', #26533, #42261 ) ;
#9219 = VERTEX_POINT ( 'NONE', #45396 ) ;
#9220 = DIRECTION ( 'NONE',  ( -0.6427681459581293666, -0.7660444431189770143, -0.005002170337467561935 ) ) ;
#9221 = DIRECTION ( 'NONE',  ( 0.007781995580012663651, -3.146120232559066537E-19, -0.9999697198139514409 ) ) ;
#9222 = ORIENTED_EDGE ( 'NONE', *, *, #20271, .T. ) ;
#9223 = LINE ( 'NONE', #48406, #44265 ) ;
#9224 = CARTESIAN_POINT ( 'NONE',  ( -56.38001980572109062, 4.410024460692103077, 2.999999999999993339 ) ) ;
#9225 = CARTESIAN_POINT ( 'NONE',  ( -10.87319881958008772, 0.000000000000000000, 2.519796959313588491 ) ) ;
#9226 = CARTESIAN_POINT ( 'NONE',  ( -20.06177075545399191, 0.000000000000000000, 14.76272000528038220 ) ) ;
#9227 = DIRECTION ( 'NONE',  ( 0.6427681459581294776, -0.7660444431189769032, 0.005002170337467562802 ) ) ;
#9228 = EDGE_LOOP ( 'NONE', ( #45859, #4232, #21048, #35363 ) ) ;
#9229 = ORIENTED_EDGE ( 'NONE', *, *, #7382, .F. ) ;
#9230 = LINE ( 'NONE', #48719, #17591 ) ;
#9231 = PLANE ( 'NONE',  #11360 ) ;
#9232 = PLANE ( 'NONE',  #30617 ) ;
#9233 = ADVANCED_FACE ( 'NONE', ( #44854 ), #6508, .F. ) ;
#9234 = ADVANCED_FACE ( 'NONE', ( #32624 ), #41149, .F. ) ;
#9235 = AXIS2_PLACEMENT_3D ( 'NONE', #50721, #3315, #28297 ) ;
#9236 = VECTOR ( 'NONE', #52017, 999.9999999999998863 ) ;
#9237 = DIRECTION ( 'NONE',  ( -0.05705673239519651330, 0.9983709377222391712, 2.351258244848514932E-16 ) ) ;
#9238 = CARTESIAN_POINT ( 'NONE',  ( 5.585384064119276459, -1.054099363964956737, -2.341019274736492850 ) ) ;
#9239 = EDGE_CURVE ( 'NONE', #17419, #22456, #13957, .T. ) ;
#9240 = DIRECTION ( 'NONE',  ( 0.007781995580012663651, -3.146120232559066537E-19, -0.9999697198139514409 ) ) ;
#9241 = LINE ( 'NONE', #43597, #5712 ) ;
#9242 = PLANE ( 'NONE',  #25036 ) ;
#9243 = PLANE ( 'NONE',  #7908 ) ;
#9244 = VECTOR ( 'NONE', #9240, 1000.000000000000227 ) ;
#9245 = ORIENTED_EDGE ( 'NONE', *, *, #7453, .T. ) ;
#9246 = DIRECTION ( 'NONE',  ( -0.5364919789714478471, 0.6444004775717705469, -0.5449076811759709926 ) ) ;
#9247 = VERTEX_POINT ( 'NONE', #23818 ) ;
#9248 = LINE ( 'NONE', #34821, #15056 ) ;
#9249 = PLANE ( 'NONE',  #24793 ) ;
#9250 = ORIENTED_EDGE ( 'NONE', *, *, #204, .T. ) ;
#9251 = VECTOR ( 'NONE', #28268, 999.9999999999998863 ) ;
#9252 = ORIENTED_EDGE ( 'NONE', *, *, #13380, .T. ) ;
#9253 = VECTOR ( 'NONE', #32039, 1000.000000000000227 ) ;
#9254 = ORIENTED_EDGE ( 'NONE', *, *, #3282, .F. ) ;
#9255 = ORIENTED_EDGE ( 'NONE', *, *, #11419, .T. ) ;
#9256 = EDGE_LOOP ( 'NONE', ( #27414, #43559, #33986, #38953 ) ) ;
#9257 = ORIENTED_EDGE ( 'NONE', *, *, #53010, .F. ) ;
#9258 = LINE ( 'NONE', #30296, #28613 ) ;
#9259 = DIRECTION ( 'NONE',  ( 0.005961354470445682716, -0.6427876096865404731, -0.7660212471507180654 ) ) ;
#9260 = CARTESIAN_POINT ( 'NONE',  ( -9.984210658517920223, 9.723509473712979911, 7.096580060653336020 ) ) ;
#9261 = EDGE_LOOP ( 'NONE', ( #17584, #13863, #22718 ) ) ;
#9262 = CARTESIAN_POINT ( 'NONE',  ( -14.41041842488296076, 0.000000000000000000, 5.077593987089866090 ) ) ;
#9263 = EDGE_LOOP ( 'NONE', ( #39020, #43140, #8483, #23922 ) ) ;
#9264 = ORIENTED_EDGE ( 'NONE', *, *, #31546, .F. ) ;
#9265 = ADVANCED_FACE ( 'NONE', ( #49686 ), #32081, .F. ) ;
#9266 = CARTESIAN_POINT ( 'NONE',  ( 2.072287782118878319, 0.000000000000000000, -2.950529333540147015 ) ) ;
#9267 = EDGE_CURVE ( 'NONE', #33602, #43397, #18758, .T. ) ;
#9268 = DIRECTION ( 'NONE',  ( -0.9999697198139514409, -0.000000000000000000, -0.007781995580013368816 ) ) ;
#9269 = LINE ( 'NONE', #9861, #50427 ) ;
#9270 = VECTOR ( 'NONE', #20397, 1000.000000000000227 ) ;
#9271 = ADVANCED_FACE ( 'NONE', ( #36915 ), #53925, .F. ) ;
#9272 = ORIENTED_EDGE ( 'NONE', *, *, #39715, .F. ) ;
#9273 = FACE_OUTER_BOUND ( 'NONE', #53647, .T. ) ;
#9274 = ORIENTED_EDGE ( 'NONE', *, *, #28972, .F. ) ;
#9275 = VECTOR ( 'NONE', #24522, 1000.000000000000227 ) ;
#9276 = AXIS2_PLACEMENT_3D ( 'NONE', #9931, #40597, #10766 ) ;
#9277 = EDGE_CURVE ( 'NONE', #9097, #42364, #54215, .T. ) ;
#9278 = DIRECTION ( 'NONE',  ( 0.9999697198139515519, 0.000000000000000000, 0.007781995580013368816 ) ) ;
#9279 = DIRECTION ( 'NONE',  ( 0.000000000000000000, -0.000000000000000000, -1.000000000000000000 ) ) ;
#9280 = VECTOR ( 'NONE', #34819, 1000.000000000000227 ) ;
#9281 = VECTOR ( 'NONE', #7682, 999.9999999999998863 ) ;
#9282 = CARTESIAN_POINT ( 'NONE',  ( -28.92982233430281980, 0.000000000000000000, 7.919257187036034651 ) ) ;
#9283 = LINE ( 'NONE', #26604, #33960 ) ;
#9284 = CARTESIAN_POINT ( 'NONE',  ( 5.618587682346595003, -1.056427131421802557, -2.260561881690064556 ) ) ;
#9285 = CARTESIAN_POINT ( 'NONE',  ( -7.930221204654489320, 7.733889655832618892, 6.298740802997315313 ) ) ;
#9286 = LINE ( 'NONE', #1323, #39516 ) ;
#9287 = EDGE_LOOP ( 'NONE', ( #17646, #38656, #21828, #30524 ) ) ;
#9288 = LINE ( 'NONE', #43929, #30200 ) ;
#9289 = DIRECTION ( 'NONE',  ( -0.000000000000000000, -1.000000000000000000, -0.000000000000000000 ) ) ;
#9290 = DIRECTION ( 'NONE',  ( -0.9999697198139514409, -0.000000000000000000, -0.007781995580013368816 ) ) ;
#9291 = FACE_OUTER_BOUND ( 'NONE', #22558, .T. ) ;
#9292 = COLOUR_RGB ( '', 0.66274510, 0.83137255, 0.94901961) ;
#9293 = CARTESIAN_POINT ( 'NONE',  ( -37.09365488523594223, 9.510193405093987806, -4.936228699513737439 ) ) ;
#9294 = DIRECTION ( 'NONE',  ( -0.7660212471507179544, -0.6427876096865405842, -0.005961354470445141482 ) ) ;
#9295 = CARTESIAN_POINT ( 'NONE',  ( -12.07286367315112052, 0.000000000000000000, 3.249125029641091178 ) ) ;
#9296 = CARTESIAN_POINT ( 'NONE',  ( -11.05155405620451958, -1.003701604285656579, 2.621975966892176046 ) ) ;
#9297 = ORIENTED_EDGE ( 'NONE', *, *, #51275, .T. ) ;
#9298 = CARTESIAN_POINT ( 'NONE',  ( 1.086233639165236964, 0.000000000000000000, 2.796443541562362078 ) ) ;
#9299 = CARTESIAN_POINT ( 'NONE',  ( -22.15441416008502529, 19.68629195356385964, 4.426028523006688253 ) ) ;
#9300 = DIRECTION ( 'NONE',  ( 0.007781995580012662783, 0.000000000000000000, -0.9999697198139514409 ) ) ;
#9301 = ADVANCED_FACE ( 'NONE', ( #10780 ), #10515, .F. ) ;
#9302 = CARTESIAN_POINT ( 'NONE',  ( -13.43195515176800292, 0.2864062442990031321, 1.890221404860171539 ) ) ;
#9303 = DIRECTION ( 'NONE',  ( 0.7660212471507180654, -0.6427876096865404731, 0.005961354470445141482 ) ) ;
#9304 = VECTOR ( 'NONE', #18599, 999.9999999999998863 ) ;
#9305 = DIRECTION ( 'NONE',  ( 0.9999697198139515519, 0.000000000000000000, 0.007781995580013368816 ) ) ;
#9306 = EDGE_CURVE ( 'NONE', #45407, #994, #51771, .T. ) ;
#9307 = EDGE_CURVE ( 'NONE', #42767, #49508, #28091, .T. ) ;
#9308 = LINE ( 'NONE', #26632, #51908 ) ;
#9309 = DIRECTION ( 'NONE',  ( 0.000000000000000000, 0.000000000000000000, 1.000000000000000000 ) ) ;
#9310 = AXIS2_PLACEMENT_3D ( 'NONE', #6069, #37242, #32700 ) ;
#9311 = CARTESIAN_POINT ( 'NONE',  ( -17.74482636761137044, -0.1191753592594197858, 3.674319602356483916 ) ) ;
#9312 = VECTOR ( 'NONE', #38018, 1000.000000000000000 ) ;
#9313 = VECTOR ( 'NONE', #47075, 1000.000000000000227 ) ;
#9314 = ORIENTED_EDGE ( 'NONE', *, *, #55186, .F. ) ;
#9315 = EDGE_CURVE ( 'NONE', #36994, #28691, #49929, .T. ) ;
#9316 = AXIS2_PLACEMENT_3D ( 'NONE', #45032, #5844, #28240 ) ;
#9317 = ORIENTED_EDGE ( 'NONE', *, *, #21870, .F. ) ;
#9318 = EDGE_LOOP ( 'NONE', ( #8645, #18320, #8042, #5236 ) ) ;
#9319 = VECTOR ( 'NONE', #34027, 999.9999999999998863 ) ;
#9320 = EDGE_LOOP ( 'NONE', ( #23931, #34160, #26154, #53874 ) ) ;
#9321 = ORIENTED_EDGE ( 'NONE', *, *, #19660, .F. ) ;
#9322 = DIRECTION ( 'NONE',  ( 0.007781995580012662783, 0.000000000000000000, -0.9999697198139514409 ) ) ;
#9323 = PLANE ( 'NONE',  #53018 ) ;
#9324 = VERTEX_POINT ( 'NONE', #11035 ) ;
#9325 = ORIENTED_EDGE ( 'NONE', *, *, #53860, .F. ) ;
#9326 = AXIS2_PLACEMENT_3D ( 'NONE', #18995, #6230, #27818 ) ;
#9327 = VECTOR ( 'NONE', #9704, 999.9999999999998863 ) ;
#9328 = FACE_OUTER_BOUND ( 'NONE', #8719, .T. ) ;
#9329 = ORIENTED_EDGE ( 'NONE', *, *, #24412, .T. ) ;
#9330 = DIRECTION ( 'NONE',  ( 0.005002170337468016433, -0.7660444431189770143, -0.6427681459581293666 ) ) ;
#9331 = DIRECTION ( 'NONE',  ( -0.5364919789714478471, 0.6444004775717705469, -0.5449076811759709926 ) ) ;
#9332 = ORIENTED_EDGE ( 'NONE', *, *, #40781, .T. ) ;
#9333 = PLANE ( 'NONE',  #274 ) ;
#9334 = AXIS2_PLACEMENT_3D ( 'NONE', #44280, #39744, #16526 ) ;
#9335 = ORIENTED_EDGE ( 'NONE', *, *, #41113, .T. ) ;
#9336 = CARTESIAN_POINT ( 'NONE',  ( -15.88053067323646417, -0.1191753592594197858, 2.950163842912994383 ) ) ;
#9337 = EDGE_CURVE ( 'NONE', #30427, #24462, #28354, .T. ) ;
#9339 = PLANE ( 'NONE',  #33822 ) ;
#9338 = VECTOR ( 'NONE', #1189, 999.9999999999998863 ) ;
#9340 = DIRECTION ( 'NONE',  ( -0.5364919789714478471, 0.6444004775717705469, -0.5449076811759709926 ) ) ;
#9341 = CARTESIAN_POINT ( 'NONE',  ( -22.40478740399063895, 0.000000000000000000, 5.384712028983816623 ) ) ;
#9342 = ORIENTED_EDGE ( 'NONE', *, *, #43484, .T. ) ;
#9343 = LINE ( 'NONE', #5383, #43079 ) ;
#9344 = CARTESIAN_POINT ( 'NONE',  ( -11.40636015113596180, 0.000000000000000000, 11.32142374880780089 ) ) ;
#9345 = DIRECTION ( 'NONE',  ( -0.3620778797217455991, 0.000000000000000000, -0.9321478471874540261 ) ) ;
#9346 = VECTOR ( 'NONE', #25048, 1000.000000000000227 ) ;
#9347 = ORIENTED_EDGE ( 'NONE', *, *, #36689, .T. ) ;
#9348 = LINE ( 'NONE', #29831, #11975 ) ;
#9349 = ORIENTED_EDGE ( 'NONE', *, *, #40428, .F. ) ;
#9350 = ADVANCED_FACE ( 'NONE', ( #24117 ), #49104, .F. ) ;
#9351 = AXIS2_PLACEMENT_3D ( 'NONE', #6492, #23799, #54736 ) ;
#9352 = VECTOR ( 'NONE', #27964, 1000.000000000000227 ) ;
#9353 = FACE_OUTER_BOUND ( 'NONE', #45790, .T. ) ;
#9354 = CARTESIAN_POINT ( 'NONE',  ( -11.21901323774118708, 0.000000000000000000, 1.039777472322872098 ) ) ;
#9355 = DIRECTION ( 'NONE',  ( 0.000000000000000000, 0.000000000000000000, 1.000000000000000000 ) ) ;
#9356 = DIRECTION ( 'NONE',  ( 0.9999697198139515519, 0.000000000000000000, 0.007781995580013368816 ) ) ;
#9357 = CARTESIAN_POINT ( 'NONE',  ( -13.55892737469792309, -0.1191753592594191197, 2.229566956987161230 ) ) ;
#9358 = EDGE_CURVE ( 'NONE', #2279, #47606, #40615, .T. ) ;
#9359 = CARTESIAN_POINT ( 'NONE',  ( -4.802685646341279480, -6.704367417419401676, 5.083899780593831963 ) ) ;
#9361 = EDGE_CURVE ( 'NONE', #36569, #5010, #42813, .T. ) ;
#9360 = DIRECTION ( 'NONE',  ( -0.005002170337468016433, -0.7660444431189770143, 0.6427681459581293666 ) ) ;
#9362 = VECTOR ( 'NONE', #54549, 999.9999999999998863 ) ;
#9363 = CARTESIAN_POINT ( 'NONE',  ( -12.40300812230242045, 1.257817950434005461, 3.763364223827011745 ) ) ;
#9364 = AXIS2_PLACEMENT_3D ( 'NONE', #36392, #14820, #10588 ) ;
#9365 = CARTESIAN_POINT ( 'NONE',  ( -12.29585004515617186, 0.000000000000000000, 6.202046256587205875 ) ) ;
#9366 = EDGE_LOOP ( 'NONE', ( #32895, #36444, #51302, #38631 ) ) ;
#9367 = CARTESIAN_POINT ( 'NONE',  ( -17.93139508144814442, 0.000000000000000000, 13.85596890686001537 ) ) ;
#9368 = LINE ( 'NONE', #1409, #1533 ) ;
#9369 = EDGE_CURVE ( 'NONE', #50871, #394, #3073, .T. ) ;
#9370 = CARTESIAN_POINT ( 'NONE',  ( -22.07924021441773377, 3.362543313726510164, 5.150975708369738726 ) ) ;
#9371 = CARTESIAN_POINT ( 'NONE',  ( -14.56888064431065821, -0.1191753592594197858, 12.58947452739191064 ) ) ;
#9372 = EDGE_CURVE ( 'NONE', #13435, #48572, #16709, .T. ) ;
#9373 = PLANE ( 'NONE',  #8260 ) ;
#9374 = VECTOR ( 'NONE', #3261, 1000.000000000000114 ) ;
#9375 = DIRECTION ( 'NONE',  ( 0.5364919789714477361, 0.6444004775717706579, 0.5449076811759711036 ) ) ;
#9376 = EDGE_CURVE ( 'NONE', #48014, #32968, #34039, .T. ) ;
#9377 = LINE ( 'NONE', #22717, #11116 ) ;
#9378 = ORIENTED_EDGE ( 'NONE', *, *, #19048, .T. ) ;
#9379 = EDGE_LOOP ( 'NONE', ( #5876, #8031, #4897, #20875 ) ) ;
#9380 = DIRECTION ( 'NONE',  ( 0.007781995580012663651, 0.000000000000000000, -0.9999697198139515519 ) ) ;
#9381 = LINE ( 'NONE', #36344, #42214 ) ;
#9382 = VECTOR ( 'NONE', #15167, 999.9999999999998863 ) ;
#9383 = EDGE_CURVE ( 'NONE', #20306, #21351, #55317, .T. ) ;
#9384 = ORIENTED_EDGE ( 'NONE', *, *, #12093, .T. ) ;
#9385 = CARTESIAN_POINT ( 'NONE',  ( -14.94838282604900748, -0.1191753592594197858, 2.588085963191248506 ) ) ;
#9386 = VECTOR ( 'NONE', #19358, 999.9999999999998863 ) ;
#9387 = EDGE_LOOP ( 'NONE', ( #5558, #42314, #48215, #29695 ) ) ;
#9388 = CARTESIAN_POINT ( 'NONE',  ( -19.47222345087960704, -3.270328918600661439, 4.340653370440049841 ) ) ;
#9389 = ADVANCED_FACE ( 'NONE', ( #46819 ), #24650, .F. ) ;
#9390 = EDGE_LOOP ( 'NONE', ( #55400, #29866, #42316, #11635 ) ) ;
#9391 = EDGE_LOOP ( 'NONE', ( #18919, #24214, #34637, #31822 ) ) ;
#9392 = ORIENTED_EDGE ( 'NONE', *, *, #849, .T. ) ;
#9393 = FACE_OUTER_BOUND ( 'NONE', #3218, .T. ) ;
#9394 = AXIS2_PLACEMENT_3D ( 'NONE', #22871, #40194, #30839 ) ;
#9395 = LINE ( 'NONE', #15, #18703 ) ;
#9396 = CARTESIAN_POINT ( 'NONE',  ( -19.77031582249948016, 4.495856970884011261, 4.217952423934554496 ) ) ;
#9397 = VECTOR ( 'NONE', #40720, 999.9999999999998863 ) ;
#9398 = VECTOR ( 'NONE', #21717, 999.9999999999998863 ) ;
#9399 = FACE_OUTER_BOUND ( 'NONE', #15601, .T. ) ;
#9400 = ORIENTED_EDGE ( 'NONE', *, *, #16222, .T. ) ;
#9401 = ORIENTED_EDGE ( 'NONE', *, *, #9267, .F. ) ;
#9402 = VECTOR ( 'NONE', #39921, 1000.000000000000227 ) ;
#9403 = AXIS2_PLACEMENT_3D ( 'NONE', #24114, #37164, #54213 ) ;
#9404 = CARTESIAN_POINT ( 'NONE',  ( -13.19793970290151641, 0.000000000000000000, 2.701711344436330098 ) ) ;
#9405 = ORIENTED_EDGE ( 'NONE', *, *, #23320, .T. ) ;
#9406 = CARTESIAN_POINT ( 'NONE',  ( -17.68960728864125898, 4.172053068839008283, 10.59961518480473508 ) ) ;
#9407 = EDGE_LOOP ( 'NONE', ( #34536, #30595, #8310, #51335 ) ) ;
#9408 = CARTESIAN_POINT ( 'NONE',  ( -16.06709938707323460, 0.000000000000000000, 13.13181314741652628 ) ) ;
#9409 = LINE ( 'NONE', #27026, #44849 ) ;
#9410 = EDGE_LOOP ( 'NONE', ( #1133, #26358, #28326, #11702 ) ) ;
#9411 = CARTESIAN_POINT ( 'NONE',  ( -16.06709938707323460, 0.000000000000000000, 13.13181314741652628 ) ) ;
#9412 = EDGE_CURVE ( 'NONE', #44511, #18621, #38276, .T. ) ;
#9413 = EDGE_LOOP ( 'NONE', ( #26384, #9392, #12048, #21940 ) ) ;
#9414 = LINE ( 'NONE', #5441, #41780 ) ;
#9415 = VECTOR ( 'NONE', #687, 999.9999999999998863 ) ;
#9416 = ORIENTED_EDGE ( 'NONE', *, *, #34002, .T. ) ;
#9417 = DIRECTION ( 'NONE',  ( -0.2426528472758542054, 0.7422098413412800966, -0.6246952433987894571 ) ) ;
#9418 = LINE ( 'NONE', #19627, #51138 ) ;
#9419 = CARTESIAN_POINT ( 'NONE',  ( -18.67775241435682432, 0.000000000000000000, 4.136394454059623804 ) ) ;
#9420 = ORIENTED_EDGE ( 'NONE', *, *, #21144, .F. ) ;
#9421 = AXIS2_PLACEMENT_3D ( 'NONE', #23266, #27812, #32602 ) ;
#9422 = LINE ( 'NONE', #5189, #17505 ) ;
#9423 = DIRECTION ( 'NONE',  ( 0.6427681459581294776, -0.7660444431189769032, 0.005002170337467562802 ) ) ;
#9424 = CARTESIAN_POINT ( 'NONE',  ( -31.72704407542318350, -0.1191753592594197858, 9.105487798182664960 ) ) ;
#9425 = AXIS2_PLACEMENT_3D ( 'NONE', #17242, #22638, #30869 ) ;
#9426 = DIRECTION ( 'NONE',  ( -0.7886751345948130876, 0.2113248654051844977, 0.5773502691896263972 ) ) ;
#9427 = CARTESIAN_POINT ( 'NONE',  ( -12.62536516875885795, -0.1191753592594181482, 1.685747015088036482 ) ) ;
#9429 = EDGE_CURVE ( 'NONE', #6987, #33042, #15488, .T. ) ;
#9428 = LINE ( 'NONE', #5195, #3441 ) ;
#9430 = CARTESIAN_POINT ( 'NONE',  ( -17.37836304482322802, -5.213152330870664208, 3.465340642280367867 ) ) ;
#9431 = ORIENTED_EDGE ( 'NONE', *, *, #11087, .T. ) ;
#9432 = LINE ( 'NONE', #2006, #48851 ) ;
#9433 = CARTESIAN_POINT ( 'NONE',  ( -22.40634380310664397, 0.000000000000000000, 5.584705972946605534 ) ) ;
#9434 = DIRECTION ( 'NONE',  ( -0.9999697198139514409, -0.000000000000000000, -0.007781995580013368816 ) ) ;
#9435 = ORIENTED_EDGE ( 'NONE', *, *, #21238, .F. ) ;
#9436 = VECTOR ( 'NONE', #2608, 999.9999999999998863 ) ;
#9437 = CARTESIAN_POINT ( 'NONE',  ( -10.74029228357944987, 0.000000000000000000, 11.14194120806293320 ) ) ;
#9438 = CARTESIAN_POINT ( 'NONE',  ( -13.21964368434966630, -3.594132820645663084, 1.901608010842381624 ) ) ;
#9439 = ORIENTED_EDGE ( 'NONE', *, *, #24307, .F. ) ;
#9440 = AXIS2_PLACEMENT_3D ( 'NONE', #51668, #7677, #38323 ) ;
#9441 = CARTESIAN_POINT ( 'NONE',  ( -16.74665552222552733, 0.000000000000000000, 6.736747185243664227 ) ) ;
#9442 = EDGE_CURVE ( 'NONE', #7497, #34473, #20402, .T. ) ;
#9443 = FACE_OUTER_BOUND ( 'NONE', #15976, .T. ) ;
#9444 = CARTESIAN_POINT ( 'NONE',  ( -12.13851405436063047, 0.000000000000000000, 11.68505802764555135 ) ) ;
#9445 = EDGE_CURVE ( 'NONE', #2679, #5744, #11617, .T. ) ;
#9446 = CARTESIAN_POINT ( 'NONE',  ( -6.110905869600904872, 1.712176620043476140E-14, 2.600000000000000089 ) ) ;
#9447 = ORIENTED_EDGE ( 'NONE', *, *, #39769, .F. ) ;
#9448 = AXIS2_PLACEMENT_3D ( 'NONE', #33417, #51294, #12409 ) ;
#9449 = VECTOR ( 'NONE', #33411, 999.9999999999998863 ) ;
#9450 = ORIENTED_EDGE ( 'NONE', *, *, #2491, .F. ) ;
#9451 = CARTESIAN_POINT ( 'NONE',  ( -13.41816968106543939, -2.137015261443158565, 5.401210633846317499 ) ) ;
#9452 = DIRECTION ( 'NONE',  ( -0.6427681459581293666, -0.7660444431189770143, -0.005002170337467561935 ) ) ;
#9453 = CARTESIAN_POINT ( 'NONE',  ( -65.52441736963763219, 2.000000000000033751, -2.612833193080994043 ) ) ;
#9454 = DIRECTION ( 'NONE',  ( 0.9999697198139515519, 0.000000000000000000, 0.007781995580013368816 ) ) ;
#9455 = EDGE_CURVE ( 'NONE', #44660, #46401, #38575, .T. ) ;
#9456 = CARTESIAN_POINT ( 'NONE',  ( -12.15193928448664629, -0.1191753592594197858, 1.501852324026012209 ) ) ;
#9457 = CARTESIAN_POINT ( 'NONE',  ( 2.072287782118878319, 0.000000000000000000, -2.950529333540147015 ) ) ;
#9458 = VERTEX_POINT ( 'NONE', #3380 ) ;
#9459 = CARTESIAN_POINT ( 'NONE',  ( -14.01701317841955508, 0.000000000000000000, 2.326005055450897085 ) ) ;
#9460 = AXIS2_PLACEMENT_3D ( 'NONE', #20731, #42582, #39096 ) ;
#9461 = EDGE_CURVE ( 'NONE', #50536, #30787, #55903, .T. ) ;
#9462 = DIRECTION ( 'NONE',  ( 0.007781995580012663651, -3.146120232559066537E-19, -0.9999697198139514409 ) ) ;
#9463 = ORIENTED_EDGE ( 'NONE', *, *, #20282, .T. ) ;
#9464 = DIRECTION ( 'NONE',  ( 0.9321478471874540261, 0.000000000000000000, -0.3620778797217456546 ) ) ;
#9465 = CARTESIAN_POINT ( 'NONE',  ( -11.40636015113596180, 0.000000000000000000, 11.32142374880780089 ) ) ;
#9466 = VECTOR ( 'NONE', #37279, 999.9999999999998863 ) ;
#9467 = DIRECTION ( 'NONE',  ( 0.9999697198139515519, 0.000000000000000000, 0.007781995580013368816 ) ) ;
#9468 = EDGE_LOOP ( 'NONE', ( #50421, #27345, #51981, #2332 ) ) ;
#9469 = LINE ( 'NONE', #26795, #5825 ) ;
#9470 = EDGE_LOOP ( 'NONE', ( #50845, #2571, #40215, #46139 ) ) ;
#9471 = ORIENTED_EDGE ( 'NONE', *, *, #33380, .F. ) ;
#9472 = VERTEX_POINT ( 'NONE', #29791 ) ;
#9473 = VECTOR ( 'NONE', #41362, 999.9999999999998863 ) ;
#9474 = ORIENTED_EDGE ( 'NONE', *, *, #21577, .F. ) ;
#9475 = VECTOR ( 'NONE', #45110, 1000.000000000000227 ) ;
#9476 = CARTESIAN_POINT ( 'NONE',  ( -10.33233557835786698, -0.1191753592594185784, 5.578665668683107093 ) ) ;
#9478 = EDGE_CURVE ( 'NONE', #55415, #37296, #20102, .T. ) ;
#9477 = ORIENTED_EDGE ( 'NONE', *, *, #46452, .T. ) ;
#9479 = CARTESIAN_POINT ( 'NONE',  ( -29.86197018149027116, 0.000000000000000000, 8.281335066757780083 ) ) ;
#9480 = PLANE ( 'NONE',  #34990 ) ;
#9481 = VECTOR ( 'NONE', #14131, 1000.000000000000227 ) ;
#9482 = ORIENTED_EDGE ( 'NONE', *, *, #35865, .F. ) ;
#9483 = DIRECTION ( 'NONE',  ( -0.6427681459581293666, -0.7660444431189770143, -0.005002170337467561935 ) ) ;
#9484 = ORIENTED_EDGE ( 'NONE', *, *, #42603, .T. ) ;
#9485 = LINE ( 'NONE', #43007, #31168 ) ;
#9486 = ADVANCED_FACE ( 'NONE', ( #50778 ), #47087, .F. ) ;
#9487 = EDGE_LOOP ( 'NONE', ( #45102, #8415, #2271, #17562 ) ) ;
#9488 = VECTOR ( 'NONE', #50384, 999.9999999999998863 ) ;
#9489 = DIRECTION ( 'NONE',  ( 0.005002170337468016433, -0.7660444431189770143, -0.6427681459581293666 ) ) ;
#9490 = VECTOR ( 'NONE', #15322, 1000.000000000000227 ) ;
#9491 = EDGE_CURVE ( 'NONE', #21366, #12842, #28660, .T. ) ;
#9492 = CARTESIAN_POINT ( 'NONE',  ( -14.01623497886155256, -0.1191753592594197858, 2.226008083469502630 ) ) ;
#9493 = DIRECTION ( 'NONE',  ( -0.5364919789714478471, 0.6444004775717705469, -0.5449076811759709926 ) ) ;
#9494 = EDGE_CURVE ( 'NONE', #20216, #13812, #20951, .T. ) ;
#9495 = DIRECTION ( 'NONE',  ( -0.000000000000000000, -0.000000000000000000, 1.000000000000000000 ) ) ;
#9496 = LINE ( 'NONE', #26820, #16020 ) ;
#9497 = LINE ( 'NONE', #39874, #10180 ) ;
#9498 = ORIENTED_EDGE ( 'NONE', *, *, #37443, .F. ) ;
#9499 = ADVANCED_FACE ( 'NONE', ( #29196 ), #15861, .F. ) ;
#9500 = EDGE_CURVE ( 'NONE', #19178, #1128, #42278, .T. ) ;
#9501 = EDGE_CURVE ( 'NONE', #31769, #17110, #5068, .T. ) ;
#9502 = ORIENTED_EDGE ( 'NONE', *, *, #45300, .T. ) ;
#9503 = CARTESIAN_POINT ( 'NONE',  ( -19.98761758609199291, 0.000000000000000000, 5.234196989836540581 ) ) ;
#9504 = CARTESIAN_POINT ( 'NONE',  ( -9.908141408373387193, -0.1191753592594197858, 10.77908512878318703 ) ) ;
#9505 = DIRECTION ( 'NONE',  ( -0.5364919789714478471, 0.6444004775717705469, -0.5449076811759709926 ) ) ;
#9506 = AXIS2_PLACEMENT_3D ( 'NONE', #2167, #49043, #10145 ) ;
#9507 = LINE ( 'NONE', #48395, #6758 ) ;
#9508 = ORIENTED_EDGE ( 'NONE', *, *, #12919, .T. ) ;
#9509 = VECTOR ( 'NONE', #38695, 999.9999999999998863 ) ;
#9510 = CARTESIAN_POINT ( 'NONE',  ( -50.27554558092695913, 4.209026340267034705, 5.000000000000000000 ) ) ;
#9511 = DIRECTION ( 'NONE',  ( -0.5449076811759708816, 0.6444004775717707689, 0.5364919789714475140 ) ) ;
#9512 = ORIENTED_EDGE ( 'NONE', *, *, #2591, .T. ) ;
#9513 = PLANE ( 'NONE',  #44747 ) ;
#9514 = DIRECTION ( 'NONE',  ( 0.007781995580012663651, -3.146120232559066537E-19, -0.9999697198139514409 ) ) ;
#9515 = AXIS2_PLACEMENT_3D ( 'NONE', #15104, #6561, #24176 ) ;
#9516 = ORIENTED_EDGE ( 'NONE', *, *, #7252, .F. ) ;
#9517 = DIRECTION ( 'NONE',  ( 0.5449076811759707706, 0.6444004775717708799, -0.5364919789714476250 ) ) ;
#9518 = CARTESIAN_POINT ( 'NONE',  ( -17.49314540066396617, -4.241740624735662379, 3.540919126638463421 ) ) ;
#9519 = ADVANCED_FACE ( 'NONE', ( #56175 ), #47661, .F. ) ;
#9520 = VECTOR ( 'NONE', #31778, 1000.000000000000227 ) ;
#9521 = DIRECTION ( 'NONE',  ( 0.005961354470445682716, -0.6427876096865404731, -0.7660212471507180654 ) ) ;
#9522 = PLANE ( 'NONE',  #39588 ) ;
#9523 = ADVANCED_FACE ( 'NONE', ( #31166 ), #4235, .F. ) ;
#9524 = DIRECTION ( 'NONE',  ( 0.000000000000000000, 1.000000000000000000, 0.000000000000000000 ) ) ;
#9525 = ORIENTED_EDGE ( 'NONE', *, *, #11924, .T. ) ;
#9526 = AXIS2_PLACEMENT_3D ( 'NONE', #10041, #23111, #36179 ) ;
#9527 = AXIS2_PLACEMENT_3D ( 'NONE', #17381, #43508, #1476 ) ;
#9528 = EDGE_LOOP ( 'NONE', ( #25202, #23896, #13197, #16758 ) ) ;
#9529 = EDGE_CURVE ( 'NONE', #21349, #15160, #8780, .T. ) ;
#9530 = VECTOR ( 'NONE', #49852, 1000.000000000000227 ) ;
#9531 = AXIS2_PLACEMENT_3D ( 'NONE', #4728, #48153, #9562 ) ;
#9532 = CARTESIAN_POINT ( 'NONE',  ( -13.07066190154808361, 0.000000000000000000, 12.04713590736729678 ) ) ;
#9533 = CARTESIAN_POINT ( 'NONE',  ( 2.072287782118878319, 0.000000000000000000, -2.950529333540147015 ) ) ;
#9534 = CARTESIAN_POINT ( 'NONE',  ( -13.53673582514181106, 0.000000000000000000, 12.22817484722816772 ) ) ;
#9535 = VECTOR ( 'NONE', #7390, 1000.000000000000227 ) ;
#9536 = ADVANCED_FACE ( 'NONE', ( #22395 ), #17853, .F. ) ;
#9537 = CARTESIAN_POINT ( 'NONE',  ( -14.90247820238758969, 0.000000000000000000, 8.597759348604526508 ) ) ;
#9538 = CARTESIAN_POINT ( 'NONE',  ( -18.67619601524082285, 0.000000000000000000, 3.936400510096834893 ) ) ;
#9539 = ORIENTED_EDGE ( 'NONE', *, *, #42285, .F. ) ;
#9540 = CARTESIAN_POINT ( 'NONE',  ( -15.35417357620467449, 23.79353959847493272, -3.874970200383425656 ) ) ;
#9541 = PLANE ( 'NONE',  #50120 ) ;
#9542 = AXIS2_PLACEMENT_3D ( 'NONE', #36929, #18773, #44575 ) ;
#9543 = CARTESIAN_POINT ( 'NONE',  ( -13.48114463120078810, 0.000000000000000000, 5.084825810625885900 ) ) ;
#9544 = AXIS2_PLACEMENT_3D ( 'NONE', #1251, #18288, #36453 ) ;
#9545 = LINE ( 'NONE', #26038, #20585 ) ;
#9546 = ORIENTED_EDGE ( 'NONE', *, *, #12370, .F. ) ;
#9547 = LINE ( 'NONE', #43060, #12979 ) ;
#9548 = VERTEX_POINT ( 'NONE', #39423 ) ;
#9549 = DIRECTION ( 'NONE',  ( 0.000000000000000000, -1.000000000000000000, 0.000000000000000000 ) ) ;
#9550 = FACE_OUTER_BOUND ( 'NONE', #47521, .T. ) ;
#9551 = ORIENTED_EDGE ( 'NONE', *, *, #50151, .T. ) ;
#9552 = PLANE ( 'NONE',  #31763 ) ;
#9553 = ORIENTED_EDGE ( 'NONE', *, *, #5717, .T. ) ;
#9554 = AXIS2_PLACEMENT_3D ( 'NONE', #14363, #53788, #6658 ) ;
#9555 = EDGE_LOOP ( 'NONE', ( #35974, #52410, #10910, #2544 ) ) ;
#9556 = ORIENTED_EDGE ( 'NONE', *, *, #27613, .F. ) ;
#9557 = LINE ( 'NONE', #17027, #43811 ) ;
#9558 = EDGE_LOOP ( 'NONE', ( #38791, #44928, #15594 ) ) ;
#9559 = VECTOR ( 'NONE', #36874, 999.9999999999998863 ) ;
#9560 = ORIENTED_EDGE ( 'NONE', *, *, #3036, .T. ) ;
#9561 = DIRECTION ( 'NONE',  ( -0.7660212471507179544, -0.6427876096865405842, -0.005961354470445141482 ) ) ;
#9562 = DIRECTION ( 'NONE',  ( 0.6427681459581294776, -0.7660444431189769032, 0.005002170337467562802 ) ) ;
#9563 = AXIS2_PLACEMENT_3D ( 'NONE', #56102, #30257, #8690 ) ;
#9564 = ORIENTED_EDGE ( 'NONE', *, *, #16760, .T. ) ;
#9565 = B_SPLINE_CURVE_WITH_KNOTS ( 'NONE', 3,
 ( #16217, #12537, #21326, #12238 ),
 .UNSPECIFIED., .F., .F.,
 ( 4, 4 ),
 ( 0.000000000000000000, 0.0001352353904500101485 ),
 .UNSPECIFIED. ) ;
#9566 = ORIENTED_EDGE ( 'NONE', *, *, #7537, .F. ) ;
#9567 = CARTESIAN_POINT ( 'NONE',  ( -22.17952184443886665, 5.143464774974014553, 5.133107780287143207 ) ) ;
#9568 = ORIENTED_EDGE ( 'NONE', *, *, #28877, .T. ) ;
#9569 = AXIS2_PLACEMENT_3D ( 'NONE', #11595, #55043, #21222 ) ;
#9570 = ORIENTED_EDGE ( 'NONE', *, *, #45670, .F. ) ;
#9571 = VECTOR ( 'NONE', #40905, 999.9999999999998863 ) ;
#9572 = EDGE_CURVE ( 'NONE', #12044, #32426, #26933, .T. ) ;
#9573 = AXIS2_PLACEMENT_3D ( 'NONE', #9784, #25756, #23108 ) ;
#9574 = CARTESIAN_POINT ( 'NONE',  ( -13.46677436367437686, 0.000000000000000000, 3.238277294337062795 ) ) ;
#9575 = CARTESIAN_POINT ( 'NONE',  ( 4.912750499197525045, -1.131233082521085898, 2.162384853247616867 ) ) ;
#9576 = FACE_OUTER_BOUND ( 'NONE', #48150, .T. ) ;
#9577 = CARTESIAN_POINT ( 'NONE',  ( -15.13495153988577968, 0.000000000000000000, 12.76973526769478084 ) ) ;
#9578 = ORIENTED_EDGE ( 'NONE', *, *, #31248, .F. ) ;
#9579 = CARTESIAN_POINT ( 'NONE',  ( -5.105985705592273050, 4.998162406247122824, 5.201711823720286176 ) ) ;
#9580 = ORIENTED_EDGE ( 'NONE', *, *, #48216, .F. ) ;
#9581 = AXIS2_PLACEMENT_3D ( 'NONE', #41894, #40807, #33128 ) ;
#9582 = ADVANCED_FACE ( 'NONE', ( #30883 ), #43400, .F. ) ;
#9583 = EDGE_CURVE ( 'NONE', #4850, #26435, #9610, .T. ) ;
#9584 = AXIS2_PLACEMENT_3D ( 'NONE', #48525, #1376, #36302 ) ;
#9585 = CARTESIAN_POINT ( 'NONE',  ( -17.89891568791274068, 0.000000000000000000, 9.682436588653759557 ) ) ;
#9586 = EDGE_CURVE ( 'NONE', #29013, #3202, #52476, .T. ) ;
#9587 = VECTOR ( 'NONE', #51775, 1000.000000000000114 ) ;
#9588 = DIRECTION ( 'NONE',  ( 0.007781995580012663651, -3.146120232559066537E-19, -0.9999697198139514409 ) ) ;
#9589 = AXIS2_PLACEMENT_3D ( 'NONE', #9433, #44083, #27047 ) ;
#9590 = DIRECTION ( 'NONE',  ( 0.000000000000000000, -0.000000000000000000, -1.000000000000000000 ) ) ;
#9591 = CARTESIAN_POINT ( 'NONE',  ( -18.80938876144721306, 0.000000000000000000, 7.259352601608363820 ) ) ;
#9592 = CARTESIAN_POINT ( 'NONE',  ( 5.518152842597062069, -1.042152011631011899, -2.501942471198983942 ) ) ;
#9593 = DIRECTION ( 'NONE',  ( -0.5364919789714478471, 0.6444004775717705469, -0.5449076811759709926 ) ) ;
#9594 = LINE ( 'NONE', #39949, #28597 ) ;
#9595 = VERTEX_POINT ( 'NONE', #21806 ) ;
#9596 = DIRECTION ( 'NONE',  ( 0.007781995580012662783, 0.000000000000000000, -0.9999697198139514409 ) ) ;
#9597 = CARTESIAN_POINT ( 'NONE',  ( -50.45472955569960760, 3.742236127018431890, 5.000000000000000000 ) ) ;
#9598 = DIRECTION ( 'NONE',  ( 0.007781995580012663651, -3.146120232559066537E-19, -0.9999697198139514409 ) ) ;
#9599 = CARTESIAN_POINT ( 'NONE',  ( -20.54204810873173415, 0.000000000000000000, 4.860550213503115558 ) ) ;
#9600 = CARTESIAN_POINT ( 'NONE',  ( -37.11431328563478615, 9.498266272062682702, -4.936536869034685360 ) ) ;
#9601 = DIRECTION ( 'NONE',  ( -0.005002170337468016433, -0.7660444431189770143, 0.6427681459581293666 ) ) ;
#9602 = DIRECTION ( 'NONE',  ( 0.007781995580012662783, 0.000000000000000000, -0.9999697198139514409 ) ) ;
#9603 = VECTOR ( 'NONE', #35872, 1000.000000000000227 ) ;
#9604 = DIRECTION ( 'NONE',  ( -0.6427681459581293666, -0.7660444431189770143, -0.005002170337467561935 ) ) ;
#9605 = AXIS2_PLACEMENT_3D ( 'NONE', #31805, #48267, #17925 ) ;
#9606 = VERTEX_POINT ( 'NONE', #52197 ) ;
#9607 = EDGE_CURVE ( 'NONE', #12905, #53740, #48192, .T. ) ;
#9608 = LINE ( 'NONE', #1339, #42020 ) ;
#9609 = DIRECTION ( 'NONE',  ( -0.005002170337468016433, -0.7660444431189770143, 0.6427681459581293666 ) ) ;
#9610 = LINE ( 'NONE', #4498, #30017 ) ;
#9611 = VECTOR ( 'NONE', #44231, 1000.000000000000227 ) ;
#9612 = EDGE_CURVE ( 'NONE', #19197, #4449, #39127, .T. ) ;
#9613 = DIRECTION ( 'NONE',  ( -0.6427681459581293666, -0.7660444431189770143, -0.005002170337467561935 ) ) ;
#9614 = AXIS2_PLACEMENT_3D ( 'NONE', #21853, #7984, #51115 ) ;
#9615 = LINE ( 'NONE', #26630, #45707 ) ;
#9616 = FACE_OUTER_BOUND ( 'NONE', #17383, .T. ) ;
#9617 = CARTESIAN_POINT ( 'NONE',  ( -25.20278734466900517, 0.000000000000000000, 6.670939612111840944 ) ) ;
#9618 = EDGE_CURVE ( 'NONE', #6876, #53403, #17260, .T. ) ;
#9619 = AXIS2_PLACEMENT_3D ( 'NONE', #4597, #11985, #46935 ) ;
#9620 = LINE ( 'NONE', #52483, #28821 ) ;
#9621 = AXIS2_PLACEMENT_3D ( 'NONE', #12070, #38783, #55507 ) ;
#9622 = CARTESIAN_POINT ( 'NONE',  ( -18.61382527010571764, 0.000000000000000000, 7.830212647944921223 ) ) ;
#9623 = VECTOR ( 'NONE', #50907, 1000.000000000000227 ) ;
#9624 = VERTEX_POINT ( 'NONE', #788 ) ;
#9625 = VECTOR ( 'NONE', #6701, 1000.000000000000227 ) ;
#9626 = AXIS2_PLACEMENT_3D ( 'NONE', #42628, #42912, #47165 ) ;
#9627 = VERTEX_POINT ( 'NONE', #17551 ) ;
#9628 = AXIS2_PLACEMENT_3D ( 'NONE', #7270, #54991, #55524 ) ;
#9629 = ORIENTED_EDGE ( 'NONE', *, *, #18986, .T. ) ;
#9630 = VERTEX_POINT ( 'NONE', #13840 ) ;
#9631 = ORIENTED_EDGE ( 'NONE', *, *, #52659, .F. ) ;
#9632 = LINE ( 'NONE', #26949, #45058 ) ;
#9633 = CARTESIAN_POINT ( 'NONE',  ( -19.82178941147031637, -0.1191753592594188838, 6.612812754151981665 ) ) ;
#9634 = ORIENTED_EDGE ( 'NONE', *, *, #35877, .T. ) ;
#9635 = ORIENTED_EDGE ( 'NONE', *, *, #42688, .T. ) ;
#9636 = VECTOR ( 'NONE', #41159, 1000.000000000000227 ) ;
#9637 = CARTESIAN_POINT ( 'NONE',  ( -68.21250092108449792, -9.516813072189039602, -7.380886937840050344 ) ) ;
#9638 = VERTEX_POINT ( 'NONE', #44245 ) ;
#9639 = DIRECTION ( 'NONE',  ( -0.6427681459581293666, -0.7660444431189770143, -0.005002170337467561935 ) ) ;
#9640 = CARTESIAN_POINT ( 'NONE',  ( -16.99924723426068951, 0.000000000000000000, 13.49389102713827171 ) ) ;
#9641 = VERTEX_POINT ( 'NONE', #34882 ) ;
#9642 = VECTOR ( 'NONE', #36199, 999.9999999999998863 ) ;
#9643 = CARTESIAN_POINT ( 'NONE',  ( -10.11544336623486728, -9.746244815904656633, 0.7108081496845154446 ) ) ;
#9645 = EDGE_LOOP ( 'NONE', ( #26157, #5518, #41978, #39520 ) ) ;
#9644 = ADVANCED_FACE ( 'NONE', ( #47940 ), #51630, .F. ) ;
#9646 = CARTESIAN_POINT ( 'NONE',  ( -13.58766790975075089, -0.1191753592594177180, 5.922663989564801668 ) ) ;
#9647 = AXIS2_PLACEMENT_3D ( 'NONE', #46219, #54746, #23809 ) ;
#9648 = DIRECTION ( 'NONE',  ( -0.5364919789714478471, 0.6444004775717705469, -0.5449076811759709926 ) ) ;
#9649 = ADVANCED_FACE ( 'NONE', ( #43654 ), #48491, .F. ) ;
#9650 = EDGE_CURVE ( 'NONE', #51780, #22414, #34581, .T. ) ;
#9651 = DIRECTION ( 'NONE',  ( 0.9999697198139515519, 0.000000000000000000, 0.007781995580013368816 ) ) ;
#9652 = CARTESIAN_POINT ( 'NONE',  ( -9.542064456761055524, 0.000000000000000000, 10.59726798936431180 ) ) ;
#9653 = VECTOR ( 'NONE', #6784, 999.9999999999998863 ) ;
#9654 = VERTEX_POINT ( 'NONE', #5904 ) ;
#9655 = PLANE ( 'NONE',  #22200 ) ;
#9656 = PLANE ( 'NONE',  #50139 ) ;
#9657 = LINE ( 'NONE', #47975, #10340 ) ;
#9658 = ORIENTED_EDGE ( 'NONE', *, *, #9103, .F. ) ;
#9659 = CARTESIAN_POINT ( 'NONE',  ( -17.76939998132051812, -0.1191753592594194527, 5.890120783652720071 ) ) ;
#9660 = ORIENTED_EDGE ( 'NONE', *, *, #29182, .F. ) ;
#9661 = VECTOR ( 'NONE', #55067, 1000.000000000000114 ) ;
#9662 = VECTOR ( 'NONE', #41804, 1000.000000000000000 ) ;
#9663 = DIRECTION ( 'NONE',  ( 0.007781995580012663651, -3.146120232559066537E-19, -0.9999697198139514409 ) ) ;
#9664 = CARTESIAN_POINT ( 'NONE',  ( -17.93139508144814442, 0.000000000000000000, 13.85596890686001537 ) ) ;
#9665 = CARTESIAN_POINT ( 'NONE',  ( -20.63663879154963965, 20.74370688441071664, 4.329123301634322907 ) ) ;
#9666 = LINE ( 'NONE', #26981, #20499 ) ;
#9667 = CARTESIAN_POINT ( 'NONE',  ( -12.09453844680409951, 0.000000000000000000, 6.034286896408231904 ) ) ;
#9668 = CARTESIAN_POINT ( 'NONE',  ( 2.072287782118878319, 0.000000000000000000, -2.950529333540147015 ) ) ;
#9669 = CARTESIAN_POINT ( 'NONE',  ( 2.072287782118878319, 0.000000000000000000, -2.950529333540147015 ) ) ;
#9670 = VECTOR ( 'NONE', #27793, 999.9999999999998863 ) ;
#9671 = VECTOR ( 'NONE', #7212, 999.9999999999998863 ) ;
#9672 = CARTESIAN_POINT ( 'NONE',  ( -15.42609712257811339, -0.1191753592594191752, 3.323032419688414230 ) ) ;
#9673 = CARTESIAN_POINT ( 'NONE',  ( -60.88973930853472183, 7.404220597074748333, 2.999999999999993339 ) ) ;
#9674 = EDGE_LOOP ( 'NONE', ( #43497, #28710, #27943, #40773 ) ) ;
#9675 = CARTESIAN_POINT ( 'NONE',  ( -19.16618472534906203, -0.1191753592594172323, 6.248582751606454266 ) ) ;
#9676 = LINE ( 'NONE', #17136, #55751 ) ;
#9677 = PLANE ( 'NONE',  #41745 ) ;
#9678 = LINE ( 'NONE', #44304, #38538 ) ;
#9679 = CARTESIAN_POINT ( 'NONE',  ( -8.380317325580694643, 0.000000000000000000, 6.432523893810073723 ) ) ;
#9680 = ADVANCED_FACE ( 'NONE', ( #22929 ), #49044, .F. ) ;
#9681 = DIRECTION ( 'NONE',  ( 0.000000000000000000, -0.000000000000000000, -1.000000000000000000 ) ) ;
#9682 = DIRECTION ( 'NONE',  ( -0.5364919789714478471, 0.6444004775717705469, -0.5449076811759709926 ) ) ;
#9683 = AXIS2_PLACEMENT_3D ( 'NONE', #1097, #4540, #47720 ) ;
#9684 = EDGE_LOOP ( 'NONE', ( #4372, #12697, #11855, #52442 ) ) ;
#9685 = ORIENTED_EDGE ( 'NONE', *, *, #24653, .F. ) ;
#9686 = ADVANCED_FACE ( 'NONE', ( #15258 ), #10731, .F. ) ;
#9687 = CARTESIAN_POINT ( 'NONE',  ( -18.36199618563782821, 0.000000000000000000, 9.478826732922961185 ) ) ;
#9688 = LINE ( 'NONE', #5414, #15947 ) ;
#9689 = VECTOR ( 'NONE', #30692, 999.9999999999998863 ) ;
#9690 = VERTEX_POINT ( 'NONE', #10975 ) ;
#9691 = FACE_OUTER_BOUND ( 'NONE', #29715, .T. ) ;
#9692 = AXIS2_PLACEMENT_3D ( 'NONE', #28238, #27136, #48990 ) ;
#9693 = ADVANCED_FACE ( 'NONE', ( #49331 ), #32573, .F. ) ;
#9694 = VERTEX_POINT ( 'NONE', #10447 ) ;
#9695 = LINE ( 'NONE', #39203, #4811 ) ;
#9696 = VECTOR ( 'NONE', #20390, 999.9999999999998863 ) ;
#9697 = EDGE_LOOP ( 'NONE', ( #17721, #20213, #10023, #5313 ) ) ;
#9698 = ORIENTED_EDGE ( 'NONE', *, *, #45286, .T. ) ;
#9699 = ORIENTED_EDGE ( 'NONE', *, *, #2626, .T. ) ;
#9700 = LINE ( 'NONE', #44583, #27526 ) ;
#9701 = CARTESIAN_POINT ( 'NONE',  ( -20.54204810873173415, 0.000000000000000000, 4.860550213503115558 ) ) ;
#9702 = CYLINDRICAL_SURFACE ( 'NONE', #40281, 2.749999999999997780 ) ;
#9703 = VECTOR ( 'NONE', #55294, 999.9999999999998863 ) ;
#9704 = DIRECTION ( 'NONE',  ( 0.9999697198139515519, 0.000000000000000000, 0.007781995580013368816 ) ) ;
#9705 = ORIENTED_EDGE ( 'NONE', *, *, #24727, .T. ) ;
#9706 = ORIENTED_EDGE ( 'NONE', *, *, #42752, .F. ) ;
#9707 = EDGE_CURVE ( 'NONE', #14368, #8086, #9886, .T. ) ;
#9708 = VECTOR ( 'NONE', #36570, 999.9999999999998863 ) ;
#9709 = VECTOR ( 'NONE', #50222, 1000.000000000000227 ) ;
#9710 = DIRECTION ( 'NONE',  ( 0.7660212471507180654, -0.6427876096865404731, 0.005961354470445141482 ) ) ;
#9711 = ORIENTED_EDGE ( 'NONE', *, *, #55949, .T. ) ;
#9712 = DIRECTION ( 'NONE',  ( -0.6427681459581293666, -0.7660444431189770143, -0.005002170337467561935 ) ) ;
#9713 = EDGE_CURVE ( 'NONE', #49012, #37392, #53334, .T. ) ;
#9714 = VERTEX_POINT ( 'NONE', #53579 ) ;
#9715 = FACE_OUTER_BOUND ( 'NONE', #53712, .T. ) ;
#9716 = FACE_OUTER_BOUND ( 'NONE', #30805, .T. ) ;
#9717 = ORIENTED_EDGE ( 'NONE', *, *, #54596, .T. ) ;
#9718 = EDGE_CURVE ( 'NONE', #32655, #8255, #49875, .T. ) ;
#9719 = CARTESIAN_POINT ( 'NONE',  ( -24.57312748012714820, 18.34675972927921350, -4.549864808573585329 ) ) ;
#9720 = VERTEX_POINT ( 'NONE', #45342 ) ;
#9721 = EDGE_CURVE ( 'NONE', #45468, #2367, #1886, .T. ) ;
#9722 = VECTOR ( 'NONE', #48599, 1000.000000000000227 ) ;
#9723 = LINE ( 'NONE', #31279, #8234 ) ;
#9724 = ORIENTED_EDGE ( 'NONE', *, *, #45985, .T. ) ;
#9725 = DIRECTION ( 'NONE',  ( 0.5364919789714477361, 0.6444004775717706579, 0.5449076811759711036 ) ) ;
#9726 = DIRECTION ( 'NONE',  ( -0.005961354470445682716, -0.6427876096865404731, 0.7660212471507180654 ) ) ;
#9727 = LINE ( 'NONE', #36376, #37387 ) ;
#9728 = EDGE_LOOP ( 'NONE', ( #9187, #17400, #10876, #33055 ) ) ;
#9729 = CARTESIAN_POINT ( 'NONE',  ( 2.072287782118878319, 0.000000000000000000, -2.950529333540147015 ) ) ;
#9730 = LINE ( 'NONE', #1469, #41019 ) ;
#9731 = AXIS2_PLACEMENT_3D ( 'NONE', #16881, #48351, #13173 ) ;
#9732 = LINE ( 'NONE', #19057, #39432 ) ;
#9733 = CARTESIAN_POINT ( 'NONE',  ( -56.32517369257367079, 3.868430646962533359, -2.183859404458766917 ) ) ;
#9734 = DIRECTION ( 'NONE',  ( -0.5364919789714478471, 0.6444004775717705469, -0.5449076811759709926 ) ) ;
#9735 = PLANE ( 'NONE',  #45162 ) ;
#9736 = EDGE_CURVE ( 'NONE', #30096, #49088, #44496, .T. ) ;
#9737 = AXIS2_PLACEMENT_3D ( 'NONE', #28575, #2707, #37660 ) ;
#9738 = CARTESIAN_POINT ( 'NONE',  ( -14.61647978877039478, 3.848249166794009746, 8.874490732104780122 ) ) ;
#9739 = ORIENTED_EDGE ( 'NONE', *, *, #9159, .F. ) ;
#9740 = LINE ( 'NONE', #36678, #11664 ) ;
#9741 = DIRECTION ( 'NONE',  ( -1.000000000000000000, 0.000000000000000000, 0.000000000000000000 ) ) ;
#9742 = DIRECTION ( 'NONE',  ( 0.005961354470445682716, -0.6427876096865404731, -0.7660212471507180654 ) ) ;
#9743 = ORIENTED_EDGE ( 'NONE', *, *, #55021, .F. ) ;
#9744 = PLANE ( 'NONE',  #52896 ) ;
#9745 = LINE ( 'NONE', #14289, #7301 ) ;
#9746 = APPLICATION_CONTEXT ( 'automotive_design' ) ;
#9747 = ORIENTED_EDGE ( 'NONE', *, *, #32751, .T. ) ;
#9748 = CARTESIAN_POINT ( 'NONE',  ( -13.01519007997042188, 0.000000000000000000, 4.919125963098919918 ) ) ;
#9749 = VECTOR ( 'NONE', #15771, 1000.000000000000227 ) ;
#9750 = DIRECTION ( 'NONE',  ( 0.7660212471507180654, -0.6427876096865404731, 0.005961354470445141482 ) ) ;
#9751 = CARTESIAN_POINT ( 'NONE',  ( -14.94916102560700821, 0.000000000000000000, 2.688082935172642962 ) ) ;
#9752 = CARTESIAN_POINT ( 'NONE',  ( 2.072287782118878319, 0.000000000000000000, -2.950529333540147015 ) ) ;
#9753 = EDGE_LOOP ( 'NONE', ( #22230, #18541, #46254, #39284 ) ) ;
#9754 = ORIENTED_EDGE ( 'NONE', *, *, #20347, .F. ) ;
#9755 = CARTESIAN_POINT ( 'NONE',  ( -18.19747506107908563, 0.000000000000000000, 14.03856424583689311 ) ) ;
#9756 = CARTESIAN_POINT ( 'NONE',  ( -16.53317331066696383, 0.000000000000000000, 13.31285208727739899 ) ) ;
#9757 = CARTESIAN_POINT ( 'NONE',  ( -21.47419595591918906, 0.000000000000000000, 5.222628093224860102 ) ) ;
#9758 = DIRECTION ( 'NONE',  ( 0.007781995580012662783, 0.000000000000000000, -0.9999697198139514409 ) ) ;
#9759 = DIRECTION ( 'NONE',  ( 0.005961354470445682716, -0.6427876096865404731, -0.7660212471507180654 ) ) ;
#9760 = CARTESIAN_POINT ( 'NONE',  ( -24.27063949748155380, 0.000000000000000000, 6.308861732390097288 ) ) ;
#9761 = EDGE_CURVE ( 'NONE', #11534, #36770, #41379, .T. ) ;
#9762 = ORIENTED_EDGE ( 'NONE', *, *, #42814, .T. ) ;
#9763 = DIRECTION ( 'NONE',  ( 0.5449076811759707706, 0.6444004775717708799, -0.5364919789714476250 ) ) ;
#9764 = CARTESIAN_POINT ( 'NONE',  ( -20.81724602552766612, 3.524445264749009876, 4.655608788014395927 ) ) ;
#9765 = VERTEX_POINT ( 'NONE', #14687 ) ;
#9766 = PLANE ( 'NONE',  #31988 ) ;
#9767 = CARTESIAN_POINT ( 'NONE',  ( -18.81956732107907015, 0.000000000000000000, 8.567275655344447571 ) ) ;
#9768 = CARTESIAN_POINT ( 'NONE',  ( -15.50102849149811135, -0.1191753592594197858, 12.95155240711365430 ) ) ;
#9769 = ADVANCED_FACE ( 'NONE', ( #36849 ), #18378, .F. ) ;
#9770 = ORIENTED_EDGE ( 'NONE', *, *, #25414, .F. ) ;
#9771 = CARTESIAN_POINT ( 'NONE',  ( -11.67244013076689946, 0.000000000000000000, 11.50401908778467863 ) ) ;
#9772 = ORIENTED_EDGE ( 'NONE', *, *, #42575, .F. ) ;
#9773 = EDGE_CURVE ( 'NONE', #31783, #27675, #1636, .T. ) ;
#9774 = EDGE_CURVE ( 'NONE', #8247, #14910, #53858, .T. ) ;
#9775 = VERTEX_POINT ( 'NONE', #23498 ) ;
#9776 = VECTOR ( 'NONE', #18684, 999.9999999999998863 ) ;
#9777 = ORIENTED_EDGE ( 'NONE', *, *, #43530, .T. ) ;
#9778 = ORIENTED_EDGE ( 'NONE', *, *, #15125, .T. ) ;
#9779 = LINE ( 'NONE', #19101, #14855 ) ;
#9780 = ADVANCED_FACE ( 'NONE', ( #23756 ), #53035, .F. ) ;
#9781 = B_SPLINE_CURVE_WITH_KNOTS ( 'NONE', 3,
 ( #47430, #30413, #30699, #13628 ),
 .UNSPECIFIED., .F., .F.,
 ( 4, 4 ),
 ( 0.0001144323540671334324, 0.0003537324766284092063 ),
 .UNSPECIFIED. ) ;
#9782 = ORIENTED_EDGE ( 'NONE', *, *, #9736, .F. ) ;
#9783 = LINE ( 'NONE', #31049, #13174 ) ;
#9784 = CARTESIAN_POINT ( 'NONE',  ( -14.01545677930355183, 0.000000000000000000, 2.126011111488108174 ) ) ;
#9785 = VECTOR ( 'NONE', #48625, 999.9999999999998863 ) ;
#9786 = ORIENTED_EDGE ( 'NONE', *, *, #25713, .F. ) ;
#9787 = CARTESIAN_POINT ( 'NONE',  ( -20.54204810873173415, 0.000000000000000000, 4.860550213503115558 ) ) ;
#9788 = EDGE_CURVE ( 'NONE', #26765, #2694, #19504, .T. ) ;
#9789 = EDGE_LOOP ( 'NONE', ( #5837, #19610, #9777, #27933 ) ) ;
#9790 = PLANE ( 'NONE',  #9526 ) ;
#9791 = ORIENTED_EDGE ( 'NONE', *, *, #29963, .F. ) ;
#9792 = EDGE_CURVE ( 'NONE', #29905, #35206, #31477, .T. ) ;
#9793 = FACE_OUTER_BOUND ( 'NONE', #34225, .T. ) ;
#9794 = DIRECTION ( 'NONE',  ( 0.5449076811759707706, 0.6444004775717708799, -0.5364919789714476250 ) ) ;
#9795 = CARTESIAN_POINT ( 'NONE',  ( -23.44701637808619665, 18.93456746265863799, 4.495868649597294819 ) ) ;
#9796 = DIRECTION ( 'NONE',  ( -0.9999697198139514409, -0.000000000000000000, -0.007781995580013368816 ) ) ;
#9797 = CARTESIAN_POINT ( 'NONE',  ( -23.33771345073609638, -0.1191753592594197858, 5.846786880686956955 ) ) ;
#9798 = EDGE_LOOP ( 'NONE', ( #50413, #38046, #39806, #6936 ) ) ;
#9799 = ADVANCED_FACE ( 'NONE', ( #36027 ), #54685, .F. ) ;
#9800 = ORIENTED_EDGE ( 'NONE', *, *, #18609, .F. ) ;
#9801 = FACE_OUTER_BOUND ( 'NONE', #27058, .T. ) ;
#9802 = DIRECTION ( 'NONE',  ( 0.000000000000000000, -0.000000000000000000, -1.000000000000000000 ) ) ;
#9803 = CARTESIAN_POINT ( 'NONE',  ( -24.26908309836554878, 0.000000000000000000, 6.108867788427308376 ) ) ;
#9804 = ADVANCED_FACE ( 'NONE', ( #51292 ), #41634, .F. ) ;
#9805 = CARTESIAN_POINT ( 'NONE',  ( -17.76284804600266654, 0.4483081953215033444, 3.567321762835300003 ) ) ;
#9806 = ORIENTED_EDGE ( 'NONE', *, *, #51779, .F. ) ;
#9807 = FACE_OUTER_BOUND ( 'NONE', #24835, .T. ) ;
#9808 = PLANE ( 'NONE',  #41380 ) ;
#9809 = ORIENTED_EDGE ( 'NONE', *, *, #47714, .F. ) ;
#9810 = DIRECTION ( 'NONE',  ( 0.005961354470445682716, -0.6427876096865404731, -0.7660212471507180654 ) ) ;
#9811 = FACE_OUTER_BOUND ( 'NONE', #16558, .T. ) ;
#9812 = ORIENTED_EDGE ( 'NONE', *, *, #5926, .F. ) ;
#9813 = FACE_OUTER_BOUND ( 'NONE', #29749, .T. ) ;
#9814 = LINE ( 'NONE', #23143, #38759 ) ;
#9815 = PLANE ( 'NONE',  #22307 ) ;
#9816 = DIRECTION ( 'NONE',  ( 0.007781995580012663651, -3.146120232559066537E-19, -0.9999697198139514409 ) ) ;
#9817 = DIRECTION ( 'NONE',  ( -0.005961354470445682716, -0.6427876096865404731, 0.7660212471507180654 ) ) ;
#9818 = ORIENTED_EDGE ( 'NONE', *, *, #31507, .T. ) ;
#9819 = EDGE_LOOP ( 'NONE', ( #46249, #45487, #15328, #12107 ) ) ;
#9820 = FACE_OUTER_BOUND ( 'NONE', #18848, .T. ) ;
#9821 = CARTESIAN_POINT ( 'NONE',  ( -18.15338008115919521, 0.000000000000000000, 8.372454022265671369 ) ) ;
#9822 = DIRECTION ( 'NONE',  ( -0.5364919789714478471, 0.6444004775717705469, -0.5449076811759709926 ) ) ;
#9823 = AXIS2_PLACEMENT_3D ( 'NONE', #50366, #50648, #41825 ) ;
#9824 = DIRECTION ( 'NONE',  ( -0.6427681459581293666, -0.7660444431189770143, -0.005002170337467561935 ) ) ;
#9825 = LINE ( 'NONE', #31678, #4914 ) ;
#9826 = ADVANCED_FACE ( 'NONE', ( #55255 ), #42206, .F. ) ;
#9827 = ORIENTED_EDGE ( 'NONE', *, *, #11894, .F. ) ;
#9828 = DIRECTION ( 'NONE',  ( 0.7660212471507180654, -0.6427876096865404731, 0.005961354470445141482 ) ) ;
#9829 = CARTESIAN_POINT ( 'NONE',  ( -16.94823507309948596, -3.594132820645662196, 3.349919529729364687 ) ) ;
#9830 = CARTESIAN_POINT ( 'NONE',  ( -24.27063949748155380, 0.000000000000000000, 6.308861732390097288 ) ) ;
#9831 = CARTESIAN_POINT ( 'NONE',  ( -19.98474353258670888, 0.000000000000000000, 4.864887286578777115 ) ) ;
#9832 = ORIENTED_EDGE ( 'NONE', *, *, #55323, .T. ) ;
#9833 = CARTESIAN_POINT ( 'NONE',  ( -7.626921145403491309, -9.440094667004895967, 6.180928759870859324 ) ) ;
#9834 = ORIENTED_EDGE ( 'NONE', *, *, #27505, .T. ) ;
#9835 = LINE ( 'NONE', #35130, #33168 ) ;
#9836 = EDGE_CURVE ( 'NONE', #35036, #33995, #33413, .T. ) ;
#9837 = EDGE_CURVE ( 'NONE', #41210, #27148, #54997, .T. ) ;
#9838 = FACE_OUTER_BOUND ( 'NONE', #35666, .T. ) ;
#9839 = VERTEX_POINT ( 'NONE', #29426 ) ;
#9840 = LINE ( 'NONE', #53289, #18127 ) ;
#9841 = ORIENTED_EDGE ( 'NONE', *, *, #55015, .F. ) ;
#9842 = EDGE_CURVE ( 'NONE', #49209, #10401, #2470, .T. ) ;
#9843 = ORIENTED_EDGE ( 'NONE', *, *, #50487, .F. ) ;
#9844 = ORIENTED_EDGE ( 'NONE', *, *, #19698, .T. ) ;
#9845 = DIRECTION ( 'NONE',  ( -0.005961354470445682716, -0.6427876096865404731, 0.7660212471507180654 ) ) ;
#9846 = ORIENTED_EDGE ( 'NONE', *, *, #38868, .T. ) ;
#9847 = ORIENTED_EDGE ( 'NONE', *, *, #30952, .F. ) ;
#9848 = CARTESIAN_POINT ( 'NONE',  ( -11.17101276013249134, 0.000000000000000000, 6.780138126459778647 ) ) ;
#9849 = CARTESIAN_POINT ( 'NONE',  ( -14.25207316155825765, -5.375054281893166142, 2.245817962481531538 ) ) ;
#9850 = ORIENTED_EDGE ( 'NONE', *, *, #2551, .F. ) ;
#9851 = ORIENTED_EDGE ( 'NONE', *, *, #49432, .T. ) ;
#9852 = DIRECTION ( 'NONE',  ( -0.5449076811759708816, 0.6444004775717707689, 0.5364919789714475140 ) ) ;
#9853 = EDGE_CURVE ( 'NONE', #33003, #39170, #11811, .T. ) ;
#9854 = ORIENTED_EDGE ( 'NONE', *, *, #37587, .T. ) ;
#9855 = VERTEX_POINT ( 'NONE', #50720 ) ;
#9856 = EDGE_CURVE ( 'NONE', #29873, #41167, #3312, .T. ) ;
#9857 = FACE_OUTER_BOUND ( 'NONE', #2100, .T. ) ;
#9858 = FACE_OUTER_BOUND ( 'NONE', #45814, .T. ) ;
#9859 = EDGE_CURVE ( 'NONE', #32191, #49975, #53954, .T. ) ;
#9860 = DIRECTION ( 'NONE',  ( 0.3535533905932738974, -0.6123724356957929160, 0.7071067811865487940 ) ) ;
#9861 = CARTESIAN_POINT ( 'NONE',  ( -17.87471697247878311, -4.079838673713161334, 10.32078915421988086 ) ) ;
#9862 = VERTEX_POINT ( 'NONE', #24881 ) ;
#9863 = PLANE ( 'NONE',  #31914 ) ;
#9864 = VERTEX_POINT ( 'NONE', #37948 ) ;
#9865 = EDGE_CURVE ( 'NONE', #3535, #28311, #56017, .T. ) ;
#9866 = VECTOR ( 'NONE', #40923, 999.9999999999998863 ) ;
#9867 = DIRECTION ( 'NONE',  ( 0.5449076811759707706, 0.6444004775717708799, -0.5364919789714476250 ) ) ;
#9868 = CARTESIAN_POINT ( 'NONE',  ( -23.23471500290295921, 19.24370688441070953, 4.480778704491060971 ) ) ;
#9869 = CARTESIAN_POINT ( 'NONE',  ( -17.23141079360358674, 0.000000000000000000, 9.318299196280007024 ) ) ;
#9870 = PLANE ( 'NONE',  #5883 ) ;
#9871 = CARTESIAN_POINT ( 'NONE',  ( -22.40478740399063895, 0.000000000000000000, 5.384712028983816623 ) ) ;
#9872 = FACE_OUTER_BOUND ( 'NONE', #25632, .T. ) ;
#9873 = EDGE_LOOP ( 'NONE', ( #2340, #5994, #23183, #31447 ) ) ;
#9874 = FACE_OUTER_BOUND ( 'NONE', #55620, .T. ) ;
#9875 = ORIENTED_EDGE ( 'NONE', *, *, #14772, .F. ) ;
#9876 = DIRECTION ( 'NONE',  ( 0.000000000000000000, -0.000000000000000000, -1.000000000000000000 ) ) ;
#9877 = LINE ( 'NONE', #6186, #14195 ) ;
#9878 = DIRECTION ( 'NONE',  ( -0.6427681459581293666, -0.7660444431189770143, -0.005002170337467561935 ) ) ;
#9879 = CARTESIAN_POINT ( 'NONE',  ( -38.32071399784587840, 8.801750496117048073, -4.953405659155169616 ) ) ;
#9880 = DIRECTION ( 'NONE',  ( 0.9999697198139515519, 0.000000000000000000, 0.007781995580013368816 ) ) ;
#9881 = LINE ( 'NONE', #15254, #15057 ) ;
#9882 = DIRECTION ( 'NONE',  ( 0.6427681459581294776, -0.7660444431189769032, 0.005002170337467562802 ) ) ;
#9883 = ORIENTED_EDGE ( 'NONE', *, *, #38355, .F. ) ;
#9884 = DIRECTION ( 'NONE',  ( -0.5364919789714478471, 0.6444004775717705469, -0.5449076811759709926 ) ) ;
#9885 = CARTESIAN_POINT ( 'NONE',  ( -18.86354292863559579, 0.000000000000000000, 14.21804678658176080 ) ) ;
#9886 = LINE ( 'NONE', #44791, #1897 ) ;
#9887 = EDGE_CURVE ( 'NONE', #52348, #235, #20042, .T. ) ;
#9888 = B_SPLINE_CURVE_WITH_KNOTS ( 'NONE', 3,
 ( #25356, #42658, #21076, #42947, #4053, #27039, #30745, #23344, #35285, #22507, #641, #18808, #27591, #17962 ),
 .UNSPECIFIED., .F., .F.,
 ( 4, 2, 2, 2, 2, 2, 4 ),
 ( 1.404617285391336434E-17, 0.0008437472854879493047, 0.001265620928231936696, 0.001687494570975924197, 0.002109368213719911046, 0.002531241856463898980, 0.003374989141951896966 ),
 .UNSPECIFIED. ) ;
#9889 = PLANE ( 'NONE',  #29166 ) ;
#9890 = DIRECTION ( 'NONE',  ( 0.8531650599175527594, 0.4028455766673922356, -0.3313982828793700652 ) ) ;
#9891 = EDGE_CURVE ( 'NONE', #54772, #25841, #20887, .T. ) ;
#9892 = DIRECTION ( 'NONE',  ( -0.5364919789714478471, 0.6444004775717705469, -0.5449076811759709926 ) ) ;
#9893 = DIRECTION ( 'NONE',  ( 0.5364919789714477361, 0.6444004775717706579, 0.5449076811759711036 ) ) ;
#9894 = CARTESIAN_POINT ( 'NONE',  ( -67.06923785704015017, -9.519576449723603062, 2.681528892132509334 ) ) ;
#9895 = DIRECTION ( 'NONE',  ( -0.005002170337468016433, -0.7660444431189770143, 0.6427681459581293666 ) ) ;
#9896 = EDGE_CURVE ( 'NONE', #3399, #29707, #55531, .T. ) ;
#9897 = EDGE_CURVE ( 'NONE', #27291, #32551, #8132, .T. ) ;
#9898 = ADVANCED_FACE ( 'NONE', ( #11259 ), #3001, .F. ) ;
#9899 = VERTEX_POINT ( 'NONE', #24327 ) ;
#9900 = EDGE_CURVE ( 'NONE', #19288, #13109, #37365, .T. ) ;
#9901 = ORIENTED_EDGE ( 'NONE', *, *, #51993, .F. ) ;
#9902 = ORIENTED_EDGE ( 'NONE', *, *, #17247, .T. ) ;
#9903 = ORIENTED_EDGE ( 'NONE', *, *, #6002, .F. ) ;
#9904 = EDGE_LOOP ( 'NONE', ( #28379, #37694, #41043, #18644 ) ) ;
#9905 = DIRECTION ( 'NONE',  ( 0.6427681459581294776, -0.7660444431189769032, 0.005002170337467562802 ) ) ;
#9906 = DIRECTION ( 'NONE',  ( 0.000000000000000000, -1.000000000000000000, 0.000000000000000000 ) ) ;
#9907 = ORIENTED_EDGE ( 'NONE', *, *, #12117, .F. ) ;
#9908 = ORIENTED_EDGE ( 'NONE', *, *, #54420, .F. ) ;
#9909 = VERTEX_POINT ( 'NONE', #50450 ) ;
#9910 = EDGE_CURVE ( 'NONE', #15470, #12113, #46173, .T. ) ;
#9911 = EDGE_CURVE ( 'NONE', #49710, #3791, #21482, .T. ) ;
#9912 = CARTESIAN_POINT ( 'NONE',  ( -32.65997012216863737, 0.000000000000000000, 9.567562649885804404 ) ) ;
#9913 = ORIENTED_EDGE ( 'NONE', *, *, #14890, .F. ) ;
#9914 = EDGE_CURVE ( 'NONE', #6097, #36758, #434, .T. ) ;
#9915 = FACE_OUTER_BOUND ( 'NONE', #51533, .T. ) ;
#9916 = CARTESIAN_POINT ( 'NONE',  ( -11.27719002838203544, -1.813211359398156919, 4.038164060868105310 ) ) ;
#9917 = VERTEX_POINT ( 'NONE', #26555 ) ;
#9918 = FACE_OUTER_BOUND ( 'NONE', #17020, .T. ) ;
#9919 = VERTEX_POINT ( 'NONE', #56113 ) ;
#9920 = ADVANCED_FACE ( 'NONE', ( #22019 ), #52668, .F. ) ;
#9921 = DIRECTION ( 'NONE',  ( 0.000000000000000000, -0.000000000000000000, -1.000000000000000000 ) ) ;
#9922 = DIRECTION ( 'NONE',  ( -0.7660212471507179544, -0.6427876096865405842, -0.005961354470445141482 ) ) ;
#9923 = EDGE_CURVE ( 'NONE', #41467, #25423, #34803, .T. ) ;
#9924 = LINE ( 'NONE', #14458, #49966 ) ;
#9925 = CARTESIAN_POINT ( 'NONE',  ( -20.26077012639039765, 0.7834091684795615462, 5.482683156939285318 ) ) ;
#9926 = ORIENTED_EDGE ( 'NONE', *, *, #9494, .T. ) ;
#9927 = DIRECTION ( 'NONE',  ( 0.005961354470445682716, -0.6427876096865404731, -0.7660212471507180654 ) ) ;
#9928 = CARTESIAN_POINT ( 'NONE',  ( -19.45180701075420160, 5.143464774974011888, 12.87836550513064537 ) ) ;
#9929 = PLANE ( 'NONE',  #30285 ) ;
#9930 = VERTEX_POINT ( 'NONE', #12670 ) ;
#9931 = CARTESIAN_POINT ( 'NONE',  ( -15.40103151951671734, 0.000000000000000000, 12.95233060667165681 ) ) ;
#9932 = ORIENTED_EDGE ( 'NONE', *, *, #20051, .T. ) ;
#9933 = DIRECTION ( 'NONE',  ( -0.5449076811759708816, 0.6444004775717707689, 0.5364919789714475140 ) ) ;
#9934 = CARTESIAN_POINT ( 'NONE',  ( -10.67476127473329939, 0.000000000000000000, 2.721347302392381096 ) ) ;
#9935 = CARTESIAN_POINT ( 'NONE',  ( -11.61972299033116052, 0.000000000000000000, 4.729979754440159390 ) ) ;
#9936 = CARTESIAN_POINT ( 'NONE',  ( -58.00000000000000711, -9.000000000000000000, -3.457106781186546129 ) ) ;
#9937 = LINE ( 'NONE', #5962, #26873 ) ;
#9938 = PLANE ( 'NONE',  #20420 ) ;
#9939 = DIRECTION ( 'NONE',  ( -0.8531650599175529814, -0.4028455766673920135, 0.3313982828793697877 ) ) ;
#9940 = CARTESIAN_POINT ( 'NONE',  ( -14.46888367232926420, 0.000000000000000000, 12.59025272694991315 ) ) ;
#9941 = DIRECTION ( 'NONE',  ( -0.5449076811759708816, 0.6444004775717707689, 0.5364919789714475140 ) ) ;
#9942 = VERTEX_POINT ( 'NONE', #35367 ) ;
#9943 = CARTESIAN_POINT ( 'NONE',  ( -17.36110980056009723, 3.848249166794009746, 3.302797067581964008 ) ) ;
#9944 = CARTESIAN_POINT ( 'NONE',  ( -9.342070512798265725, 0.000000000000000000, 10.59882438848031505 ) ) ;
#9945 = DIRECTION ( 'NONE',  ( -0.005002170337468016433, -0.7660444431189770143, 0.6427681459581293666 ) ) ;
#9946 = LINE ( 'NONE', #23293, #6943 ) ;
#9947 = DIRECTION ( 'NONE',  ( 0.9321478471874540261, 0.000000000000000000, -0.3620778797217456546 ) ) ;
#9948 = CARTESIAN_POINT ( 'NONE',  ( 4.918891891700036822, -1.130528823225183332, -1.997863978257569118 ) ) ;
#9949 = DIRECTION ( 'NONE',  ( 0.7660212471507180654, -0.6427876096865404731, 0.005961354470445141482 ) ) ;
#9950 = VERTEX_POINT ( 'NONE', #17472 ) ;
#9951 = ORIENTED_EDGE ( 'NONE', *, *, #52811, .F. ) ;
#9952 = CARTESIAN_POINT ( 'NONE',  ( -11.40636015113596180, 0.000000000000000000, 11.32142374880780089 ) ) ;
#9953 = CARTESIAN_POINT ( 'NONE',  ( -26.13493519185646008, 0.000000000000000000, 7.033017491833586377 ) ) ;
#9954 = EDGE_CURVE ( 'NONE', #34831, #43904, #51571, .T. ) ;
#9955 = ORIENTED_EDGE ( 'NONE', *, *, #46752, .F. ) ;
#9956 = CARTESIAN_POINT ( 'NONE',  ( -16.43317633868556626, -0.1191753592594197858, 13.31363028683540151 ) ) ;
#9957 = ORIENTED_EDGE ( 'NONE', *, *, #52141, .T. ) ;
#9958 = DIRECTION ( 'NONE',  ( -0.5449076811759708816, 0.6444004775717707689, 0.5364919789714475140 ) ) ;
#9959 = EDGE_CURVE ( 'NONE', #43441, #16665, #42744, .T. ) ;
#9960 = EDGE_CURVE ( 'NONE', #41657, #36649, #31093, .T. ) ;
#9961 = ORIENTED_EDGE ( 'NONE', *, *, #20430, .T. ) ;
#9962 = ORIENTED_EDGE ( 'NONE', *, *, #33468, .F. ) ;
#9963 = ORIENTED_EDGE ( 'NONE', *, *, #8674, .F. ) ;
#9964 = LINE ( 'NONE', #10540, #7574 ) ;
#9965 = CARTESIAN_POINT ( 'NONE',  ( -58.00000000000000711, -9.000000000000000000, 2.750000000000008438 ) ) ;
#9966 = DIRECTION ( 'NONE',  ( 0.7660212471507180654, -0.6427876096865404731, 0.005961354470445141482 ) ) ;
#9967 = CARTESIAN_POINT ( 'NONE',  ( -11.67244013076689946, 0.000000000000000000, 11.50401908778467863 ) ) ;
#9968 = ORIENTED_EDGE ( 'NONE', *, *, #36360, .F. ) ;
#9969 = ORIENTED_EDGE ( 'NONE', *, *, #23882, .T. ) ;
#9970 = LINE ( 'NONE', #22486, #10977 ) ;
#9971 = ORIENTED_EDGE ( 'NONE', *, *, #15719, .T. ) ;
#9972 = CARTESIAN_POINT ( 'NONE',  ( -9.808144436391993182, 0.000000000000000000, 10.77986332834118777 ) ) ;
#9973 = ORIENTED_EDGE ( 'NONE', *, *, #18610, .F. ) ;
#9974 = CARTESIAN_POINT ( 'NONE',  ( -30.79567442779373110, 0.000000000000000000, 8.843406890442315316 ) ) ;
#9975 = FACE_OUTER_BOUND ( 'NONE', #28546, .T. ) ;
#9976 = ORIENTED_EDGE ( 'NONE', *, *, #37314, .F. ) ;
#9977 = DIRECTION ( 'NONE',  ( -0.8531650599175527594, 0.4028455766673922356, 0.3313982828793700652 ) ) ;
#9978 = VERTEX_POINT ( 'NONE', #52414 ) ;
#9979 = EDGE_CURVE ( 'NONE', #24462, #42825, #26281, .T. ) ;
#9980 = DIRECTION ( 'NONE',  ( -0.5449076811759708816, 0.6444004775717707689, 0.5364919789714475140 ) ) ;
#9982 = EDGE_CURVE ( 'NONE', #16077, #29459, #47586, .T. ) ;
#9981 = ORIENTED_EDGE ( 'NONE', *, *, #27568, .F. ) ;
#9983 = LINE ( 'NONE', #22207, #44900 ) ;
#9984 = CARTESIAN_POINT ( 'NONE',  ( -13.41745442594840654, 3.038739411681508518, 1.796774992419481798 ) ) ;
#9985 = LINE ( 'NONE', #27294, #21960 ) ;
#9986 = VERTEX_POINT ( 'NONE', #43877 ) ;
#9987 = CARTESIAN_POINT ( 'NONE',  ( -12.57067155766631750, 0.000000000000000000, 7.507909797671279861 ) ) ;
#9988 = ADVANCED_FACE ( 'NONE', ( #30572 ), #21174, .F. ) ;
#9989 = CARTESIAN_POINT ( 'NONE',  ( -13.30555201101248208, 4.495856970884009485, 9.428116599730730130 ) ) ;
#9990 = FACE_OUTER_BOUND ( 'NONE', #19813, .T. ) ;
#9991 = CARTESIAN_POINT ( 'NONE',  ( -11.61110082981531377, 0.000000000000000000, 3.622050644666864994 ) ) ;
#9992 = CARTESIAN_POINT ( 'NONE',  ( -12.72567141089270315, 0.000000000000000000, 1.724709365947141748 ) ) ;
#9993 = AXIS2_PLACEMENT_3D ( 'NONE', #37941, #33405, #24872 ) ;
#9994 = CARTESIAN_POINT ( 'NONE',  ( -69.18949689463744335, -11.64195653086973614, 7.657023247222856099 ) ) ;
#9995 = ORIENTED_EDGE ( 'NONE', *, *, #26069, .T. ) ;
#9996 = FACE_OUTER_BOUND ( 'NONE', #4783, .T. ) ;
#9997 = DIRECTION ( 'NONE',  ( 0.007781995580012663651, 0.000000000000000000, -0.9999697198139515519 ) ) ;
#9998 = DIRECTION ( 'NONE',  ( 0.7660212471507180654, -0.6427876096865404731, 0.005961354470445141482 ) ) ;
#9999 = ORIENTED_EDGE ( 'NONE', *, *, #46888, .F. ) ;
#10000 = LINE ( 'NONE', #32441, #6655 ) ;
#10001 = LINE ( 'NONE', #9438, #23638 ) ;
#10002 = ORIENTED_EDGE ( 'NONE', *, *, #28916, .F. ) ;
#10003 = FACE_OUTER_BOUND ( 'NONE', #2081, .T. ) ;
#10004 = CARTESIAN_POINT ( 'NONE',  ( -14.97617745865445826, -5.051250379848161387, 10.78915007593705866 ) ) ;
#10005 = LINE ( 'NONE', #44628, #7845 ) ;
#10006 = CARTESIAN_POINT ( 'NONE',  ( -16.99924723426068951, 0.000000000000000000, 13.49389102713827171 ) ) ;
#10007 = ORIENTED_EDGE ( 'NONE', *, *, #2194, .F. ) ;
#10008 = ORIENTED_EDGE ( 'NONE', *, *, #41910, .T. ) ;
#10009 = CARTESIAN_POINT ( 'NONE',  ( -16.33317936670417225, 0.000000000000000000, 13.31440848639340224 ) ) ;
#10010 = DIRECTION ( 'NONE',  ( -0.5364919789714478471, 0.6444004775717705469, -0.5449076811759709926 ) ) ;
#10011 = CARTESIAN_POINT ( 'NONE',  ( -20.21988856968611969, -2.460819163488157546, 8.574646605433253299 ) ) ;
#10012 = ADVANCED_FACE ( 'NONE', ( #48129 ), #9232, .F. ) ;
#10013 = DIRECTION ( 'NONE',  ( -0.5364919789714478471, 0.6444004775717705469, -0.5449076811759709926 ) ) ;
#10014 = ADVANCED_FACE ( 'NONE', ( #22321 ), #39648, .F. ) ;
#10015 = FACE_OUTER_BOUND ( 'NONE', #954, .T. ) ;
#10016 = ORIENTED_EDGE ( 'NONE', *, *, #48568, .T. ) ;
#10017 = CARTESIAN_POINT ( 'NONE',  ( -18.29747203306047609, -0.1191753592594177458, 14.03778604627889059 ) ) ;
#10018 = VERTEX_POINT ( 'NONE', #18046 ) ;
#10019 = DIRECTION ( 'NONE',  ( 0.007781995580012662783, 0.000000000000000000, -0.9999697198139514409 ) ) ;
#10020 = EDGE_CURVE ( 'NONE', #51066, #32400, #55831, .T. ) ;
#10021 = EDGE_CURVE ( 'NONE', #43180, #28433, #47285, .T. ) ;
#10022 = CARTESIAN_POINT ( 'NONE',  ( 4.848100717410752658, 0.000000000000000000, 2.162384853247617311 ) ) ;
#10023 = ORIENTED_EDGE ( 'NONE', *, *, #16116, .T. ) ;
#10024 = LINE ( 'NONE', #32171, #33801 ) ;
#10025 = DIRECTION ( 'NONE',  ( 0.6427681459581294776, -0.7660444431189769032, 0.005002170337467562802 ) ) ;
#10026 = CARTESIAN_POINT ( 'NONE',  ( -9.542064456761055524, 0.000000000000000000, 10.59726798936431180 ) ) ;
#10027 = ORIENTED_EDGE ( 'NONE', *, *, #26261, .T. ) ;
#10028 = DIRECTION ( 'NONE',  ( -0.005961354470445682716, -0.6427876096865404731, 0.7660212471507180654 ) ) ;
#10029 = VERTEX_POINT ( 'NONE', #4158 ) ;
#10030 = ADVANCED_FACE ( 'NONE', ( #43344 ), #4439, .F. ) ;
#10031 = AXIS2_PLACEMENT_3D ( 'NONE', #34642, #846, #30942 ) ;
#10032 = EDGE_LOOP ( 'NONE', ( #21358, #46355, #49466, #1162 ) ) ;
#10033 = VERTEX_POINT ( 'NONE', #49816 ) ;
#10034 = ORIENTED_EDGE ( 'NONE', *, *, #28599, .T. ) ;
#10035 = CARTESIAN_POINT ( 'NONE',  ( -14.91176584496347424, -5.051250379848164052, 2.512396043748728491 ) ) ;
#10036 = ORIENTED_EDGE ( 'NONE', *, *, #37054, .T. ) ;
#10037 = LINE ( 'NONE', #18262, #1360 ) ;
#10038 = DIRECTION ( 'NONE',  ( 0.005002170337468016433, -0.7660444431189770143, -0.6427681459581293666 ) ) ;
#10039 = EDGE_LOOP ( 'NONE', ( #25666, #11969, #25580, #35457 ) ) ;
#10040 = ORIENTED_EDGE ( 'NONE', *, *, #31629, .T. ) ;
#10041 = CARTESIAN_POINT ( 'NONE',  ( -10.27421835998572064, 0.000000000000000000, 10.96090226820206048 ) ) ;
#10042 = EDGE_LOOP ( 'NONE', ( #48741, #48268, #19912, #55326 ) ) ;
#10043 = PLANE ( 'NONE',  #6538 ) ;
#10044 = DIRECTION ( 'NONE',  ( 0.000000000000000000, 1.000000000000000000, -0.000000000000000000 ) ) ;
#10045 = CARTESIAN_POINT ( 'NONE',  ( -15.50102849149811135, -0.1191753592594197858, 12.95155240711365430 ) ) ;
#10046 = LINE ( 'NONE', #6353, #23900 ) ;
#10047 = CARTESIAN_POINT ( 'NONE',  ( -10.88756908710649896, 0.000000000000000000, 4.366345475602411597 ) ) ;
#10048 = CARTESIAN_POINT ( 'NONE',  ( -12.60458797795435615, 0.000000000000000000, 11.86609696750642229 ) ) ;
#10049 = FACE_OUTER_BOUND ( 'NONE', #26422, .T. ) ;
#10050 = VERTEX_POINT ( 'NONE', #53789 ) ;
#10051 = EDGE_LOOP ( 'NONE', ( #18949, #45120, #10189, #25289 ) ) ;
#10052 = VECTOR ( 'NONE', #18191, 999.9999999999998863 ) ;
#10053 = CARTESIAN_POINT ( 'NONE',  ( -16.81345671998191449, 0.000000000000000000, 3.412238694616132495 ) ) ;
#10054 = EDGE_CURVE ( 'NONE', #23468, #5331, #40483, .T. ) ;
#10055 = CARTESIAN_POINT ( 'NONE',  ( -11.30636317915456779, -0.1191753592594197858, 11.32220194836580340 ) ) ;
#10056 = DIRECTION ( 'NONE',  ( 0.5364919789714477361, 0.6444004775717706579, 0.5449076811759711036 ) ) ;
#10057 = LINE ( 'NONE', #5810, #8638 ) ;
#10058 = EDGE_LOOP ( 'NONE', ( #48399, #39670, #10894, #44445 ) ) ;
#10059 = PLANE ( 'NONE',  #1423 ) ;
#10060 = DIRECTION ( 'NONE',  ( 0.9999697198139515519, 0.000000000000000000, 0.007781995580013368816 ) ) ;
#10061 = ORIENTED_EDGE ( 'NONE', *, *, #40989, .T. ) ;
#10062 = LINE ( 'NONE', #35354, #49243 ) ;
#10063 = CARTESIAN_POINT ( 'NONE',  ( -13.49551489872720111, 0.000000000000000000, 6.931374326914707673 ) ) ;
#10064 = ORIENTED_EDGE ( 'NONE', *, *, #52482, .T. ) ;
#10065 = EDGE_CURVE ( 'NONE', #20837, #18484, #44433, .T. ) ;
#10066 = CARTESIAN_POINT ( 'NONE',  ( -10.39706570871786795, 0.000000000000000000, 1.046174058050539646 ) ) ;
#10067 = LINE ( 'NONE', #27380, #25138 ) ;
#10068 = VECTOR ( 'NONE', #51409, 1000.000000000000227 ) ;
#10069 = CARTESIAN_POINT ( 'NONE',  ( -24.26908309836554878, 0.000000000000000000, 6.108867788427308376 ) ) ;
#10070 = EDGE_CURVE ( 'NONE', #38527, #16305, #32515, .T. ) ;
#10071 = EDGE_CURVE ( 'NONE', #12044, #28099, #49257, .T. ) ;
#10072 = DIRECTION ( 'NONE',  ( -0.5364919789714478471, 0.6444004775717705469, -0.5449076811759709926 ) ) ;
#10073 = VECTOR ( 'NONE', #43122, 1000.000000000000227 ) ;
#10074 = DIRECTION ( 'NONE',  ( 0.5364919789714477361, 0.6444004775717706579, 0.5449076811759711036 ) ) ;
#10075 = VERTEX_POINT ( 'NONE', #19145 ) ;
#10076 = ORIENTED_EDGE ( 'NONE', *, *, #12950, .T. ) ;
#10077 = LINE ( 'NONE', #44711, #31208 ) ;
#10078 = DIRECTION ( 'NONE',  ( 0.7660212471507180654, -0.6427876096865404731, 0.005961354470445141482 ) ) ;
#10079 = CARTESIAN_POINT ( 'NONE',  ( -17.46532115785441519, 0.000000000000000000, 13.67492996699914265 ) ) ;
#10080 = EDGE_CURVE ( 'NONE', #43916, #32205, #1267, .T. ) ;
#10081 = CARTESIAN_POINT ( 'NONE',  ( -12.53905696910820744, 0.000000000000000000, 3.445503061835871517 ) ) ;
#10082 = EDGE_CURVE ( 'NONE', #23668, #56039, #14364, .T. ) ;
#10083 = LINE ( 'NONE', #18904, #1335 ) ;
#10084 = EDGE_LOOP ( 'NONE', ( #29690, #5386, #925, #25716 ) ) ;
#10085 = CARTESIAN_POINT ( 'NONE',  ( -16.11986972353830083, 23.35146472169441267, -3.958709963775913554 ) ) ;
#10086 = CARTESIAN_POINT ( 'NONE',  ( -10.84028925556084388, -0.1191753592594197858, 11.14116300850493246 ) ) ;
#10087 = EDGE_CURVE ( 'NONE', #41032, #36837, #41008, .T. ) ;
#10088 = DIRECTION ( 'NONE',  ( -0.005961354470445682716, -0.6427876096865404731, 0.7660212471507180654 ) ) ;
#10089 = CARTESIAN_POINT ( 'NONE',  ( -16.02599783302199299, 0.000000000000000000, 7.850351719436975628 ) ) ;
#10090 = ORIENTED_EDGE ( 'NONE', *, *, #49388, .T. ) ;
#10091 = CARTESIAN_POINT ( 'NONE',  ( -16.81267852042391198, -0.1191753592594197858, 3.312241722634738039 ) ) ;
#10092 = ORIENTED_EDGE ( 'NONE', *, *, #42107, .T. ) ;
#10093 = CARTESIAN_POINT ( 'NONE',  ( -11.87243407472968926, 0.000000000000000000, 11.50246268866867361 ) ) ;
#10094 = PLANE ( 'NONE',  #18470 ) ;
#10095 = ADVANCED_FACE ( 'NONE', ( #31676 ), #36216, .F. ) ;
#10096 = ORIENTED_EDGE ( 'NONE', *, *, #20539, .F. ) ;
#10097 = VECTOR ( 'NONE', #2241, 999.9999999999998863 ) ;
#10098 = VECTOR ( 'NONE', #47632, 1000.000000000000114 ) ;
#10099 = DIRECTION ( 'NONE',  ( 0.007781995580012663651, 0.000000000000000000, -0.9999697198139515519 ) ) ;
#10100 = ORIENTED_EDGE ( 'NONE', *, *, #33344, .F. ) ;
#10101 = ADVANCED_FACE ( 'NONE', ( #22592 ), #53516, .F. ) ;
#10102 = VERTEX_POINT ( 'NONE', #27391 ) ;
#10103 = ORIENTED_EDGE ( 'NONE', *, *, #44902, .T. ) ;
#10104 = DIRECTION ( 'NONE',  ( 0.9999697198139515519, 0.000000000000000000, 0.007781995580013368816 ) ) ;
#10105 = ORIENTED_EDGE ( 'NONE', *, *, #32844, .T. ) ;
#10106 = EDGE_LOOP ( 'NONE', ( #40506, #9747, #37023, #14379, #39036, #25268, #20038, #29547 ) ) ;
#10107 = DIRECTION ( 'NONE',  ( -0.005961354470445682716, -0.6427876096865404731, 0.7660212471507180654 ) ) ;
#10108 = PLANE ( 'NONE',  #42145 ) ;
#10109 = EDGE_LOOP ( 'NONE', ( #45763, #5365, #26947, #3233 ) ) ;
#10110 = ORIENTED_EDGE ( 'NONE', *, *, #54058, .T. ) ;
#10111 = LINE ( 'NONE', #9567, #43992 ) ;
#10112 = VERTEX_POINT ( 'NONE', #14618 ) ;
#10113 = EDGE_LOOP ( 'NONE', ( #33204, #8994, #23226, #34217, #10623, #49393, #45235 ) ) ;
#10114 = AXIS2_PLACEMENT_3D ( 'NONE', #53069, #53355, #43975 ) ;
#10115 = DIRECTION ( 'NONE',  ( -0.7660212471507179544, -0.6427876096865405842, -0.005961354470445141482 ) ) ;
#10116 = LINE ( 'NONE', #35401, #50263 ) ;
#10117 = FACE_OUTER_BOUND ( 'NONE', #49913, .T. ) ;
#10118 = PLANE ( 'NONE',  #26844 ) ;
#10119 = ORIENTED_EDGE ( 'NONE', *, *, #47743, .F. ) ;
#10120 = CARTESIAN_POINT ( 'NONE',  ( -17.09571308368427367, -2.622721114510659035, 7.626819433174508056 ) ) ;
#10121 = VERTEX_POINT ( 'NONE', #31937 ) ;
#10122 = EDGE_CURVE ( 'NONE', #49177, #1909, #49559, .T. ) ;
#10123 = FACE_OUTER_BOUND ( 'NONE', #22525, .T. ) ;
#10124 = CARTESIAN_POINT ( 'NONE',  ( -9.808144436391993182, 0.000000000000000000, 10.77986332834118777 ) ) ;
#10125 = CARTESIAN_POINT ( 'NONE',  ( -69.14205738506272780, 0.1323226647188939231, -6.443496511055998965 ) ) ;
#10126 = LINE ( 'NONE', #28021, #34904 ) ;
#10127 = LINE ( 'NONE', #23212, #54728 ) ;
#10128 = DIRECTION ( 'NONE',  ( 0.000000000000000000, -0.000000000000000000, -1.000000000000000000 ) ) ;
#10129 = VERTEX_POINT ( 'NONE', #27127 ) ;
#10130 = LINE ( 'NONE', #1325, #35633 ) ;
#10131 = B_SPLINE_SURFACE_WITH_KNOTS ( 'NONE', 1, 3, ( 
 ( #3627, #21792, #47342, #4483, #29775, #33718, #34564, #26326, #186, #42536, #9023, #43387, #43639, #20683 ),
 ( #8178, #8448, #37998, #42794, #38257, #34865, #25776, #38848, #8761, #17243, #25486, #51880, #55581, #29480 ) ),
 .UNSPECIFIED., .F., .F., .F.,
 ( 2, 2 ),
 ( 4, 2, 2, 2, 2, 2, 4 ),
 ( 0.000000000000000000, 1.000000000000000000 ),
 ( 0.000000000000000000, 0.1159099261691615840, 0.2318198523383231680, 0.4636397046766463359, 0.6954595570149695316, 0.9272794093532926718, 1.000000000000000000 ),
 .UNSPECIFIED. ) ;
#10132 = ORIENTED_EDGE ( 'NONE', *, *, #45776, .F. ) ;
#10133 = VECTOR ( 'NONE', #55258, 1000.000000000000227 ) ;
#10134 = VECTOR ( 'NONE', #8440, 1000.000000000000227 ) ;
#10135 = FACE_OUTER_BOUND ( 'NONE', #40623, .T. ) ;
#10136 = LINE ( 'NONE', #31998, #38670 ) ;
#10137 = FACE_OUTER_BOUND ( 'NONE', #43965, .T. ) ;
#10138 = CARTESIAN_POINT ( 'NONE',  ( -14.57916698481732887, 1.095915999411504194, 2.310009840857418340 ) ) ;
#10139 = EDGE_CURVE ( 'NONE', #39340, #27792, #52958, .T. ) ;
#10140 = DIRECTION ( 'NONE',  ( -0.7660212471507179544, -0.6427876096865405842, -0.005961354470445141482 ) ) ;
#10141 = LINE ( 'NONE', #5341, #39318 ) ;
#10142 = VECTOR ( 'NONE', #42657, 1000.000000000000227 ) ;
#10143 = ORIENTED_EDGE ( 'NONE', *, *, #50663, .T. ) ;
#10144 = DIRECTION ( 'NONE',  ( 0.005002170337468016433, -0.7660444431189770143, -0.6427681459581293666 ) ) ;
#10145 = DIRECTION ( 'NONE',  ( 0.6427681459581294776, -0.7660444431189769032, 0.005002170337467562802 ) ) ;
#10146 = DIRECTION ( 'NONE',  ( 0.007781995580012663651, 0.000000000000000000, -0.9999697198139515519 ) ) ;
#10147 = DIRECTION ( 'NONE',  ( -0.005961354470445682716, -0.6427876096865404731, 0.7660212471507180654 ) ) ;
#10148 = EDGE_CURVE ( 'NONE', #30900, #40325, #18305, .T. ) ;
#10149 = VECTOR ( 'NONE', #19249, 999.9999999999998863 ) ;
#10150 = LINE ( 'NONE', #17555, #38463 ) ;
#10151 = DIRECTION ( 'NONE',  ( 0.9999697198139515519, 0.000000000000000000, 0.007781995580013368816 ) ) ;
#10152 = LINE ( 'NONE', #40256, #48294 ) ;
#10153 = VECTOR ( 'NONE', #50035, 1000.000000000000227 ) ;
#10154 = EDGE_CURVE ( 'NONE', #15763, #20246, #45022, .T. ) ;
#10155 = FACE_OUTER_BOUND ( 'NONE', #19533, .T. ) ;
#10156 = CARTESIAN_POINT ( 'NONE',  ( -18.37703690296480019, -5.213152330870661544, 12.37586806173053056 ) ) ;
#10157 = EDGE_CURVE ( 'NONE', #46689, #9630, #40753, .T. ) ;
#10158 = ORIENTED_EDGE ( 'NONE', *, *, #13652, .T. ) ;
#10159 = EDGE_CURVE ( 'NONE', #22163, #41757, #2096, .T. ) ;
#10160 = ORIENTED_EDGE ( 'NONE', *, *, #25159, .F. ) ;
#10161 = ORIENTED_EDGE ( 'NONE', *, *, #48437, .T. ) ;
#10162 = EDGE_LOOP ( 'NONE', ( #27007, #2325, #25182, #40699 ) ) ;
#10163 = EDGE_LOOP ( 'NONE', ( #25777, #34390, #38768, #26916 ) ) ;
#10164 = DIRECTION ( 'NONE',  ( 0.005961354470445682716, -0.6427876096865404731, -0.7660212471507180654 ) ) ;
#10165 = CARTESIAN_POINT ( 'NONE',  ( -11.63984136486813803, 0.000000000000000000, 7.315147677244509872 ) ) ;
#10166 = AXIS2_PLACEMENT_3D ( 'NONE', #38589, #47100, #20966 ) ;
#10167 = VECTOR ( 'NONE', #34365, 999.9999999999998863 ) ;
#10168 = ORIENTED_EDGE ( 'NONE', *, *, #31169, .F. ) ;
#10169 = ORIENTED_EDGE ( 'NONE', *, *, #15766, .F. ) ;
#10170 = ORIENTED_EDGE ( 'NONE', *, *, #14215, .T. ) ;
#10171 = VECTOR ( 'NONE', #35475, 1000.000000000000114 ) ;
#10172 = CARTESIAN_POINT ( 'NONE',  ( -16.93515325216717926, 0.000000000000000000, 5.257951973096605336 ) ) ;
#10173 = CARTESIAN_POINT ( 'NONE',  ( -28.93060053386082231, -0.1191753592594197858, 8.019254159017428663 ) ) ;
#10174 = CARTESIAN_POINT ( 'NONE',  ( -15.52244184149622264, 0.000000000000000000, 2.852947544891258680 ) ) ;
#10175 = ORIENTED_EDGE ( 'NONE', *, *, #12731, .T. ) ;
#10176 = LINE ( 'NONE', #32042, #45514 ) ;
#10177 = EDGE_CURVE ( 'NONE', #26525, #16077, #45284, .T. ) ;
#10178 = ORIENTED_EDGE ( 'NONE', *, *, #1210, .T. ) ;
#10179 = DIRECTION ( 'NONE',  ( 0.7660212471507180654, -0.6427876096865404731, 0.005961354470445141482 ) ) ;
#10180 = VECTOR ( 'NONE', #52093, 1000.000000000000114 ) ;
#10181 = ADVANCED_FACE ( 'NONE', ( #36774 ), #35645, .F. ) ;
#10182 = CARTESIAN_POINT ( 'NONE',  ( -27.06708303904391144, 0.000000000000000000, 7.395095371555332697 ) ) ;
#10183 = CARTESIAN_POINT ( 'NONE',  ( -20.54204810873173415, 0.000000000000000000, 4.860550213503115558 ) ) ;
#10184 = DIRECTION ( 'NONE',  ( 0.6427681459581294776, -0.7660444431189769032, 0.005002170337467562802 ) ) ;
#10185 = CARTESIAN_POINT ( 'NONE',  ( -11.79997668751810203, -2.460819163488159766, 1.386319776390585012 ) ) ;
#10186 = CARTESIAN_POINT ( 'NONE',  ( -25.54041736840764187, 17.91250900301538351, 4.591768117563441720 ) ) ;
#10187 = FACE_OUTER_BOUND ( 'NONE', #654, .T. ) ;
#10188 = EDGE_CURVE ( 'NONE', #19170, #33373, #20826, .T. ) ;
#10189 = ORIENTED_EDGE ( 'NONE', *, *, #23850, .T. ) ;
#10190 = CARTESIAN_POINT ( 'NONE',  ( -9.755427295956252465, 0.000000000000000000, 4.005823994996667636 ) ) ;
#10191 = ORIENTED_EDGE ( 'NONE', *, *, #36713, .F. ) ;
#10192 = EDGE_CURVE ( 'NONE', #13134, #33706, #54610, .T. ) ;
#10193 = ADVANCED_FACE ( 'NONE', ( #6659 ), #16562, .F. ) ;
#10194 = EDGE_CURVE ( 'NONE', #18937, #36080, #10914, .T. ) ;
#10195 = DIRECTION ( 'NONE',  ( 0.005961354470445682716, -0.6427876096865404731, -0.7660212471507180654 ) ) ;
#10196 = LINE ( 'NONE', #27518, #25993 ) ;
#10197 = CARTESIAN_POINT ( 'NONE',  ( -56.02165185617580079, 5.343604887189308705, 2.999999999999993339 ) ) ;
#10198 = CARTESIAN_POINT ( 'NONE',  ( -18.46543118150865226, 2.391131607591508335, 3.778242673840852994 ) ) ;
#10199 = VECTOR ( 'NONE', #10074, 999.9999999999998863 ) ;
#10200 = DIRECTION ( 'NONE',  ( 0.007781995580012663651, -3.146120232559066537E-19, -0.9999697198139514409 ) ) ;
#10201 = DIRECTION ( 'NONE',  ( 0.000000000000000000, -0.000000000000000000, -1.000000000000000000 ) ) ;
#10202 = CARTESIAN_POINT ( 'NONE',  ( 5.204999356530675136, -6.244963811491316186, -2.061810099490657411 ) ) ;
#10203 = FACE_OUTER_BOUND ( 'NONE', #11283, .T. ) ;
#10204 = FACE_OUTER_BOUND ( 'NONE', #25137, .T. ) ;
#10205 = ORIENTED_EDGE ( 'NONE', *, *, #727, .F. ) ;
#10206 = VECTOR ( 'NONE', #26489, 999.9999999999998863 ) ;
#10207 = CARTESIAN_POINT ( 'NONE',  ( -15.83594370396432183, 0.000000000000000000, 9.129152987621246496 ) ) ;
#10208 = DIRECTION ( 'NONE',  ( 0.5364919789714477361, 0.6444004775717706579, 0.5449076811759711036 ) ) ;
#10209 = CARTESIAN_POINT ( 'NONE',  ( -19.60834386242827776, 0.000000000000000000, 4.298478389818581213 ) ) ;
#10210 = DIRECTION ( 'NONE',  ( 0.007781995580012663651, -3.146120232559066537E-19, -0.9999697198139514409 ) ) ;
#10211 = VECTOR ( 'NONE', #33140, 1000.000000000000114 ) ;
#10212 = AXIS2_PLACEMENT_3D ( 'NONE', #50763, #55050, #45962 ) ;
#10213 = CARTESIAN_POINT ( 'NONE',  ( 2.072287782118878319, 0.000000000000000000, -2.950529333540147015 ) ) ;
#10214 = EDGE_CURVE ( 'NONE', #26440, #51840, #55194, .T. ) ;
#10215 = CARTESIAN_POINT ( 'NONE',  ( -22.40634380310664397, 0.000000000000000000, 5.584705972946605534 ) ) ;
#10216 = CARTESIAN_POINT ( 'NONE',  ( -16.37157077545227324, 4.333955019861511992, 2.902929945681169688 ) ) ;
#10217 = ORIENTED_EDGE ( 'NONE', *, *, #33425, .F. ) ;
#10218 = EDGE_CURVE ( 'NONE', #40214, #41786, #33059, .T. ) ;
#10219 = VECTOR ( 'NONE', #39721, 1000.000000000000227 ) ;
#10220 = VECTOR ( 'NONE', #49866, 1000.000000000000227 ) ;
#10221 = EDGE_LOOP ( 'NONE', ( #391, #3333, #29745, #32440 ) ) ;
#10222 = EDGE_CURVE ( 'NONE', #49166, #15338, #19724, .T. ) ;
#10223 = CARTESIAN_POINT ( 'NONE',  ( -18.78542079201265125, -1.327505506330656893, 6.157489818200859943 ) ) ;
#10224 = PLANE ( 'NONE',  #33184 ) ;
#10225 = EDGE_CURVE ( 'NONE', #34831, #9919, #11489, .T. ) ;
#10226 = ORIENTED_EDGE ( 'NONE', *, *, #37599, .F. ) ;
#10227 = FACE_OUTER_BOUND ( 'NONE', #12130, .T. ) ;
#10228 = VECTOR ( 'NONE', #35918, 1000.000000000000227 ) ;
#10229 = ORIENTED_EDGE ( 'NONE', *, *, #27733, .F. ) ;
#10230 = CARTESIAN_POINT ( 'NONE',  ( -17.08519138589328179, 4.010151117816509903, 10.09913083817650303 ) ) ;
#10231 = AXIS2_PLACEMENT_3D ( 'NONE', #16236, #33553, #50864 ) ;
#10232 = EDGE_CURVE ( 'NONE', #12750, #21737, #37049, .T. ) ;
#10233 = VERTEX_POINT ( 'NONE', #50379 ) ;
#10234 = ORIENTED_EDGE ( 'NONE', *, *, #35725, .T. ) ;
#10235 = VERTEX_POINT ( 'NONE', #42130 ) ;
#10236 = DIRECTION ( 'NONE',  ( 1.000000000000000000, 0.000000000000000000, 0.000000000000000000 ) ) ;
#10237 = DIRECTION ( 'NONE',  ( 0.6427681459581294776, -0.7660444431189769032, 0.005002170337467562802 ) ) ;
#10238 = PLANE ( 'NONE',  #10336 ) ;
#10239 = VECTOR ( 'NONE', #21581, 1000.000000000000227 ) ;
#10240 = CARTESIAN_POINT ( 'NONE',  ( -11.60535272280474928, 0.000000000000000000, 2.883431238151338505 ) ) ;
#10241 = ORIENTED_EDGE ( 'NONE', *, *, #30459, .T. ) ;
#10242 = EDGE_LOOP ( 'NONE', ( #48422, #5780, #52861, #24421 ) ) ;
#10243 = VECTOR ( 'NONE', #23299, 1000.000000000000000 ) ;
#10244 = CARTESIAN_POINT ( 'NONE',  ( -16.27128914543113680, 2.553033558614006715, 2.920797873763766095 ) ) ;
#10245 = ORIENTED_EDGE ( 'NONE', *, *, #40525, .T. ) ;
#10246 = AXIS2_PLACEMENT_3D ( 'NONE', #37526, #54845, #33293 ) ;
#10247 = DIRECTION ( 'NONE',  ( 0.7660212471507180654, -0.6427876096865404731, 0.005961354470445141482 ) ) ;
#10248 = ORIENTED_EDGE ( 'NONE', *, *, #306, .T. ) ;
#10249 = FACE_OUTER_BOUND ( 'NONE', #51211, .T. ) ;
#10250 = AXIS2_PLACEMENT_3D ( 'NONE', #28641, #36896, #28338 ) ;
#10251 = AXIS2_PLACEMENT_3D ( 'NONE', #50644, #11736, #37287 ) ;
#10252 = ORIENTED_EDGE ( 'NONE', *, *, #7228, .T. ) ;
#10253 = LINE ( 'NONE', #23039, #26786 ) ;
#10254 = VERTEX_POINT ( 'NONE', #2927 ) ;
#10255 = AXIS2_PLACEMENT_3D ( 'NONE', #16296, #38158, #6972 ) ;
#10256 = PLANE ( 'NONE',  #39975 ) ;
#10257 = VECTOR ( 'NONE', #53443, 1000.000000000000227 ) ;
#10258 = ORIENTED_EDGE ( 'NONE', *, *, #46522, .F. ) ;
#10259 = DIRECTION ( 'NONE',  ( -0.7660212471507179544, -0.6427876096865405842, -0.005961354470445141482 ) ) ;
#10260 = CARTESIAN_POINT ( 'NONE',  ( -19.42933299877883968, -1.003701604285656579, 4.396310540701692915 ) ) ;
#10261 = CARTESIAN_POINT ( 'NONE',  ( -14.42059698451481076, 0.000000000000000000, 6.385517040825948953 ) ) ;
#10262 = ORIENTED_EDGE ( 'NONE', *, *, #42309, .T. ) ;
#10263 = EDGE_CURVE ( 'NONE', #4466, #31521, #55462, .T. ) ;
#10264 = EDGE_CURVE ( 'NONE', #15700, #6398, #24811, .T. ) ;
#10265 = DIRECTION ( 'NONE',  ( -0.3620778797217456546, 0.000000000000000000, -0.9321478471874540261 ) ) ;
#10266 = CARTESIAN_POINT ( 'NONE',  ( -24.27063949748155380, 0.000000000000000000, 6.308861732390097288 ) ) ;
#10267 = FACE_OUTER_BOUND ( 'NONE', #33335, .T. ) ;
#10268 = VECTOR ( 'NONE', #43176, 1000.000000000000227 ) ;
#10269 = FACE_OUTER_BOUND ( 'NONE', #23418, .T. ) ;
#10270 = EDGE_CURVE ( 'NONE', #45526, #27480, #54350, .T. ) ;
#10271 = AXIS2_PLACEMENT_3D ( 'NONE', #49285, #27723, #5563 ) ;
#10272 = LINE ( 'NONE', #5450, #53943 ) ;
#10273 = CARTESIAN_POINT ( 'NONE',  ( -13.85891992762947744, 5.143464774974011888, 10.70589822680017456 ) ) ;
#10274 = CARTESIAN_POINT ( 'NONE',  ( -68.50280060959401851, -9.683984559439076989, -6.182688104189539402 ) ) ;
#10275 = EDGE_LOOP ( 'NONE', ( #30600, #25520, #28100, #56016 ) ) ;
#10276 = FACE_OUTER_BOUND ( 'NONE', #1149, .T. ) ;
#10277 = CARTESIAN_POINT ( 'NONE',  ( -22.40556560354864146, -0.1191753592594197858, 5.484709000965211523 ) ) ;
#10278 = CARTESIAN_POINT ( 'NONE',  ( -66.55406810601930090, 5.346159682976206314E-12, -1.783245832580018675 ) ) ;
#10279 = ORIENTED_EDGE ( 'NONE', *, *, #24220, .T. ) ;
#10280 = DIRECTION ( 'NONE',  ( -0.005002170337468016433, -0.7660444431189770143, 0.6427681459581293666 ) ) ;
#10281 = DIRECTION ( 'NONE',  ( -0.7660212471507179544, -0.6427876096865405842, -0.005961354470445141482 ) ) ;
#10282 = ORIENTED_EDGE ( 'NONE', *, *, #627, .T. ) ;
#10283 = VECTOR ( 'NONE', #7449, 999.9999999999998863 ) ;
#10284 = DIRECTION ( 'NONE',  ( -0.5364919789714478471, 0.6444004775717705469, -0.5449076811759709926 ) ) ;
#10285 = AXIS2_PLACEMENT_3D ( 'NONE', #10295, #18534, #5474 ) ;
#10286 = CARTESIAN_POINT ( 'NONE',  ( -13.27065584551087163, 0.000000000000000000, 12.04557950825129176 ) ) ;
#10287 = DIRECTION ( 'NONE',  ( 0.000000000000000000, -0.000000000000000000, -1.000000000000000000 ) ) ;
#10288 = ORIENTED_EDGE ( 'NONE', *, *, #28680, .T. ) ;
#10289 = EDGE_LOOP ( 'NONE', ( #12962, #25822, #4722, #13527 ) ) ;
#10290 = EDGE_CURVE ( 'NONE', #10918, #20122, #11189, .T. ) ;
#10291 = CARTESIAN_POINT ( 'NONE',  ( -20.54204810873173415, 0.000000000000000000, 4.860550213503115558 ) ) ;
#10292 = VECTOR ( 'NONE', #31420, 999.9999999999998863 ) ;
#10293 = CARTESIAN_POINT ( 'NONE',  ( -66.84075661360076026, 2.000000000000022204, -6.315096454939387094 ) ) ;
#10294 = VECTOR ( 'NONE', #10881, 1000.000000000000000 ) ;
#10295 = CARTESIAN_POINT ( 'NONE',  ( -19.60990026154428278, 0.000000000000000000, 4.498472333781370125 ) ) ;
#10296 = VECTOR ( 'NONE', #32619, 999.9999999999998863 ) ;
#10297 = EDGE_CURVE ( 'NONE', #15470, #38880, #15442, .T. ) ;
#10298 = LINE ( 'NONE', #668, #52754 ) ;
#10299 = VERTEX_POINT ( 'NONE', #46113 ) ;
#10300 = PLANE ( 'NONE',  #55734 ) ;
#10301 = VERTEX_POINT ( 'NONE', #28511 ) ;
#10302 = FACE_OUTER_BOUND ( 'NONE', #51793, .T. ) ;
#10303 = ADVANCED_FACE ( 'NONE', ( #45833 ), #24268, .F. ) ;
#10304 = VECTOR ( 'NONE', #51986, 999.9999999999998863 ) ;
#10305 = PLANE ( 'NONE',  #44179 ) ;
#10306 = AXIS2_PLACEMENT_3D ( 'NONE', #38573, #25242, #51052 ) ;
#10307 = EDGE_LOOP ( 'NONE', ( #8350, #52127, #45577, #32414, #28581 ) ) ;
#10308 = EDGE_CURVE ( 'NONE', #48202, #45033, #46372, .T. ) ;
#10309 = DIRECTION ( 'NONE',  ( -0.005002170337468016433, -0.7660444431189770143, 0.6427681459581293666 ) ) ;
#10310 = DIRECTION ( 'NONE',  ( 0.7660212471507180654, -0.6427876096865404731, 0.005961354470445141482 ) ) ;
#10311 = EDGE_CURVE ( 'NONE', #36044, #38766, #2659, .T. ) ;
#10312 = PLANE ( 'NONE',  #42998 ) ;
#10313 = VERTEX_POINT ( 'NONE', #24519 ) ;
#10314 = DIRECTION ( 'NONE',  ( 1.000000000000000000, 0.000000000000000000, -0.000000000000000000 ) ) ;
#10315 = ADVANCED_FACE ( 'NONE', ( #3236 ), #7793, .F. ) ;
#10316 = ORIENTED_EDGE ( 'NONE', *, *, #23588, .F. ) ;
#10317 = ORIENTED_EDGE ( 'NONE', *, *, #6426, .T. ) ;
#10318 = ORIENTED_EDGE ( 'NONE', *, *, #23176, .T. ) ;
#10319 = DIRECTION ( 'NONE',  ( 0.000000000000000000, -0.000000000000000000, -1.000000000000000000 ) ) ;
#10320 = AXIS2_PLACEMENT_3D ( 'NONE', #30150, #13116, #42639 ) ;
#10321 = ORIENTED_EDGE ( 'NONE', *, *, #2727, .F. ) ;
#10322 = DIRECTION ( 'NONE',  ( 0.5364919789714477361, 0.6444004775717706579, 0.5449076811759711036 ) ) ;
#10323 = VERTEX_POINT ( 'NONE', #17700 ) ;
#10324 = VECTOR ( 'NONE', #24625, 1000.000000000000227 ) ;
#10325 = CARTESIAN_POINT ( 'NONE',  ( -10.23886491294503820, 0.000000000000000000, 6.418060246738034991 ) ) ;
#10326 = CARTESIAN_POINT ( 'NONE',  ( -13.19506564939623416, 0.000000000000000000, 2.332401641178565299 ) ) ;
#10327 = ORIENTED_EDGE ( 'NONE', *, *, #54598, .T. ) ;
#10328 = CARTESIAN_POINT ( 'NONE',  ( -16.53317331066696383, 0.000000000000000000, 13.31285208727739899 ) ) ;
#10329 = VECTOR ( 'NONE', #9593, 1000.000000000000000 ) ;
#10330 = ORIENTED_EDGE ( 'NONE', *, *, #22010, .T. ) ;
#10331 = FACE_OUTER_BOUND ( 'NONE', #43244, .T. ) ;
#10332 = FACE_OUTER_BOUND ( 'NONE', #28400, .T. ) ;
#10333 = DIRECTION ( 'NONE',  ( -1.000000000000000000, 0.000000000000000000, -0.000000000000000000 ) ) ;
#10334 = DIRECTION ( 'NONE',  ( 0.007781995580012662783, 0.000000000000000000, -0.9999697198139514409 ) ) ;
#10335 = CARTESIAN_POINT ( 'NONE',  ( -21.64220182007004212, 20.16314479920728431, 4.391939828907996279 ) ) ;
#10336 = AXIS2_PLACEMENT_3D ( 'NONE', #14503, #32652, #40638 ) ;
#10337 = CARTESIAN_POINT ( 'NONE',  ( -15.87975247367846166, 0.000000000000000000, 2.850166870931599927 ) ) ;
#10338 = PLANE ( 'NONE',  #32000 ) ;
#10339 = EDGE_LOOP ( 'NONE', ( #15890, #34009, #28167, #33381 ) ) ;
#10340 = VECTOR ( 'NONE', #40298, 1000.000000000000227 ) ;
#10341 = EDGE_CURVE ( 'NONE', #5277, #54540, #17403, .T. ) ;
#10342 = VERTEX_POINT ( 'NONE', #21412 ) ;
#10343 = CARTESIAN_POINT ( 'NONE',  ( -13.53673582514181106, 0.000000000000000000, 12.22817484722816772 ) ) ;
#10344 = FACE_OUTER_BOUND ( 'NONE', #1092, .T. ) ;
#10345 = ADVANCED_FACE ( 'NONE', ( #13451 ), #12873, .F. ) ;
#10346 = ADVANCED_FACE ( 'NONE', ( #25378 ), #4080, .F. ) ;
#10347 = PLANE ( 'NONE',  #8895 ) ;
#10348 = VECTOR ( 'NONE', #31008, 1000.000000000000114 ) ;
#10349 = VECTOR ( 'NONE', #19979, 1000.000000000000227 ) ;
#10350 = FACE_OUTER_BOUND ( 'NONE', #36101, .T. ) ;
#10351 = EDGE_LOOP ( 'NONE', ( #51359, #44346, #48086, #36876 ) ) ;
#10352 = DIRECTION ( 'NONE',  ( 0.7660212471507180654, -0.6427876096865404731, 0.005961354470445141482 ) ) ;
#10353 = PLANE ( 'NONE',  #49527 ) ;
#10354 = ORIENTED_EDGE ( 'NONE', *, *, #8572, .T. ) ;
#10355 = CARTESIAN_POINT ( 'NONE',  ( -19.73291444811881945, 0.000000000000000000, 6.513501371556814412 ) ) ;
#10356 = CARTESIAN_POINT ( 'NONE',  ( -26.26580391614848864, 17.49370688441070953, -4.622528711259356271 ) ) ;
#10357 = ORIENTED_EDGE ( 'NONE', *, *, #37145, .F. ) ;
#10358 = CARTESIAN_POINT ( 'NONE',  ( -66.57353123603060396, -8.724002626923901715, 0.6758588499069799749 ) ) ;
#10359 = DIRECTION ( 'NONE',  ( 0.9999697198139515519, 0.000000000000000000, 0.007781995580013368816 ) ) ;
#10360 = DIRECTION ( 'NONE',  ( 0.007781995580012662783, 0.000000000000000000, -0.9999697198139514409 ) ) ;
#10361 = PLANE ( 'NONE',  #14218 ) ;
#10362 = DIRECTION ( 'NONE',  ( -0.7660212471507179544, -0.6427876096865405842, -0.005961354470445141482 ) ) ;
#10363 = VECTOR ( 'NONE', #7120, 1000.000000000000227 ) ;
#10364 = EDGE_LOOP ( 'NONE', ( #684, #13775, #43678, #46694 ) ) ;
#10365 = VECTOR ( 'NONE', #40122, 1000.000000000000227 ) ;
#10366 = ORIENTED_EDGE ( 'NONE', *, *, #52527, .F. ) ;
#10367 = CARTESIAN_POINT ( 'NONE',  ( -11.30636317915456779, -0.1191753592594197858, 11.32220194836580340 ) ) ;
#10368 = CARTESIAN_POINT ( 'NONE',  ( -11.61054990949386401, 2.553033558614006715, 1.110408475155038266 ) ) ;
#10369 = CARTESIAN_POINT ( 'NONE',  ( -18.83816797531202880, 4.495856970884011261, 3.855874544212809507 ) ) ;
#10370 = VECTOR ( 'NONE', #18284, 1000.000000000000227 ) ;
#10371 = LINE ( 'NONE', #31096, #53654 ) ;
#10372 = LINE ( 'NONE', #54092, #35807 ) ;
#10373 = VECTOR ( 'NONE', #54128, 1000.000000000000114 ) ;
#10374 = ORIENTED_EDGE ( 'NONE', *, *, #53231, .T. ) ;
#10375 = DIRECTION ( 'NONE',  ( 0.6427681459581294776, -0.7660444431189769032, 0.005002170337467562802 ) ) ;
#10376 = EDGE_CURVE ( 'NONE', #43104, #4253, #13163, .T. ) ;
#10377 = CARTESIAN_POINT ( 'NONE',  ( -9.808144436391993182, 0.000000000000000000, 10.77986332834118777 ) ) ;
#10378 = DIRECTION ( 'NONE',  ( 0.3313982828793700097, 0.4028455766673916805, 0.8531650599175528704 ) ) ;
#10379 = CARTESIAN_POINT ( 'NONE',  ( -28.92982233430281980, 0.000000000000000000, 7.919257187036034651 ) ) ;
#10380 = VERTEX_POINT ( 'NONE', #39576 ) ;
#10381 = EDGE_CURVE ( 'NONE', #30922, #22808, #52048, .T. ) ;
#10382 = VECTOR ( 'NONE', #39442, 999.9999999999998863 ) ;
#10383 = CARTESIAN_POINT ( 'NONE',  ( -20.14641686010442356, -0.1941918491731554619, 4.700677864147936980 ) ) ;
#10384 = ORIENTED_EDGE ( 'NONE', *, *, #20693, .T. ) ;
#10385 = DIRECTION ( 'NONE',  ( -0.005961354470445682716, -0.6427876096865404731, 0.7660212471507180654 ) ) ;
#10386 = DIRECTION ( 'NONE',  ( -0.005002170337468016433, -0.7660444431189770143, 0.6427681459581293666 ) ) ;
#10387 = VECTOR ( 'NONE', #38556, 999.9999999999998863 ) ;
#10388 = ORIENTED_EDGE ( 'NONE', *, *, #42117, .T. ) ;
#10389 = DIRECTION ( 'NONE',  ( 0.6427681459581294776, -0.7660444431189769032, 0.005002170337467562802 ) ) ;
#10390 = EDGE_CURVE ( 'NONE', #13096, #18181, #30196, .T. ) ;
#10391 = ORIENTED_EDGE ( 'NONE', *, *, #7947, .F. ) ;
#10392 = AXIS2_PLACEMENT_3D ( 'NONE', #34327, #12733, #8475 ) ;
#10393 = ORIENTED_EDGE ( 'NONE', *, *, #10232, .T. ) ;
#10394 = ORIENTED_EDGE ( 'NONE', *, *, #16164, .F. ) ;
#10395 = DIRECTION ( 'NONE',  ( 0.5364919789714477361, 0.6444004775717706579, 0.5449076811759711036 ) ) ;
#10396 = VECTOR ( 'NONE', #33108, 1000.000000000000000 ) ;
#10397 = ORIENTED_EDGE ( 'NONE', *, *, #15013, .T. ) ;
#10398 = EDGE_LOOP ( 'NONE', ( #355, #48414, #9762, #55150 ) ) ;
#10399 = LINE ( 'NONE', #1599, #34752 ) ;
#10400 = LINE ( 'NONE', #27419, #49409 ) ;
#10401 = VERTEX_POINT ( 'NONE', #47515 ) ;
#10402 = EDGE_CURVE ( 'NONE', #22818, #11131, #42679, .T. ) ;
#10403 = VERTEX_POINT ( 'NONE', #25958 ) ;
#10404 = CARTESIAN_POINT ( 'NONE',  ( -21.47341775636118655, -0.1191753592594197858, 5.122631121243466090 ) ) ;
#10405 = VERTEX_POINT ( 'NONE', #66 ) ;
#10406 = EDGE_LOOP ( 'NONE', ( #54460, #41231, #37849, #19319, #2729 ) ) ;
#10407 = EDGE_CURVE ( 'NONE', #21718, #38033, #9167, .T. ) ;
#10408 = VECTOR ( 'NONE', #37743, 1000.000000000000227 ) ;
#10409 = CARTESIAN_POINT ( 'NONE',  ( -12.57445172676405143, -1.165603555308157846, 1.728476342015877076 ) ) ;
#10410 = AXIS2_PLACEMENT_3D ( 'NONE', #24690, #42013, #25834 ) ;
#10411 = CARTESIAN_POINT ( 'NONE',  ( -12.17363884469051527, -0.1191753592594191197, 3.348343802064481789 ) ) ;
#10412 = CARTESIAN_POINT ( 'NONE',  ( -10.41299237536028421, 0.000000000000000000, 3.092716518302152551 ) ) ;
#10413 = LINE ( 'NONE', #27740, #13314 ) ;
#10414 = EDGE_CURVE ( 'NONE', #23836, #42731, #34730, .T. ) ;
#10415 = ORIENTED_EDGE ( 'NONE', *, *, #48040, .F. ) ;
#10416 = CARTESIAN_POINT ( 'NONE',  ( -16.79925329029790149, 0.000000000000000000, 13.49544742625427496 ) ) ;
#10417 = VECTOR ( 'NONE', #51675, 1000.000000000000227 ) ;
#10418 = ORIENTED_EDGE ( 'NONE', *, *, #45294, .F. ) ;
#10419 = EDGE_CURVE ( 'NONE', #46963, #24466, #43286, .T. ) ;
#10420 = DIRECTION ( 'NONE',  ( 0.007781995580012662783, 0.000000000000000000, -0.9999697198139514409 ) ) ;
#10421 = VECTOR ( 'NONE', #3682, 1000.000000000000227 ) ;
#10422 = EDGE_CURVE ( 'NONE', #26242, #23457, #21102, .T. ) ;
#10423 = CARTESIAN_POINT ( 'NONE',  ( -19.17768093937019458, -0.1191753592594166911, 7.725821564637509908 ) ) ;
#10424 = CARTESIAN_POINT ( 'NONE',  ( -17.74482636761139531, -0.1191753592594203132, 3.674319602356484804 ) ) ;
#10425 = LINE ( 'NONE', #33115, #44861 ) ;
#10426 = DIRECTION ( 'NONE',  ( -0.5364919789714478471, 0.6444004775717705469, -0.5449076811759709926 ) ) ;
#10427 = VECTOR ( 'NONE', #39925, 999.9999999999998863 ) ;
#10428 = LINE ( 'NONE', #52717, #24993 ) ;
#10429 = ORIENTED_EDGE ( 'NONE', *, *, #21474, .T. ) ;
#10430 = DIRECTION ( 'NONE',  ( 0.007781995580012662783, 0.000000000000000000, -0.9999697198139514409 ) ) ;
#10431 = ORIENTED_EDGE ( 'NONE', *, *, #6663, .T. ) ;
#10432 = VECTOR ( 'NONE', #46030, 1000.000000000000114 ) ;
#10433 = ADVANCED_FACE ( 'NONE', ( #26483 ), #16870, .F. ) ;
#10434 = LINE ( 'NONE', #14964, #49253 ) ;
#10435 = CARTESIAN_POINT ( 'NONE',  ( -14.46888367232926420, 0.000000000000000000, 12.59025272694991315 ) ) ;
#10436 = ADVANCED_FACE ( 'NONE', ( #51215 ), #51764, .F. ) ;
#10437 = DIRECTION ( 'NONE',  ( 0.005961354470445682716, -0.6427876096865404731, -0.7660212471507180654 ) ) ;
#10438 = DIRECTION ( 'NONE',  ( 0.9999697198139515519, 0.000000000000000000, 0.007781995580013368816 ) ) ;
#10439 = LINE ( 'NONE', #1334, #54977 ) ;
#10440 = EDGE_CURVE ( 'NONE', #51521, #48984, #8069, .T. ) ;
#10441 = VECTOR ( 'NONE', #5835, 999.9999999999998863 ) ;
#10442 = DIRECTION ( 'NONE',  ( -0.7660212471507179544, -0.6427876096865405842, -0.005961354470445141482 ) ) ;
#10443 = AXIS2_PLACEMENT_3D ( 'NONE', #35625, #1802, #40992 ) ;
#10444 = ORIENTED_EDGE ( 'NONE', *, *, #3800, .F. ) ;
#10445 = DIRECTION ( 'NONE',  ( 0.000000000000000000, -1.000000000000000000, 0.000000000000000000 ) ) ;
#10446 = CARTESIAN_POINT ( 'NONE',  ( -17.73140113748535285, 0.000000000000000000, 13.85752530597602039 ) ) ;
#10447 = CARTESIAN_POINT ( 'NONE',  ( -13.22093213094377617, 0.000000000000000000, 5.656188970498445379 ) ) ;
#10448 = LINE ( 'NONE', #48793, #40966 ) ;
#10449 = DIRECTION ( 'NONE',  ( 0.6427681459581294776, -0.7660444431189769032, 0.005002170337467562802 ) ) ;
#10450 = CARTESIAN_POINT ( 'NONE',  ( -15.62927958056622657, 0.1245042932765045296, 3.156596835203342888 ) ) ;
#10451 = FACE_OUTER_BOUND ( 'NONE', #35147, .T. ) ;
#10452 = VECTOR ( 'NONE', #38801, 1000.000000000000227 ) ;
#10453 = CARTESIAN_POINT ( 'NONE',  ( -10.07782610008833757, 0.000000000000000000, 1.048658454501847137 ) ) ;
#10454 = DIRECTION ( 'NONE',  ( 0.9999697198139515519, 0.000000000000000000, 0.007781995580013368816 ) ) ;
#10455 = VECTOR ( 'NONE', #260, 1000.000000000000227 ) ;
#10456 = VERTEX_POINT ( 'NONE', #29669 ) ;
#10457 = ADVANCED_FACE ( 'NONE', ( #38431 ), #34201, .F. ) ;
#10458 = VECTOR ( 'NONE', #29641, 1000.000000000000227 ) ;
#10459 = ORIENTED_EDGE ( 'NONE', *, *, #29882, .F. ) ;
#10460 = EDGE_LOOP ( 'NONE', ( #20475, #13328, #28049 ) ) ;
#10461 = VECTOR ( 'NONE', #51354, 999.9999999999998863 ) ;
#10462 = VECTOR ( 'NONE', #34710, 999.9999999999998863 ) ;
#10463 = ORIENTED_EDGE ( 'NONE', *, *, #9529, .T. ) ;
#10464 = VECTOR ( 'NONE', #19071, 999.9999999999998863 ) ;
#10465 = ORIENTED_EDGE ( 'NONE', *, *, #23803, .F. ) ;
#10466 = LINE ( 'NONE', #28052, #20561 ) ;
#10467 = LINE ( 'NONE', #24073, #43044 ) ;
#10468 = VECTOR ( 'NONE', #50209, 1000.000000000000227 ) ;
#10469 = EDGE_CURVE ( 'NONE', #44458, #50858, #1741, .T. ) ;
#10470 = ORIENTED_EDGE ( 'NONE', *, *, #25977, .T. ) ;
#10471 = VERTEX_POINT ( 'NONE', #40401 ) ;
#10472 = VERTEX_POINT ( 'NONE', #31019 ) ;
#10473 = ADVANCED_FACE ( 'NONE', ( #6319 ), #44940, .F. ) ;
#10474 = EDGE_CURVE ( 'NONE', #27150, #8639, #18832, .T. ) ;
#10475 = VECTOR ( 'NONE', #861, 999.9999999999998863 ) ;
#10476 = VECTOR ( 'NONE', #53702, 999.9999999999998863 ) ;
#10477 = CARTESIAN_POINT ( 'NONE',  ( -66.09197391315379377, -9.273643325778634150, -5.205015551674848417 ) ) ;
#10478 = LINE ( 'NONE', #24084, #3813 ) ;
#10479 = CARTESIAN_POINT ( 'NONE',  ( -15.40103151951671734, 0.000000000000000000, 12.95233060667165681 ) ) ;
#10480 = VERTEX_POINT ( 'NONE', #1195 ) ;
#10481 = LINE ( 'NONE', #27807, #47349 ) ;
#10482 = ORIENTED_EDGE ( 'NONE', *, *, #18001, .F. ) ;
#10483 = FACE_OUTER_BOUND ( 'NONE', #50034, .T. ) ;
#10484 = EDGE_CURVE ( 'NONE', #27583, #47452, #40686, .T. ) ;
#10485 = DIRECTION ( 'NONE',  ( 0.9999697198139515519, 0.000000000000000000, 0.007781995580013368816 ) ) ;
#10486 = ADVANCED_FACE ( 'NONE', ( #44634 ), #27062, .F. ) ;
#10487 = VECTOR ( 'NONE', #18045, 1000.000000000000114 ) ;
#10488 = DIRECTION ( 'NONE',  ( -0.5364919789714478471, 0.6444004775717705469, -0.5449076811759709926 ) ) ;
#10489 = DIRECTION ( 'NONE',  ( 0.9999697198139515519, 0.000000000000000000, 0.007781995580013368816 ) ) ;
#10490 = DIRECTION ( 'NONE',  ( -0.005961354470445682716, -0.6427876096865404731, 0.7660212471507180654 ) ) ;
#10491 = LINE ( 'NONE', #10762, #53747 ) ;
#10493 = VECTOR ( 'NONE', #45573, 999.9999999999998863 ) ;
#10492 = CARTESIAN_POINT ( 'NONE',  ( -10.94028622754223967, 0.000000000000000000, 11.14038480894692995 ) ) ;
#10494 = ORIENTED_EDGE ( 'NONE', *, *, #16262, .T. ) ;
#10495 = PLANE ( 'NONE',  #34644 ) ;
#10496 = VERTEX_POINT ( 'NONE', #31610 ) ;
#10497 = AXIS2_PLACEMENT_3D ( 'NONE', #22913, #27755, #10128 ) ;
#10498 = EDGE_CURVE ( 'NONE', #19093, #21379, #6059, .T. ) ;
#10499 = CARTESIAN_POINT ( 'NONE',  ( -13.27065584551087163, 0.000000000000000000, 12.04557950825129176 ) ) ;
#10500 = DIRECTION ( 'NONE',  ( 0.007781995580012663651, -3.146120232559066537E-19, -0.9999697198139514409 ) ) ;
#10501 = FACE_OUTER_BOUND ( 'NONE', #32533, .T. ) ;
#10502 = FACE_OUTER_BOUND ( 'NONE', #4313, .T. ) ;
#10503 = VECTOR ( 'NONE', #38916, 1000.000000000000114 ) ;
#10504 = CARTESIAN_POINT ( 'NONE',  ( -17.66531893442506629, -2.784623065533161856, 3.654286853175606975 ) ) ;
#10505 = DIRECTION ( 'NONE',  ( 0.000000000000000000, -0.000000000000000000, -1.000000000000000000 ) ) ;
#10506 = LINE ( 'NONE', #42194, #40660 ) ;
#10507 = EDGE_CURVE ( 'NONE', #19751, #2789, #48340, .T. ) ;
#10509 = VECTOR ( 'NONE', #22749, 1000.000000000000000 ) ;
#10508 = LINE ( 'NONE', #36609, #33747 ) ;
#10510 = VECTOR ( 'NONE', #38531, 1000.000000000000000 ) ;
#10511 = DIRECTION ( 'NONE',  ( -0.6427681459581293666, -0.7660444431189770143, -0.005002170337467561935 ) ) ;
#10512 = ORIENTED_EDGE ( 'NONE', *, *, #28360, .T. ) ;
#10513 = DIRECTION ( 'NONE',  ( 0.007781995580012663651, -3.146120232559066537E-19, -0.9999697198139514409 ) ) ;
#10514 = CARTESIAN_POINT ( 'NONE',  ( -28.93137873341882127, 0.000000000000000000, 8.119251130998824451 ) ) ;
#10515 = PLANE ( 'NONE',  #45437 ) ;
#10516 = CARTESIAN_POINT ( 'NONE',  ( 2.072287782118878319, 0.000000000000000000, -2.950529333540147015 ) ) ;
#10517 = VECTOR ( 'NONE', #8508, 1000.000000000000227 ) ;
#10518 = CARTESIAN_POINT ( 'NONE',  ( -12.90429806846666061, -1.003701604285656579, 1.861765382649475553 ) ) ;
#10519 = AXIS2_PLACEMENT_3D ( 'NONE', #17263, #3927, #38580 ) ;
#10520 = DIRECTION ( 'NONE',  ( 0.5449076811759707706, 0.6444004775717708799, -0.5364919789714476250 ) ) ;
#10521 = CARTESIAN_POINT ( 'NONE',  ( -28.93137873341882127, 0.000000000000000000, 8.119251130998824451 ) ) ;
#10522 = CARTESIAN_POINT ( 'NONE',  ( -3.486932065698848504, -6.851436116247921149, -1.863930744634968883 ) ) ;
#10523 = ORIENTED_EDGE ( 'NONE', *, *, #10711, .F. ) ;
#10524 = VECTOR ( 'NONE', #20580, 1000.000000000000227 ) ;
#10525 = AXIS2_PLACEMENT_3D ( 'NONE', #51891, #40808, #49870 ) ;
#10526 = EDGE_LOOP ( 'NONE', ( #44658, #383, #33962, #43554 ) ) ;
#10527 = DIRECTION ( 'NONE',  ( 0.9999697198139515519, 0.000000000000000000, 0.007781995580013368816 ) ) ;
#10528 = CARTESIAN_POINT ( 'NONE',  ( 0.1285714285714296967, 0.000000000000000000, -5.998622290806041590 ) ) ;
#10529 = ORIENTED_EDGE ( 'NONE', *, *, #51808, .F. ) ;
#10530 = CARTESIAN_POINT ( 'NONE',  ( -12.73212453470555872, -2.460819163488159766, 1.748397656112330667 ) ) ;
#10531 = EDGE_CURVE ( 'NONE', #5703, #31643, #14551, .T. ) ;
#10532 = ORIENTED_EDGE ( 'NONE', *, *, #107, .F. ) ;
#10533 = CARTESIAN_POINT ( 'NONE',  ( 5.284365508485809215, -1.088618427183434934, -2.393569053917001810 ) ) ;
#10534 = VECTOR ( 'NONE', #36152, 1000.000000000000000 ) ;
#10535 = ORIENTED_EDGE ( 'NONE', *, *, #42059, .T. ) ;
#10536 = ORIENTED_EDGE ( 'NONE', *, *, #32826, .F. ) ;
#10537 = ADVANCED_FACE ( 'NONE', ( #53714 ), #14834, .F. ) ;
#10538 = ORIENTED_EDGE ( 'NONE', *, *, #25966, .F. ) ;
#10539 = EDGE_CURVE ( 'NONE', #30584, #16783, #32161, .T. ) ;
#10540 = CARTESIAN_POINT ( 'NONE',  ( -20.50469437842130915, -0.007300641194113378224, 4.854714758035273192 ) ) ;
#10541 = CARTESIAN_POINT ( 'NONE',  ( -13.59054196325603137, -0.1191753592594179401, 6.291973692822567799 ) ) ;
#10542 = VECTOR ( 'NONE', #47567, 999.9999999999998863 ) ;
#10543 = LINE ( 'NONE', #19607, #20290 ) ;
#10544 = EDGE_CURVE ( 'NONE', #27553, #49693, #40106, .T. ) ;
#10545 = EDGE_CURVE ( 'NONE', #33893, #19103, #31866, .T. ) ;
#10546 = EDGE_CURVE ( 'NONE', #1529, #37474, #36263, .T. ) ;
#10547 = ORIENTED_EDGE ( 'NONE', *, *, #704, .F. ) ;
#10548 = VECTOR ( 'NONE', #36323, 1000.000000000000000 ) ;
#10549 = EDGE_LOOP ( 'NONE', ( #3802, #6405, #19149, #11272 ) ) ;
#10550 = ADVANCED_FACE ( 'NONE', ( #51637 ), #12482, .F. ) ;
#10551 = VECTOR ( 'NONE', #24639, 999.9999999999998863 ) ;
#10552 = VECTOR ( 'NONE', #48379, 999.9999999999998863 ) ;
#10553 = LINE ( 'NONE', #10244, #996 ) ;
#10554 = VERTEX_POINT ( 'NONE', #46518 ) ;
#10555 = FACE_OUTER_BOUND ( 'NONE', #26206, .T. ) ;
#10556 = ORIENTED_EDGE ( 'NONE', *, *, #35188, .T. ) ;
#10557 = PLANE ( 'NONE',  #42072 ) ;
#10558 = DIRECTION ( 'NONE',  ( 0.007781995580012663651, 0.000000000000000000, -0.9999697198139515519 ) ) ;
#10559 = VECTOR ( 'NONE', #11780, 1000.000000000000000 ) ;
#10560 = VERTEX_POINT ( 'NONE', #42290 ) ;
#10561 = AXIS2_PLACEMENT_3D ( 'NONE', #50182, #20072, #11587 ) ;
#10562 = LINE ( 'NONE', #49144, #34049 ) ;
#10563 = EDGE_CURVE ( 'NONE', #18224, #34747, #30061, .T. ) ;
#10564 = VECTOR ( 'NONE', #23090, 1000.000000000000114 ) ;
#10565 = EDGE_CURVE ( 'NONE', #16295, #47558, #29203, .T. ) ;
#10566 = CARTESIAN_POINT ( 'NONE',  ( -8.704071095609336339, 0.000000000000000000, 6.599330380697081999 ) ) ;
#10567 = AXIS2_PLACEMENT_3D ( 'NONE', #47579, #18040, #30565 ) ;
#10568 = ORIENTED_EDGE ( 'NONE', *, *, #31577, .T. ) ;
#10569 = DIRECTION ( 'NONE',  ( -0.000000000000000000, -0.000000000000000000, -1.000000000000000000 ) ) ;
#10570 = FILL_AREA_STYLE_COLOUR ( '', #28482 ) ;
#10571 = ADVANCED_FACE ( 'NONE', ( #20113 ), #25252, .F. ) ;
#10572 = DIRECTION ( 'NONE',  ( -0.5364919789714478471, 0.6444004775717705469, -0.5449076811759709926 ) ) ;
#10573 = ORIENTED_EDGE ( 'NONE', *, *, #3302, .F. ) ;
#10574 = EDGE_CURVE ( 'NONE', #14055, #44098, #43134, .T. ) ;
#10575 = CARTESIAN_POINT ( 'NONE',  ( -19.69569380384165669, -0.1191753592594177458, 14.58090286586150697 ) ) ;
#10576 = DIRECTION ( 'NONE',  ( -0.005002170337468016433, -0.7660444431189770143, 0.6427681459581293666 ) ) ;
#10577 = DIRECTION ( 'NONE',  ( 0.007781995580012663651, -3.146120232559066537E-19, -0.9999697198139514409 ) ) ;
#10578 = PLANE ( 'NONE',  #19567 ) ;
#10579 = LINE ( 'NONE', #22765, #21322 ) ;
#10580 = CARTESIAN_POINT ( 'NONE',  ( -19.12962290826653700, 0.000000000000000000, 14.40064212555863854 ) ) ;
#10581 = AXIS2_PLACEMENT_3D ( 'NONE', #35796, #18174, #5413 ) ;
#10582 = CARTESIAN_POINT ( 'NONE',  ( -66.92263959938523499, -11.38200647523100528, 3.427396607173184062 ) ) ;
#10583 = ORIENTED_EDGE ( 'NONE', *, *, #12125, .F. ) ;
#10584 = CARTESIAN_POINT ( 'NONE',  ( -24.96676581047183063, 18.24370688441070953, -4.657437592157546824 ) ) ;
#10585 = LINE ( 'NONE', #31852, #50390 ) ;
#10586 = CARTESIAN_POINT ( 'NONE',  ( -67.65221793698312069, 2.688821387764050996E-14, -7.239294561904388026 ) ) ;
#10587 = VERTEX_POINT ( 'NONE', #20963 ) ;
#10588 = DIRECTION ( 'NONE',  ( 0.6427681459581294776, -0.7660444431189769032, 0.005002170337467562802 ) ) ;
#10589 = DIRECTION ( 'NONE',  ( 0.000000000000000000, -1.000000000000000000, 0.000000000000000000 ) ) ;
#10590 = AXIS2_PLACEMENT_3D ( 'NONE', #3989, #21317, #37504 ) ;
#10591 = AXIS2_PLACEMENT_3D ( 'NONE', #47221, #29923, #664 ) ;
#10592 = DIRECTION ( 'NONE',  ( 0.005961354470445682716, -0.6427876096865404731, -0.7660212471507180654 ) ) ;
#10593 = LINE ( 'NONE', #44093, #580 ) ;
#10594 = PLANE ( 'NONE',  #24738 ) ;
#10595 = EDGE_LOOP ( 'NONE', ( #46447, #6066, #33364, #31692 ) ) ;
#10596 = AXIS2_PLACEMENT_3D ( 'NONE', #2991, #3838, #42482 ) ;
#10597 = ORIENTED_EDGE ( 'NONE', *, *, #11495, .T. ) ;
#10598 = LINE ( 'NONE', #32449, #37719 ) ;
#10599 = CARTESIAN_POINT ( 'NONE',  ( -66.30127701227512205, 2.000000000000023093, -5.120420914815960955 ) ) ;
#10600 = DIRECTION ( 'NONE',  ( 0.005002170337468016433, -0.7660444431189770143, -0.6427681459581293666 ) ) ;
#10601 = VECTOR ( 'NONE', #53490, 999.9999999999998863 ) ;
#10602 = ORIENTED_EDGE ( 'NONE', *, *, #42906, .T. ) ;
#10603 = LINE ( 'NONE', #27920, #42154 ) ;
#10604 = ADVANCED_FACE ( 'NONE', ( #16423 ), #50529, .F. ) ;
#10605 = ORIENTED_EDGE ( 'NONE', *, *, #24751, .F. ) ;
#10606 = CARTESIAN_POINT ( 'NONE',  ( -24.27063949748155380, 0.000000000000000000, 6.308861732390097288 ) ) ;
#10607 = AXIS2_PLACEMENT_3D ( 'NONE', #18122, #540, #26360 ) ;
#10608 = VECTOR ( 'NONE', #23000, 999.9999999999998863 ) ;
#10609 = EDGE_CURVE ( 'NONE', #26301, #50967, #51065, .T. ) ;
#10610 = ORIENTED_EDGE ( 'NONE', *, *, #19588, .F. ) ;
#10611 = DIRECTION ( 'NONE',  ( 0.7660212471507180654, -0.6427876096865404731, 0.005961354470445141482 ) ) ;
#10612 = CARTESIAN_POINT ( 'NONE',  ( -10.94028622754223967, 0.000000000000000000, 11.14038480894692995 ) ) ;
#10613 = FACE_OUTER_BOUND ( 'NONE', #10364, .T. ) ;
#10614 = ADVANCED_FACE ( 'NONE', ( #17015 ), #55074, .F. ) ;
#10615 = EDGE_CURVE ( 'NONE', #44163, #27792, #37448, .T. ) ;
#10616 = ADVANCED_FACE ( 'NONE', ( #25807 ), #38285, .F. ) ;
#10617 = ORIENTED_EDGE ( 'NONE', *, *, #52180, .T. ) ;
#10618 = DIRECTION ( 'NONE',  ( -0.005002170337468016433, -0.7660444431189770143, 0.6427681459581293666 ) ) ;
#10619 = ORIENTED_EDGE ( 'NONE', *, *, #48503, .F. ) ;
#10620 = EDGE_CURVE ( 'NONE', #8057, #17431, #55612, .T. ) ;
#10621 = VECTOR ( 'NONE', #29562, 1000.000000000000114 ) ;
#10622 = ORIENTED_EDGE ( 'NONE', *, *, #4348, .F. ) ;
#10623 = ORIENTED_EDGE ( 'NONE', *, *, #1008, .T. ) ;
#10624 = DIRECTION ( 'NONE',  ( -0.5449076811759708816, 0.6444004775717707689, 0.5364919789714475140 ) ) ;
#10625 = ORIENTED_EDGE ( 'NONE', *, *, #42333, .T. ) ;
#10626 = FACE_OUTER_BOUND ( 'NONE', #36386, .T. ) ;
#10627 = ORIENTED_EDGE ( 'NONE', *, *, #38292, .T. ) ;
#10628 = CARTESIAN_POINT ( 'NONE',  ( -17.86730109935463418, 0.000000000000000000, 5.620029852818350768 ) ) ;
#10629 = CARTESIAN_POINT ( 'NONE',  ( -20.54204810873173415, 0.000000000000000000, 4.860550213503115558 ) ) ;
#10630 = ORIENTED_EDGE ( 'NONE', *, *, #43632, .T. ) ;
#10631 = AXIS2_PLACEMENT_3D ( 'NONE', #53281, #14372, #41585 ) ;
#10632 = DIRECTION ( 'NONE',  ( 0.5449076811759707706, 0.6444004775717708799, -0.5364919789714476250 ) ) ;
#10633 = ORIENTED_EDGE ( 'NONE', *, *, #57, .T. ) ;
#10634 = EDGE_CURVE ( 'NONE', #9106, #8391, #34334, .T. ) ;
#10635 = VECTOR ( 'NONE', #47575, 1000.000000000000227 ) ;
#10636 = DIRECTION ( 'NONE',  ( 0.7660212471507180654, -0.6427876096865404731, 0.005961354470445141482 ) ) ;
#10637 = DIRECTION ( 'NONE',  ( 0.6246952433987894571, -0.7422098413412800966, -0.2426528472758541777 ) ) ;
#10638 = LINE ( 'NONE', #19693, #37738 ) ;
#10639 = CARTESIAN_POINT ( 'NONE',  ( -21.47263955680318404, 0.000000000000000000, 5.022634149262071190 ) ) ;
#10640 = EDGE_CURVE ( 'NONE', #28121, #29147, #41982, .T. ) ;
#10641 = DIRECTION ( 'NONE',  ( -0.7660212471507179544, -0.6427876096865405842, -0.005961354470445141482 ) ) ;
#10642 = CARTESIAN_POINT ( 'NONE',  ( -10.88182098009593446, 0.000000000000000000, 3.627726069086881111 ) ) ;
#10643 = CARTESIAN_POINT ( 'NONE',  ( -16.84795344307834597, -1.813211359398159583, 3.367787457811957541 ) ) ;
#10644 = EDGE_LOOP ( 'NONE', ( #54429, #10007, #37902, #51704 ) ) ;
#10646 = ORIENTED_EDGE ( 'NONE', *, *, #5863, .T. ) ;
#10645 = ADVANCED_FACE ( 'NONE', ( #55328 ), #3084, .F. ) ;
#10647 = VECTOR ( 'NONE', #49908, 999.9999999999998863 ) ;
#10648 = LINE ( 'NONE', #10053, #45469 ) ;
#10649 = LINE ( 'NONE', #40151, #22156 ) ;
#10650 = LINE ( 'NONE', #23664, #52079 ) ;
#10651 = EDGE_CURVE ( 'NONE', #8988, #27291, #47096, .T. ) ;
#10652 = LINE ( 'NONE', #41816, #44197 ) ;
#10653 = VECTOR ( 'NONE', #42681, 1000.000000000000000 ) ;
#10654 = CARTESIAN_POINT ( 'NONE',  ( -15.50102849149811135, -0.1191753592594197858, 12.95155240711365430 ) ) ;
#10655 = EDGE_LOOP ( 'NONE', ( #46778, #11000, #25695, #4435 ) ) ;
#10656 = DIRECTION ( 'NONE',  ( -0.6427681459581293666, -0.7660444431189770143, -0.005002170337467561935 ) ) ;
#10657 = FACE_OUTER_BOUND ( 'NONE', #27131, .T. ) ;
#10658 = ORIENTED_EDGE ( 'NONE', *, *, #10725, .F. ) ;
#10659 = CARTESIAN_POINT ( 'NONE',  ( -32.65997012216863737, 0.000000000000000000, 9.567562649885804404 ) ) ;
#10660 = CARTESIAN_POINT ( 'NONE',  ( -18.39746900504187010, 0.000000000000000000, 14.03700784672088808 ) ) ;
#10661 = ORIENTED_EDGE ( 'NONE', *, *, #37111, .F. ) ;
#10662 = DIRECTION ( 'NONE',  ( 0.000000000000000000, -1.000000000000000000, 0.000000000000000000 ) ) ;
#10663 = DIRECTION ( 'NONE',  ( 0.9999697198139515519, 0.000000000000000000, 0.007781995580013368816 ) ) ;
#10664 = PLANE ( 'NONE',  #17765 ) ;
#10665 = CARTESIAN_POINT ( 'NONE',  ( -17.56503730440392985, -1.003701604285657911, 3.672154781258202050 ) ) ;
#10666 = LINE ( 'NONE', #37295, #7477 ) ;
#10667 = ORIENTED_EDGE ( 'NONE', *, *, #27734, .T. ) ;
#10668 = ORIENTED_EDGE ( 'NONE', *, *, #44636, .F. ) ;
#10669 = DIRECTION ( 'NONE',  ( 0.005961354470445682716, -0.6427876096865404731, -0.7660212471507180654 ) ) ;
#10670 = DIRECTION ( 'NONE',  ( 0.7660212471507180654, -0.6427876096865404731, 0.005961354470445141482 ) ) ;
#10671 = DIRECTION ( 'NONE',  ( 0.007781995580012662783, 0.000000000000000000, -0.9999697198139514409 ) ) ;
#10672 = CARTESIAN_POINT ( 'NONE',  ( 5.558065546916891364, 8.867787166497208620E-06, 2.260478567416572826 ) ) ;
#10673 = CARTESIAN_POINT ( 'NONE',  ( -14.16876790004692843, 0.000000000000000000, 8.034131125803988027 ) ) ;
#10674 = ORIENTED_EDGE ( 'NONE', *, *, #14688, .T. ) ;
#10675 = CARTESIAN_POINT ( 'NONE',  ( -16.95946333459872335, 0.000000000000000000, 8.381745358453697392 ) ) ;
#10677 = VECTOR ( 'NONE', #27695, 999.9999999999998863 ) ;
#10676 = CARTESIAN_POINT ( 'NONE',  ( -11.67244013076689946, 0.000000000000000000, 11.50401908778467863 ) ) ;
#10678 = CARTESIAN_POINT ( 'NONE',  ( -18.14344026625406414, 0.000000000000000000, 7.095209153197401086 ) ) ;
#10679 = ORIENTED_EDGE ( 'NONE', *, *, #21719, .F. ) ;
#10680 = DIRECTION ( 'NONE',  ( 0.000000000000000000, -1.000000000000000000, 0.000000000000000000 ) ) ;
#10681 = ORIENTED_EDGE ( 'NONE', *, *, #38628, .F. ) ;
#10682 = PLANE ( 'NONE',  #25920 ) ;
#10683 = LINE ( 'NONE', #19993, #22088 ) ;
#10684 = ADVANCED_FACE ( 'NONE', ( #50787 ), #42824, .F. ) ;
#10685 = ORIENTED_EDGE ( 'NONE', *, *, #41044, .F. ) ;
#10686 = VECTOR ( 'NONE', #19124, 1000.000000000000114 ) ;
#10687 = CARTESIAN_POINT ( 'NONE',  ( -13.53673582514181106, 0.000000000000000000, 12.22817484722816772 ) ) ;
#10688 = VERTEX_POINT ( 'NONE', #35729 ) ;
#10689 = ADVANCED_FACE ( 'NONE', ( #5355 ), #39972, .F. ) ;
#10690 = EDGE_CURVE ( 'NONE', #54495, #10471, #9620, .T. ) ;
#10691 = ORIENTED_EDGE ( 'NONE', *, *, #5500, .F. ) ;
#10692 = ORIENTED_EDGE ( 'NONE', *, *, #11758, .T. ) ;
#10693 = DIRECTION ( 'NONE',  ( -0.005002170337468016433, -0.7660444431189770143, 0.6427681459581293666 ) ) ;
#10694 = VERTEX_POINT ( 'NONE', #5076 ) ;
#10695 = ORIENTED_EDGE ( 'NONE', *, *, #32286, .F. ) ;
#10696 = CARTESIAN_POINT ( 'NONE',  ( -19.33759994122731385, 21.49370731433205250, -4.239680377485293583 ) ) ;
#10697 = ORIENTED_EDGE ( 'NONE', *, *, #28059, .T. ) ;
#10698 = ORIENTED_EDGE ( 'NONE', *, *, #2086, .T. ) ;
#10699 = DIRECTION ( 'NONE',  ( -0.9999697198139514409, -0.000000000000000000, -0.007781995580013368816 ) ) ;
#10700 = VERTEX_POINT ( 'NONE', #1057 ) ;
#10701 = ORIENTED_EDGE ( 'NONE', *, *, #37827, .T. ) ;
#10702 = CARTESIAN_POINT ( 'NONE',  ( -19.13459676410571220, -3.917936722690661178, 10.54446056703513790 ) ) ;
#10703 = DIRECTION ( 'NONE',  ( 0.000000000000000000, -0.000000000000000000, -1.000000000000000000 ) ) ;
#10704 = CARTESIAN_POINT ( 'NONE',  ( -17.83139810946674686, -0.1191753592594197858, 13.85674710641801788 ) ) ;
#10705 = CARTESIAN_POINT ( 'NONE',  ( -14.69949350034596414, -4.727446477803161073, 10.15025926240234178 ) ) ;
#10706 = EDGE_LOOP ( 'NONE', ( #45349, #39990, #19819, #15141 ) ) ;
#10707 = DIRECTION ( 'NONE',  ( 0.007781995580012662783, 0.000000000000000000, -0.9999697198139514409 ) ) ;
#10708 = VERTEX_POINT ( 'NONE', #18385 ) ;
#10709 = VERTEX_POINT ( 'NONE', #14161 ) ;
#10710 = FACE_OUTER_BOUND ( 'NONE', #19892, .T. ) ;
#10711 = EDGE_CURVE ( 'NONE', #36870, #26056, #22101, .T. ) ;
#10712 = DIRECTION ( 'NONE',  ( 0.000000000000000000, -0.000000000000000000, -1.000000000000000000 ) ) ;
#10713 = CARTESIAN_POINT ( 'NONE',  ( -23.33771345073609638, -0.1191753592594197858, 5.846786880686956955 ) ) ;
#10714 = EDGE_CURVE ( 'NONE', #27821, #10380, #32812, .T. ) ;
#10715 = CARTESIAN_POINT ( 'NONE',  ( -14.93495759592298988, 0.000000000000000000, 12.77129166681078409 ) ) ;
#10716 = DIRECTION ( 'NONE',  ( 0.007781995580012662783, 0.000000000000000000, -0.9999697198139514409 ) ) ;
#10717 = ORIENTED_EDGE ( 'NONE', *, *, #49818, .F. ) ;
#10718 = DIRECTION ( 'NONE',  ( 0.2426528472758541499, 0.7422098413412800966, 0.6246952433987894571 ) ) ;
#10719 = EDGE_CURVE ( 'NONE', #50938, #47436, #56185, .T. ) ;
#10720 = ORIENTED_EDGE ( 'NONE', *, *, #7365, .T. ) ;
#10721 = VECTOR ( 'NONE', #44077, 1000.000000000000114 ) ;
#10722 = CARTESIAN_POINT ( 'NONE',  ( -24.26986129792355129, -0.1191753592594197858, 6.208864760408702388 ) ) ;
#10723 = CARTESIAN_POINT ( 'NONE',  ( -24.83619454210204580, 18.20872041849631984, -4.561852789702152577 ) ) ;
#10724 = FACE_OUTER_BOUND ( 'NONE', #20728, .T. ) ;
#10725 = EDGE_CURVE ( 'NONE', #6678, #50665, #34590, .T. ) ;
#10726 = LINE ( 'NONE', #2709, #46733 ) ;
#10727 = CARTESIAN_POINT ( 'NONE',  ( -17.87592325987048270, 0.000000000000000000, 6.727958962591642944 ) ) ;
#10728 = ORIENTED_EDGE ( 'NONE', *, *, #35662, .F. ) ;
#10729 = DIRECTION ( 'NONE',  ( 0.5449076811759707706, 0.6444004775717708799, -0.5364919789714476250 ) ) ;
#10730 = LINE ( 'NONE', #1885, #51209 ) ;
#10731 = PLANE ( 'NONE',  #17312 ) ;
#10732 = DIRECTION ( 'NONE',  ( 0.6427681459581294776, -0.7660444431189769032, 0.005002170337467562802 ) ) ;
#10733 = CARTESIAN_POINT ( 'NONE',  ( -15.30154763612674707, 0.2864062442990046309, 3.295003302109830390 ) ) ;
#10734 = CARTESIAN_POINT ( 'NONE',  ( -22.40634380310664397, 0.000000000000000000, 5.584705972946605534 ) ) ;
#10735 = DIRECTION ( 'NONE',  ( -0.5449076811759708816, 0.6444004775717707689, 0.5364919789714475140 ) ) ;
#10736 = FACE_OUTER_BOUND ( 'NONE', #5489, .T. ) ;
#10737 = LINE ( 'NONE', #23504, #13818 ) ;
#10738 = EDGE_CURVE ( 'NONE', #28378, #18922, #22405, .T. ) ;
#10739 = ORIENTED_EDGE ( 'NONE', *, *, #21587, .F. ) ;
#10740 = ADVANCED_FACE ( 'NONE', ( #523 ), #39720, .F. ) ;
#10741 = ORIENTED_EDGE ( 'NONE', *, *, #23995, .T. ) ;
#10742 = ORIENTED_EDGE ( 'NONE', *, *, #55208, .F. ) ;
#10743 = ORIENTED_EDGE ( 'NONE', *, *, #2266, .F. ) ;
#10744 = ORIENTED_EDGE ( 'NONE', *, *, #36294, .F. ) ;
#10745 = DIRECTION ( 'NONE',  ( 0.007781995580012662783, 0.000000000000000000, -0.9999697198139514409 ) ) ;
#10746 = LINE ( 'NONE', #20657, #39404 ) ;
#10747 = AXIS2_PLACEMENT_3D ( 'NONE', #9669, #35775, #30399 ) ;
#10748 = EDGE_LOOP ( 'NONE', ( #48249, #47888, #31824, #23431 ) ) ;
#10749 = CARTESIAN_POINT ( 'NONE',  ( -16.96964189423057334, 0.000000000000000000, 9.689668412189776703 ) ) ;
#10750 = ORIENTED_EDGE ( 'NONE', *, *, #41456, .F. ) ;
#10751 = EDGE_CURVE ( 'NONE', #21963, #49166, #35436, .T. ) ;
#10752 = CARTESIAN_POINT ( 'NONE',  ( -68.64979563745795588, -9.566959495664058011, -7.934121704141916531 ) ) ;
#10753 = FACE_OUTER_BOUND ( 'NONE', #34600, .T. ) ;
#10754 = LINE ( 'NONE', #24616, #19579 ) ;
#10755 = ORIENTED_EDGE ( 'NONE', *, *, #19561, .F. ) ;
#10756 = DIRECTION ( 'NONE',  ( 0.007781995580012662783, 0.000000000000000000, -0.9999697198139514409 ) ) ;
#10757 = DIRECTION ( 'NONE',  ( 0.6427681459581294776, -0.7660444431189769032, 0.005002170337467562802 ) ) ;
#10758 = LINE ( 'NONE', #22685, #29369 ) ;
#10759 = CARTESIAN_POINT ( 'NONE',  ( -25.20278734466900517, 0.000000000000000000, 6.670939612111840944 ) ) ;
#10760 = LINE ( 'NONE', #54444, #9703 ) ;
#10761 = LINE ( 'NONE', #23531, #41295 ) ;
#10762 = CARTESIAN_POINT ( 'NONE',  ( -9.342070512798265725, 0.000000000000000000, 10.59882438848031505 ) ) ;
#10763 = CARTESIAN_POINT ( 'NONE',  ( -20.16176772743538237, -0.1191753592594197858, 14.76194180572237968 ) ) ;
#10764 = LINE ( 'NONE', #36593, #14794 ) ;
#10765 = VERTEX_POINT ( 'NONE', #43407 ) ;
#10766 = DIRECTION ( 'NONE',  ( -0.6427681459581293666, -0.7660444431189770143, -0.005002170337467561935 ) ) ;
#10767 = ORIENTED_EDGE ( 'NONE', *, *, #24998, .F. ) ;
#10768 = CARTESIAN_POINT ( 'NONE',  ( -11.75290974440948766, -0.1191753592594203132, 7.783602850887407776 ) ) ;
#10769 = DIRECTION ( 'NONE',  ( 0.7660212471507180654, -0.6427876096865404731, 0.005961354470445141482 ) ) ;
#10770 = LINE ( 'NONE', #15031, #19515 ) ;
#10771 = CARTESIAN_POINT ( 'NONE',  ( -57.29829478218162109, -10.27834239552269935, 3.000000000000005773 ) ) ;
#10772 = ADVANCED_FACE ( 'NONE', ( #21815 ), #34891, .F. ) ;
#10773 = LINE ( 'NONE', #32617, #32313 ) ;
#10774 = LINE ( 'NONE', #40860, #54872 ) ;
#10775 = PLANE ( 'NONE',  #55158 ) ;
#10776 = DIRECTION ( 'NONE',  ( -0.6427681459581293666, -0.7660444431189770143, -0.005002170337467561935 ) ) ;
#10777 = CARTESIAN_POINT ( 'NONE',  ( -15.40103151951671734, 0.000000000000000000, 12.95233060667165681 ) ) ;
#10778 = CARTESIAN_POINT ( 'NONE',  ( -15.33914129824368011, 2.553033558614008047, 2.558719994042019774 ) ) ;
#10779 = DIRECTION ( 'NONE',  ( 0.005961354470445682716, -0.6427876096865404731, -0.7660212471507180654 ) ) ;
#10780 = FACE_OUTER_BOUND ( 'NONE', #40651, .T. ) ;
#10781 = DIRECTION ( 'NONE',  ( 0.005002170337468016433, -0.7660444431189770143, -0.6427681459581293666 ) ) ;
#10782 = EDGE_CURVE ( 'NONE', #9219, #27886, #4774, .T. ) ;
#10783 = VECTOR ( 'NONE', #42954, 999.9999999999998863 ) ;
#10784 = CARTESIAN_POINT ( 'NONE',  ( -9.808144436391993182, 0.000000000000000000, 10.77986332834118777 ) ) ;
#10785 = DIRECTION ( 'NONE',  ( 0.7660212471507180654, -0.6427876096865404731, 0.005961354470445141482 ) ) ;
#10786 = ADVANCED_FACE ( 'NONE', ( #10736 ), #24058, .F. ) ;
#10787 = DIRECTION ( 'NONE',  ( 0.005961354470445682716, -0.6427876096865404731, -0.7660212471507180654 ) ) ;
#10788 = ADVANCED_FACE ( 'NONE', ( #15264 ), #44504, .T. ) ;
#10789 = CARTESIAN_POINT ( 'NONE',  ( -17.93139508144814442, 0.000000000000000000, 13.85596890686001537 ) ) ;
#10790 = ORIENTED_EDGE ( 'NONE', *, *, #12821, .F. ) ;
#10791 = ORIENTED_EDGE ( 'NONE', *, *, #32138, .F. ) ;
#10792 = CARTESIAN_POINT ( 'NONE',  ( -25.20278734466900517, 0.000000000000000000, 6.670939612111840944 ) ) ;
#10793 = LINE ( 'NONE', #2537, #30352 ) ;
#10794 = EDGE_CURVE ( 'NONE', #18005, #294, #53586, .T. ) ;
#10795 = ORIENTED_EDGE ( 'NONE', *, *, #15438, .T. ) ;
#10796 = EDGE_CURVE ( 'NONE', #32426, #21097, #19794, .T. ) ;
#10797 = DIRECTION ( 'NONE',  ( 0.000000000000000000, -0.000000000000000000, -1.000000000000000000 ) ) ;
#10798 = ORIENTED_EDGE ( 'NONE', *, *, #40390, .T. ) ;
#10799 = CARTESIAN_POINT ( 'NONE',  ( -10.31796531083145219, -0.1191753592594183703, 3.732117152394283099 ) ) ;
#10800 = EDGE_CURVE ( 'NONE', #21762, #39658, #11267, .T. ) ;
#10801 = ORIENTED_EDGE ( 'NONE', *, *, #5289, .T. ) ;
#10802 = ORIENTED_EDGE ( 'NONE', *, *, #50254, .T. ) ;
#10803 = ORIENTED_EDGE ( 'NONE', *, *, #25121, .F. ) ;
#10804 = CARTESIAN_POINT ( 'NONE',  ( -9.727461976784988806, 9.474806996477934007, 6.996850153446332321 ) ) ;
#10805 = DIRECTION ( 'NONE',  ( -0.9999697198139514409, -0.000000000000000000, -0.007781995580013368816 ) ) ;
#10806 = DIRECTION ( 'NONE',  ( 0.007781995580012663651, -3.146120232559066537E-19, -0.9999697198139514409 ) ) ;
#10807 = EDGE_CURVE ( 'NONE', #21652, #12842, #6202, .T. ) ;
#10808 = VERTEX_POINT ( 'NONE', #14435 ) ;
#10809 = ORIENTED_EDGE ( 'NONE', *, *, #53891, .F. ) ;
#10810 = EDGE_CURVE ( 'NONE', #6267, #11826, #36554, .T. ) ;
#10811 = DIRECTION ( 'NONE',  ( 0.6427681459581294776, -0.7660444431189769032, 0.005002170337467562802 ) ) ;
#10812 = VERTEX_POINT ( 'NONE', #5614 ) ;
#10813 = LINE ( 'NONE', #49961, #1940 ) ;
#10814 = ORIENTED_EDGE ( 'NONE', *, *, #1025, .T. ) ;
#10815 = DIRECTION ( 'NONE',  ( 0.000000000000000000, -0.000000000000000000, -1.000000000000000000 ) ) ;
#10816 = CARTESIAN_POINT ( 'NONE',  ( -16.81190032086591302, 0.000000000000000000, 3.212244750653343583 ) ) ;
#10817 = STYLED_ITEM ( 'NONE', ( #21608 ), #3559 ) ;
#10818 = EDGE_LOOP ( 'NONE', ( #39077, #11458, #47894, #28886 ) ) ;
#10819 = DIRECTION ( 'NONE',  ( 0.007781995580012663651, 0.000000000000000000, -0.9999697198139515519 ) ) ;
#10820 = DIRECTION ( 'NONE',  ( 0.007781995580012662783, 0.000000000000000000, -0.9999697198139514409 ) ) ;
#10821 = ORIENTED_EDGE ( 'NONE', *, *, #52566, .F. ) ;
#10822 = CARTESIAN_POINT ( 'NONE',  ( -15.42508763604229927, 2.067327705546507133, 6.265785956968178638 ) ) ;
#10823 = DIRECTION ( 'NONE',  ( 0.005002170337468016433, -0.7660444431189770143, -0.6427681459581293666 ) ) ;
#10824 = DIRECTION ( 'NONE',  ( 0.5364919789714477361, 0.6444004775717706579, 0.5449076811759711036 ) ) ;
#10825 = VERTEX_POINT ( 'NONE', #10453 ) ;
#10826 = LINE ( 'NONE', #24174, #5630 ) ;
#10827 = LINE ( 'NONE', #28136, #54096 ) ;
#10828 = FACE_OUTER_BOUND ( 'NONE', #13693, .T. ) ;
#10829 = EDGE_CURVE ( 'NONE', #54076, #45033, #21954, .T. ) ;
#10830 = DIRECTION ( 'NONE',  ( 0.6427681459581294776, -0.7660444431189769032, 0.005002170337467562802 ) ) ;
#10831 = LINE ( 'NONE', #2300, #12234 ) ;
#10832 = DIRECTION ( 'NONE',  ( 0.5364919789714477361, 0.6444004775717706579, 0.5449076811759711036 ) ) ;
#10833 = CARTESIAN_POINT ( 'NONE',  ( -67.69827580336652773, -11.47095193942022995, 5.359670781636989290 ) ) ;
#10834 = EDGE_LOOP ( 'NONE', ( #20203, #28537, #4936, #45988 ) ) ;
#10835 = DIRECTION ( 'NONE',  ( -0.9999697198139514409, -0.000000000000000000, -0.007781995580013368816 ) ) ;
#10836 = CARTESIAN_POINT ( 'NONE',  ( 2.072287782118878319, 0.000000000000000000, -2.950529333540147015 ) ) ;
#10837 = CARTESIAN_POINT ( 'NONE',  ( -67.81784386561373879, -0.6013392113702856756, -4.340774506266853905 ) ) ;
#10838 = VERTEX_POINT ( 'NONE', #32578 ) ;
#10839 = CARTESIAN_POINT ( 'NONE',  ( -18.67619601524082285, 0.000000000000000000, 3.936400510096834893 ) ) ;
#10840 = CARTESIAN_POINT ( 'NONE',  ( -19.68796468072271111, -4.565544526780662693, 11.82224219410458055 ) ) ;
#10841 = ADVANCED_FACE ( 'NONE', ( #5910 ), #23503, .F. ) ;
#10842 = LINE ( 'NONE', #6312, #32233 ) ;
#10843 = DIRECTION ( 'NONE',  ( -0.9999697198139514409, -0.000000000000000000, -0.007781995580013368816 ) ) ;
#10844 = EDGE_CURVE ( 'NONE', #25146, #23505, #23237, .T. ) ;
#10845 = CARTESIAN_POINT ( 'NONE',  ( -14.43874742113896126, -1.165603555308156514, 2.452632101459367497 ) ) ;
#10846 = EDGE_LOOP ( 'NONE', ( #46306, #4705, #4752, #36011 ) ) ;
#10847 = ORIENTED_EDGE ( 'NONE', *, *, #48004, .T. ) ;
#10848 = CARTESIAN_POINT ( 'NONE',  ( -58.00000000000000711, -8.999999999999998224, -2.749999999999999556 ) ) ;
#10849 = CARTESIAN_POINT ( 'NONE',  ( -24.53374897521541698, 18.49370927080960669, -4.545578601930409413 ) ) ;
#10850 = COLOUR_RGB ( '', 0.72549020, 0.75294118, 0.79215686) ;
#10851 = ORIENTED_EDGE ( 'NONE', *, *, #11282, .F. ) ;
#10852 = EDGE_CURVE ( 'NONE', #29930, #10033, #49883, .T. ) ;
#10853 = DIRECTION ( 'NONE',  ( 0.007781995580012663651, 0.000000000000000000, -0.9999697198139515519 ) ) ;
#10854 = ORIENTED_EDGE ( 'NONE', *, *, #49354, .T. ) ;
#10855 = CARTESIAN_POINT ( 'NONE',  ( -24.28770178542860947, -24.42559627614718565, -2.749999999999994671 ) ) ;
#10856 = ADVANCED_FACE ( 'NONE', ( #10155 ), #10982, .F. ) ;
#10857 = VERTEX_POINT ( 'NONE', #23763 ) ;
#10858 = ORIENTED_EDGE ( 'NONE', *, *, #47969, .T. ) ;
#10859 = FACE_OUTER_BOUND ( 'NONE', #3574, .T. ) ;
#10860 = DIRECTION ( 'NONE',  ( 0.005961354470445682716, -0.6427876096865404731, -0.7660212471507180654 ) ) ;
#10861 = DIRECTION ( 'NONE',  ( 0.000000000000000000, -0.000000000000000000, -1.000000000000000000 ) ) ;
#10862 = ORIENTED_EDGE ( 'NONE', *, *, #29832, .T. ) ;
#10863 = ADVANCED_FACE ( 'NONE', ( #28304 ), #41087, .F. ) ;
#10864 = DIRECTION ( 'NONE',  ( -0.005961354470445682716, -0.6427876096865404731, 0.7660212471507180654 ) ) ;
#10865 = ORIENTED_EDGE ( 'NONE', *, *, #52422, .F. ) ;
#10866 = ORIENTED_EDGE ( 'NONE', *, *, #11680, .F. ) ;
#10867 = ORIENTED_EDGE ( 'NONE', *, *, #48832, .F. ) ;
#10868 = CARTESIAN_POINT ( 'NONE',  ( -13.18788971426693557, 4.981562823951513508, 1.645618023703288246 ) ) ;
#10869 = ORIENTED_EDGE ( 'NONE', *, *, #44388, .F. ) ;
#10870 = DIRECTION ( 'NONE',  ( 0.007781995580012663651, 0.000000000000000000, -0.9999697198139515519 ) ) ;
#10871 = ORIENTED_EDGE ( 'NONE', *, *, #29672, .T. ) ;
#10872 = PLANE ( 'NONE',  #35834 ) ;
#10873 = LINE ( 'NONE', #6913, #46724 ) ;
#10874 = EDGE_LOOP ( 'NONE', ( #4815, #19465, #16652, #53535 ) ) ;
#10875 = DIRECTION ( 'NONE',  ( -0.6427681459581293666, -0.7660444431189770143, -0.005002170337467561935 ) ) ;
#10876 = ORIENTED_EDGE ( 'NONE', *, *, #53485, .F. ) ;
#10877 = VECTOR ( 'NONE', #48739, 1000.000000000000227 ) ;
#10878 = DIRECTION ( 'NONE',  ( -0.5449076811759708816, 0.6444004775717707689, 0.5364919789714475140 ) ) ;
#10879 = PLANE ( 'NONE',  #14822 ) ;
#10880 = LINE ( 'NONE', #28191, #42273 ) ;
#10881 = DIRECTION ( 'NONE',  ( -0.5364919789714478471, 0.6444004775717705469, -0.5449076811759709926 ) ) ;
#10882 = LINE ( 'NONE', #33023, #17857 ) ;
#10883 = PLANE ( 'NONE',  #36432 ) ;
#10884 = LINE ( 'NONE', #36188, #10228 ) ;
#10885 = EDGE_LOOP ( 'NONE', ( #18593, #48165, #157, #52624 ) ) ;
#10886 = EDGE_CURVE ( 'NONE', #38808, #37795, #1640, .T. ) ;
#10887 = ORIENTED_EDGE ( 'NONE', *, *, #558, .F. ) ;
#10888 = CARTESIAN_POINT ( 'NONE',  ( -56.40932156468398517, 3.913516004366899725, 2.245148959471634065 ) ) ;
#10889 = CARTESIAN_POINT ( 'NONE',  ( -19.60834386242827776, 0.000000000000000000, 4.298478389818581213 ) ) ;
#10890 = ADVANCED_FACE ( 'NONE', ( #49340 ), #48673, .F. ) ;
#10891 = CARTESIAN_POINT ( 'NONE',  ( -20.32972687588355853, 2.391131607591508335, 4.502398433284342971 ) ) ;
#10892 = CARTESIAN_POINT ( 'NONE',  ( -11.82833909480979884, 0.000000000000000000, 5.836352465097450093 ) ) ;
#10893 = DIRECTION ( 'NONE',  ( -0.3620778797217457101, 0.000000000000000000, -0.9321478471874540261 ) ) ;
#10894 = ORIENTED_EDGE ( 'NONE', *, *, #18197, .F. ) ;
#10895 = EDGE_CURVE ( 'NONE', #27645, #42294, #20645, .T. ) ;
#10896 = LINE ( 'NONE', #16269, #12291 ) ;
#10897 = PLANE ( 'NONE',  #46804 ) ;
#10898 = ORIENTED_EDGE ( 'NONE', *, *, #37762, .F. ) ;
#10899 = CARTESIAN_POINT ( 'NONE',  ( -20.63919478859656209, 2.714935509636507316, 9.353956982646346674 ) ) ;
#10900 = CARTESIAN_POINT ( 'NONE',  ( -21.47263955680318404, 0.000000000000000000, 5.022634149262071190 ) ) ;
#10901 = ORIENTED_EDGE ( 'NONE', *, *, #15268, .T. ) ;
#10902 = EDGE_CURVE ( 'NONE', #52808, #25477, #34274, .T. ) ;
#10903 = EDGE_CURVE ( 'NONE', #15187, #7720, #54693, .T. ) ;
#10904 = ADVANCED_FACE ( 'NONE', ( #7876 ), #41907, .F. ) ;
#10905 = CARTESIAN_POINT ( 'NONE',  ( -67.40301992698960021, 2.000000000000002220, -2.652841686095984031 ) ) ;
#10906 = CARTESIAN_POINT ( 'NONE',  ( -11.34514022254773735, 0.000000000000000000, 3.454794398023896651 ) ) ;
#10907 = DIRECTION ( 'NONE',  ( 0.005002170337468016433, -0.7660444431189770143, -0.6427681459581293666 ) ) ;
#10908 = DIRECTION ( 'NONE',  ( 0.6427681459581294776, -0.7660444431189769032, 0.005002170337467562802 ) ) ;
#10909 = DIRECTION ( 'NONE',  ( 0.000000000000000000, -1.000000000000000000, 0.000000000000000000 ) ) ;
#10910 = ORIENTED_EDGE ( 'NONE', *, *, #47125, .T. ) ;
#10911 = ORIENTED_EDGE ( 'NONE', *, *, #28773, .T. ) ;
#10912 = DIRECTION ( 'NONE',  ( 0.6427681459581294776, -0.7660444431189769032, 0.005002170337467562802 ) ) ;
#10913 = DIRECTION ( 'NONE',  ( 0.6427681459581294776, -0.7660444431189769032, 0.005002170337467562802 ) ) ;
#10914 = LINE ( 'NONE', #41306, #11551 ) ;
#10915 = LINE ( 'NONE', #54352, #24664 ) ;
#10916 = ADVANCED_FACE ( 'NONE', ( #55264 ), #3859, .F. ) ;
#10917 = CARTESIAN_POINT ( 'NONE',  ( -14.89451260070033456, 3.686347215771511365, 2.349852469050325077 ) ) ;
#10918 = VERTEX_POINT ( 'NONE', #45919 ) ;
#10919 = CARTESIAN_POINT ( 'NONE',  ( 5.592372708928878389, -1.049503284171714013, -2.322659989241096845 ) ) ;
#10920 = VECTOR ( 'NONE', #44303, 999.9999999999998863 ) ;
#10921 = ADVANCED_FACE ( 'NONE', ( #7033 ), #24334, .F. ) ;
#10922 = DIRECTION ( 'NONE',  ( 0.005961354470445682716, -0.6427876096865404731, -0.7660212471507180654 ) ) ;
#10923 = DIRECTION ( 'NONE',  ( 0.5364919789714477361, 0.6444004775717706579, 0.5449076811759711036 ) ) ;
#10924 = EDGE_LOOP ( 'NONE', ( #33622, #33102, #54178, #22872 ) ) ;
#10925 = EDGE_CURVE ( 'NONE', #36151, #11807, #55038, .T. ) ;
#10926 = FACE_OUTER_BOUND ( 'NONE', #38945, .T. ) ;
#10927 = FACE_OUTER_BOUND ( 'NONE', #14815, .T. ) ;
#10928 = CARTESIAN_POINT ( 'NONE',  ( -14.72909745882335386, -1.489407457353157049, 4.847584766220364827 ) ) ;
#10929 = ORIENTED_EDGE ( 'NONE', *, *, #41415, .F. ) ;
#10930 = EDGE_CURVE ( 'NONE', #36112, #7607, #55005, .T. ) ;
#10931 = CARTESIAN_POINT ( 'NONE',  ( -23.33693525117809386, 0.000000000000000000, 5.746789908705562944 ) ) ;
#10932 = ORIENTED_EDGE ( 'NONE', *, *, #17915, .F. ) ;
#10933 = ADVANCED_FACE ( 'NONE', ( #12099 ), #50727, .F. ) ;
#10934 = EDGE_LOOP ( 'NONE', ( #39834, #36295, #5484, #17930 ) ) ;
#10935 = ORIENTED_EDGE ( 'NONE', *, *, #50571, .T. ) ;
#10936 = CARTESIAN_POINT ( 'NONE',  ( -29.00661482377690703, 15.91129896909354180, 4.725528206980505352 ) ) ;
#10937 = EDGE_LOOP ( 'NONE', ( #9384, #55618, #23671, #54637, #1742 ) ) ;
#10938 = ORIENTED_EDGE ( 'NONE', *, *, #23443, .T. ) ;
#10939 = DIRECTION ( 'NONE',  ( 0.007781995580012663651, -3.146120232559066537E-19, -0.9999697198139514409 ) ) ;
#10940 = ORIENTED_EDGE ( 'NONE', *, *, #2922, .T. ) ;
#10941 = ORIENTED_EDGE ( 'NONE', *, *, #5916, .F. ) ;
#10942 = CARTESIAN_POINT ( 'NONE',  ( -16.59339315319826014, -1.489407457353158160, 5.571740525663858357 ) ) ;
#10943 = ORIENTED_EDGE ( 'NONE', *, *, #33278, .T. ) ;
#10944 = ORIENTED_EDGE ( 'NONE', *, *, #11147, .F. ) ;
#10945 = EDGE_LOOP ( 'NONE', ( #18399, #21039, #32060, #32155 ) ) ;
#10946 = FACE_OUTER_BOUND ( 'NONE', #7578, .T. ) ;
#10947 = LINE ( 'NONE', #50418, #45718 ) ;
#10948 = CARTESIAN_POINT ( 'NONE',  ( -63.00984630926863161, 1.788483511016180305, 2.999999999999993339 ) ) ;
#10949 = LINE ( 'NONE', #45063, #46775 ) ;
#10950 = ORIENTED_EDGE ( 'NONE', *, *, #17940, .F. ) ;
#10951 = CARTESIAN_POINT ( 'NONE',  ( -9.510902717614937885, 0.000000000000000000, 6.593051430453025219 ) ) ;
#10952 = ORIENTED_EDGE ( 'NONE', *, *, #24223, .F. ) ;
#10953 = ORIENTED_EDGE ( 'NONE', *, *, #1905, .F. ) ;
#10954 = VECTOR ( 'NONE', #25610, 1000.000000000000227 ) ;
#10955 = CARTESIAN_POINT ( 'NONE',  ( -15.50102849149811135, -0.1191753592594197858, 12.95155240711365430 ) ) ;
#10956 = AXIS2_PLACEMENT_3D ( 'NONE', #30638, #52734, #22654 ) ;
#10957 = CARTESIAN_POINT ( 'NONE',  ( -29.02628690221330388, 15.89994128931277295, -4.726187803958536549 ) ) ;
#10958 = FACE_OUTER_BOUND ( 'NONE', #18350, .T. ) ;
#10959 = CARTESIAN_POINT ( 'NONE',  ( -16.13292578047435910, 0.000000000000000000, 3.048202673938099849 ) ) ;
#10960 = CARTESIAN_POINT ( 'NONE',  ( -20.54126990917373519, -0.1191753592594197858, 4.760553241521720658 ) ) ;
#10961 = ORIENTED_EDGE ( 'NONE', *, *, #44269, .F. ) ;
#10962 = CARTESIAN_POINT ( 'NONE',  ( 0.1285714285714296967, 2.000000000000000000, 5.998622290806041590 ) ) ;
#10963 = EDGE_LOOP ( 'NONE', ( #33540, #54874, #15808, #39798 ) ) ;
#10964 = EDGE_CURVE ( 'NONE', #44493, #45963, #33421, .T. ) ;
#10965 = EDGE_CURVE ( 'NONE', #1437, #38304, #24894, .T. ) ;
#10966 = PLANE ( 'NONE',  #22054 ) ;
#10967 = CARTESIAN_POINT ( 'NONE',  ( -24.87971818958798309, 18.22038254469182661, -4.563127009718482618 ) ) ;
#10968 = CARTESIAN_POINT ( 'NONE',  ( -17.74560456716937296, 0.000000000000000000, 3.774316574337878372 ) ) ;
#10969 = DIRECTION ( 'NONE',  ( 0.6427681459581294776, -0.7660444431189769032, 0.005002170337467562802 ) ) ;
#10970 = EDGE_CURVE ( 'NONE', #27279, #19226, #30279, .T. ) ;
#10971 = CARTESIAN_POINT ( 'NONE',  ( -18.80364065443665211, 0.000000000000000000, 6.520733195092834222 ) ) ;
#10972 = EDGE_LOOP ( 'NONE', ( #51164, #16706, #45561, #17942 ) ) ;
#10973 = DIRECTION ( 'NONE',  ( 0.9999697198139515519, 0.000000000000000000, 0.007781995580013368816 ) ) ;
#10974 = DIRECTION ( 'NONE',  ( -0.005002170337468016433, -0.7660444431189770143, 0.6427681459581293666 ) ) ;
#10975 = CARTESIAN_POINT ( 'NONE',  ( -27.13299098042555002, 16.99303619941258603, -4.657414165320978405 ) ) ;
#10976 = VECTOR ( 'NONE', #28938, 1000.000000000000000 ) ;
#10977 = VECTOR ( 'NONE', #48287, 1000.000000000000227 ) ;
#10978 = DIRECTION ( 'NONE',  ( 0.7660212471507180654, -0.6427876096865404731, 0.005961354470445141482 ) ) ;
#10979 = LINE ( 'NONE', #6197, #26664 ) ;
#10980 = DIRECTION ( 'NONE',  ( 0.007781995580012663651, -3.146120232559066537E-19, -0.9999697198139514409 ) ) ;
#10981 = CARTESIAN_POINT ( 'NONE',  ( -27.56460882755735753, 16.74384151918395247, 4.673983433494172779 ) ) ;
#10982 = PLANE ( 'NONE',  #51393 ) ;
#10983 = LINE ( 'NONE', #1641, #41931 ) ;
#10984 = ORIENTED_EDGE ( 'NONE', *, *, #10087, .T. ) ;
#10985 = VECTOR ( 'NONE', #43986, 999.9999999999998863 ) ;
#10986 = EDGE_CURVE ( 'NONE', #37343, #42711, #21492, .T. ) ;
#10987 = VECTOR ( 'NONE', #42552, 1000.000000000000114 ) ;
#10988 = VERTEX_POINT ( 'NONE', #8717 ) ;
#10989 = VERTEX_POINT ( 'NONE', #30583 ) ;
#10990 = VERTEX_POINT ( 'NONE', #13519 ) ;
#10991 = ADVANCED_FACE ( 'NONE', ( #30834 ), #22029, .F. ) ;
#10992 = EDGE_LOOP ( 'NONE', ( #20906, #37179, #51022, #49441 ) ) ;
#10993 = CARTESIAN_POINT ( 'NONE',  ( -9.413091840428602808, -0.1191753592594190225, 6.874738116430744839 ) ) ;
#10994 = ADVANCED_FACE ( 'NONE', ( #988 ), #52132, .F. ) ;
#10995 = DIRECTION ( 'NONE',  ( -0.8531650599175529814, -0.4028455766673920135, 0.3313982828793697877 ) ) ;
#10996 = EDGE_LOOP ( 'NONE', ( #56192, #3901, #36573, #462 ) ) ;
#10997 = VERTEX_POINT ( 'NONE', #39354 ) ;
#10998 = EDGE_CURVE ( 'NONE', #46093, #54486, #445, .T. ) ;
#10999 = ORIENTED_EDGE ( 'NONE', *, *, #54021, .T. ) ;
#11000 = ORIENTED_EDGE ( 'NONE', *, *, #44997, .T. ) ;
#11001 = CARTESIAN_POINT ( 'NONE',  ( -66.02636694011434315, -9.266119898376031117, 1.786740587087118470 ) ) ;
#11002 = CARTESIAN_POINT ( 'NONE',  ( 2.072287782118878319, 0.000000000000000000, -2.950529333540147015 ) ) ;
#11003 = CARTESIAN_POINT ( 'NONE',  ( -15.86710544311044302, 0.000000000000000000, 13.13336954653252953 ) ) ;
#11004 = EDGE_LOOP ( 'NONE', ( #35504, #26504, #29154, #16225 ) ) ;
#11005 = CARTESIAN_POINT ( 'NONE',  ( 1.086233639165236964, 0.000000000000000000, 2.796443541562362078 ) ) ;
#11006 = AXIS2_PLACEMENT_3D ( 'NONE', #48722, #44714, #9824 ) ;
#11007 = VECTOR ( 'NONE', #27223, 1000.000000000000227 ) ;
#11008 = DIRECTION ( 'NONE',  ( 0.9999697198139515519, 0.000000000000000000, 0.007781995580013368816 ) ) ;
#11009 = PLANE ( 'NONE',  #25723 ) ;
#11010 = CARTESIAN_POINT ( 'NONE',  ( -21.74593062183054926, 4.010151117816509903, 11.90952023678523197 ) ) ;
#11011 = CARTESIAN_POINT ( 'NONE',  ( -10.80846868922008497, -0.1191753592594181482, 7.052288569946153274 ) ) ;
#11012 = VECTOR ( 'NONE', #20540, 1000.000000000000227 ) ;
#11013 = FACE_OUTER_BOUND ( 'NONE', #20075, .T. ) ;
#11014 = DIRECTION ( 'NONE',  ( 0.6427681459581294776, -0.7660444431189769032, 0.005002170337467562802 ) ) ;
#11015 = DIRECTION ( 'NONE',  ( 0.000000000000000000, -0.000000000000000000, -1.000000000000000000 ) ) ;
#11016 = FACE_OUTER_BOUND ( 'NONE', #27911, .T. ) ;
#11017 = ORIENTED_EDGE ( 'NONE', *, *, #12082, .F. ) ;
#11018 = DIRECTION ( 'NONE',  ( 0.005961354470445682716, -0.6427876096865404731, -0.7660212471507180654 ) ) ;
#11019 = ORIENTED_EDGE ( 'NONE', *, *, #7453, .F. ) ;
#11020 = ADVANCED_FACE ( 'NONE', ( #12679 ), #21757, .F. ) ;
#11021 = FACE_OUTER_BOUND ( 'NONE', #5824, .T. ) ;
#11022 = LINE ( 'NONE', #19002, #6890 ) ;
#11023 = CARTESIAN_POINT ( 'NONE',  ( -15.54830832304376820, 0.000000000000000000, 6.176734874211137871 ) ) ;
#11024 = CARTESIAN_POINT ( 'NONE',  ( -15.87635958039733097, 3.686347215771509145, 9.098162144920037164 ) ) ;
#11025 = DIRECTION ( 'NONE',  ( 0.007781995580012662783, 0.000000000000000000, -0.9999697198139514409 ) ) ;
#11026 = CARTESIAN_POINT ( 'NONE',  ( 4.848100717410754434, 0.000000000000000000, -2.061810099490656079 ) ) ;
#11027 = EDGE_CURVE ( 'NONE', #22884, #370, #9545, .T. ) ;
#11028 = ADVANCED_FACE ( 'NONE', ( #5000 ), #9243, .F. ) ;
#11029 = VECTOR ( 'NONE', #26656, 1000.000000000000227 ) ;
#11030 = DIRECTION ( 'NONE',  ( 0.005961354470445682716, -0.6427876096865404731, -0.7660212471507180654 ) ) ;
#11031 =( LENGTH_UNIT ( ) NAMED_UNIT ( * ) SI_UNIT ( .MILLI., .METRE. ) );
#11032 = CARTESIAN_POINT ( 'NONE',  ( -17.93139508144814442, 0.000000000000000000, 13.85596890686001537 ) ) ;
#11033 = LINE ( 'NONE', #11868, #53828 ) ;
#11034 = DIRECTION ( 'NONE',  ( 0.007781995580012663651, -3.146120232559066537E-19, -0.9999697198139514409 ) ) ;
#11035 = CARTESIAN_POINT ( 'NONE',  ( -12.06136745912998975, 0.000000000000000000, 1.771886216610035092 ) ) ;
#11036 = PLANE ( 'NONE',  #16912 ) ;
#11037 = PLANE ( 'NONE',  #91 ) ;
#11038 = FACE_OUTER_BOUND ( 'NONE', #22742, .T. ) ;
#11039 = DIRECTION ( 'NONE',  ( 0.000000000000000000, -0.000000000000000000, -1.000000000000000000 ) ) ;
#11040 = LINE ( 'NONE', #10789, #20188 ) ;
#11041 = ORIENTED_EDGE ( 'NONE', *, *, #20974, .F. ) ;
#11042 = LINE ( 'NONE', #41699, #9490 ) ;
#11043 = ORIENTED_EDGE ( 'NONE', *, *, #8329, .T. ) ;
#11044 = CARTESIAN_POINT ( 'NONE',  ( -15.80102324005015824, -2.784623065533160524, 2.930131093732116554 ) ) ;
#11045 = CARTESIAN_POINT ( 'NONE',  ( -13.67694686726901665, 0.000000000000000000, 4.544643948957142854 ) ) ;
#11046 = VECTOR ( 'NONE', #18242, 1000.000000000000000 ) ;
#11047 = VECTOR ( 'NONE', #42943, 1000.000000000000227 ) ;
#11048 = ORIENTED_EDGE ( 'NONE', *, *, #40485, .T. ) ;
#11049 = ORIENTED_EDGE ( 'NONE', *, *, #50599, .T. ) ;
#11050 = CARTESIAN_POINT ( 'NONE',  ( -19.60912206198628027, -0.1191753592594197858, 4.398475361799976113 ) ) ;
#11051 = ORIENTED_EDGE ( 'NONE', *, *, #27316, .T. ) ;
#11052 = ORIENTED_EDGE ( 'NONE', *, *, #13652, .F. ) ;
#11053 = VECTOR ( 'NONE', #27887, 999.9999999999998863 ) ;
#11054 = ORIENTED_EDGE ( 'NONE', *, *, #52505, .T. ) ;
#11055 = CARTESIAN_POINT ( 'NONE',  ( -18.86354292863559579, 0.000000000000000000, 14.21804678658176080 ) ) ;
#11056 = CARTESIAN_POINT ( 'NONE',  ( -12.60458797795435615, 0.000000000000000000, 11.86609696750642229 ) ) ;
#11057 = DIRECTION ( 'NONE',  ( 0.9999697198139515519, 0.000000000000000000, 0.007781995580013368816 ) ) ;
#11058 = VERTEX_POINT ( 'NONE', #12949 ) ;
#11059 = EDGE_CURVE ( 'NONE', #12635, #6150, #39910, .T. ) ;
#11060 = VECTOR ( 'NONE', #35405, 1000.000000000000114 ) ;
#11061 = ORIENTED_EDGE ( 'NONE', *, *, #3840, .T. ) ;
#11062 = VECTOR ( 'NONE', #29465, 1000.000000000000114 ) ;
#11063 = PLANE ( 'NONE',  #32977 ) ;
#11064 = LINE ( 'NONE', #53962, #26374 ) ;
#11065 = ORIENTED_EDGE ( 'NONE', *, *, #37015, .F. ) ;
#11066 = DIRECTION ( 'NONE',  ( -0.9999697198139514409, -0.000000000000000000, -0.007781995580013368816 ) ) ;
#11067 = ORIENTED_EDGE ( 'NONE', *, *, #3587, .F. ) ;
#11068 = CARTESIAN_POINT ( 'NONE',  ( -18.32598891683381126, -5.698858183938163791, 13.15316534217173938 ) ) ;
#11069 = FACE_OUTER_BOUND ( 'NONE', #19859, .T. ) ;
#11070 = ADVANCED_FACE ( 'NONE', ( #43059 ), #35375, .F. ) ;
#11071 = EDGE_CURVE ( 'NONE', #46056, #46010, #39071, .T. ) ;
#11072 = ORIENTED_EDGE ( 'NONE', *, *, #40665, .F. ) ;
#11073 = DIRECTION ( 'NONE',  ( 0.9997703818010067467, -0.000000000000000000, -0.02142857142857158143 ) ) ;
#11074 = VECTOR ( 'NONE', #6953, 999.9999999999998863 ) ;
#11075 = EDGE_CURVE ( 'NONE', #49206, #5052, #34527, .T. ) ;
#11076 = EDGE_CURVE ( 'NONE', #50902, #38693, #47296, .T. ) ;
#11077 = CARTESIAN_POINT ( 'NONE',  ( 2.072287782118878319, -1.000000000000000000, -2.950529333540147015 ) ) ;
#11078 = ORIENTED_EDGE ( 'NONE', *, *, #2314, .T. ) ;
#11079 = CARTESIAN_POINT ( 'NONE',  ( -26.13493519185646008, 0.000000000000000000, 7.033017491833586377 ) ) ;
#11080 = FACE_OUTER_BOUND ( 'NONE', #1280, .T. ) ;
#11081 = AXIS2_PLACEMENT_3D ( 'NONE', #9940, #1684, #10776 ) ;
#11082 = DIRECTION ( 'NONE',  ( 0.005002170337468016433, -0.7660444431189770143, -0.6427681459581293666 ) ) ;
#11083 = EDGE_CURVE ( 'NONE', #46790, #51656, #38810, .T. ) ;
#11084 = ORIENTED_EDGE ( 'NONE', *, *, #42469, .T. ) ;
#11085 = AXIS2_PLACEMENT_3D ( 'NONE', #15800, #55537, #16641 ) ;
#11086 = VECTOR ( 'NONE', #25846, 1000.000000000000227 ) ;
#11087 = EDGE_CURVE ( 'NONE', #16268, #3020, #34814, .T. ) ;
#11088 = DIRECTION ( 'NONE',  ( 0.3583679495452941066, 0.9335804264972041855, 0.000000000000000000 ) ) ;
#11089 = FACE_OUTER_BOUND ( 'NONE', #7973, .T. ) ;
#11090 = FACE_OUTER_BOUND ( 'NONE', #14178, .T. ) ;
#11091 = DIRECTION ( 'NONE',  ( -0.005002170337468016433, -0.7660444431189770143, 0.6427681459581293666 ) ) ;
#11092 = CARTESIAN_POINT ( 'NONE',  ( -23.44701637808619665, 18.93456746265863799, 4.495868649597294819 ) ) ;
#11093 = EDGE_CURVE ( 'NONE', #12998, #21622, #26288, .T. ) ;
#11094 = DIRECTION ( 'NONE',  ( 0.005961354470445682716, -0.6427876096865404731, -0.7660212471507180654 ) ) ;
#11095 = AXIS2_PLACEMENT_3D ( 'NONE', #30064, #47371, #796 ) ;
#11096 = DIRECTION ( 'NONE',  ( 0.5449076811759707706, 0.6444004775717708799, -0.5364919789714476250 ) ) ;
#11097 = VECTOR ( 'NONE', #3908, 1000.000000000000114 ) ;
#11098 = VERTEX_POINT ( 'NONE', #9831 ) ;
#11099 = CARTESIAN_POINT ( 'NONE',  ( 2.072287782118878319, 0.000000000000000000, -2.950529333540147015 ) ) ;
#11100 = LINE ( 'NONE', #19903, #44066 ) ;
#11101 = CARTESIAN_POINT ( 'NONE',  ( -67.40002305061796051, -5.356753701341379876E-12, -4.884162593219334880 ) ) ;
#11102 = EDGE_LOOP ( 'NONE', ( #38699, #27287, #40386, #32586 ) ) ;
#11103 = CARTESIAN_POINT ( 'NONE',  ( -26.13493519185646008, 0.000000000000000000, 7.033017491833586377 ) ) ;
#11104 = DIRECTION ( 'NONE',  ( 0.007781995580012663651, -3.146120232559066537E-19, -0.9999697198139514409 ) ) ;
#11105 = EDGE_CURVE ( 'NONE', #33009, #21477, #31684, .T. ) ;
#11106 = CARTESIAN_POINT ( 'NONE',  ( -15.54699066865448565, 0.000000000000000000, 6.007419114916161540 ) ) ;
#11107 = FACE_OUTER_BOUND ( 'NONE', #2117, .T. ) ;
#11108 = LINE ( 'NONE', #54533, #21135 ) ;
#11109 = EDGE_CURVE ( 'NONE', #51910, #5412, #52970, .T. ) ;
#11110 = ORIENTED_EDGE ( 'NONE', *, *, #393, .F. ) ;
#11111 = ORIENTED_EDGE ( 'NONE', *, *, #49199, .F. ) ;
#11112 = DIRECTION ( 'NONE',  ( 0.9932609354084158682, 0.1139014070068027351, -0.02142857142857155367 ) ) ;
#11113 = CARTESIAN_POINT ( 'NONE',  ( -12.19375721922749278, -0.1191753592594181482, 5.933511724868832715 ) ) ;
#11114 = EDGE_LOOP ( 'NONE', ( #20554, #4367, #25027, #46130 ) ) ;
#11115 = DIRECTION ( 'NONE',  ( 0.5449076811759707706, 0.6444004775717708799, -0.5364919789714476250 ) ) ;
#11116 = VECTOR ( 'NONE', #30947, 999.9999999999998863 ) ;
#11117 = ORIENTED_EDGE ( 'NONE', *, *, #43314, .F. ) ;
#11118 = PLANE ( 'NONE',  #29244 ) ;
#11119 = ORIENTED_EDGE ( 'NONE', *, *, #3357, .T. ) ;
#11120 = VERTEX_POINT ( 'NONE', #49267 ) ;
#11121 = CARTESIAN_POINT ( 'NONE',  ( -15.40103151951671734, 0.000000000000000000, 12.95233060667165681 ) ) ;
#11122 = VECTOR ( 'NONE', #17709, 1000.000000000000114 ) ;
#11123 = DIRECTION ( 'NONE',  ( -0.005002170337468016433, -0.7660444431189770143, 0.6427681459581293666 ) ) ;
#11124 = LINE ( 'NONE', #40949, #12144 ) ;
#11125 = EDGE_LOOP ( 'NONE', ( #10961, #16060, #53253, #44672 ) ) ;
#11126 = VECTOR ( 'NONE', #4601, 1000.000000000000114 ) ;
#11127 = VECTOR ( 'NONE', #8688, 999.9999999999998863 ) ;
#11128 = CARTESIAN_POINT ( 'NONE',  ( -16.09911561167002958, 4.010151117816511679, 2.807430147226621209 ) ) ;
#11129 = ADVANCED_FACE ( 'NONE', ( #15208 ), #27707, .F. ) ;
#11130 = EDGE_LOOP ( 'NONE', ( #26431, #49283, #12169, #16528 ) ) ;
#11131 = VERTEX_POINT ( 'NONE', #10089 ) ;
#11132 = AXIS2_PLACEMENT_3D ( 'NONE', #52426, #13521, #48431 ) ;
#11133 = ORIENTED_EDGE ( 'NONE', *, *, #1593, .T. ) ;
#11134 = CARTESIAN_POINT ( 'NONE',  ( -19.54294029912376729, 21.18270206417094315, -4.260498045023555669 ) ) ;
#11135 = VECTOR ( 'NONE', #3143, 999.9999999999998863 ) ;
#11136 = ORIENTED_EDGE ( 'NONE', *, *, #12958, .F. ) ;
#11137 = PLANE ( 'NONE',  #30265 ) ;
#11138 = ORIENTED_EDGE ( 'NONE', *, *, #41766, .F. ) ;
#11139 = DIRECTION ( 'NONE',  ( 0.007781995580012662783, 0.000000000000000000, -0.9999697198139514409 ) ) ;
#11140 = CARTESIAN_POINT ( 'NONE',  ( -16.75815173624665277, 0.000000000000000000, 8.213985998274722533 ) ) ;
#11141 = ADVANCED_FACE ( 'NONE', ( #44444 ), #27986, .F. ) ;
#11142 = ORIENTED_EDGE ( 'NONE', *, *, #43481, .F. ) ;
#11144 = VECTOR ( 'NONE', #31211, 1000.000000000000227 ) ;
#11143 = DIRECTION ( 'NONE',  ( 0.007781995580012663651, -3.146120232559066537E-19, -0.9999697198139514409 ) ) ;
#11145 = ORIENTED_EDGE ( 'NONE', *, *, #2754, .T. ) ;
#11146 = VECTOR ( 'NONE', #48871, 1000.000000000000227 ) ;
#11147 = EDGE_CURVE ( 'NONE', #40714, #27501, #32247, .T. ) ;
#11148 = CARTESIAN_POINT ( 'NONE',  ( -13.25450402488150203, 4.981562823951511731, 10.20541388017194073 ) ) ;
#11149 = FACE_OUTER_BOUND ( 'NONE', #46539, .T. ) ;
#11150 = FACE_OUTER_BOUND ( 'NONE', #44521, .T. ) ;
#11151 = CARTESIAN_POINT ( 'NONE',  ( -13.27065584551087163, 0.000000000000000000, 12.04557950825129176 ) ) ;
#11152 = DIRECTION ( 'NONE',  ( -0.7660212471507179544, -0.6427876096865405842, -0.005961354470445141482 ) ) ;
#11153 = DIRECTION ( 'NONE',  ( 0.005002170337468016433, -0.7660444431189770143, -0.6427681459581293666 ) ) ;
#11154 = FACE_OUTER_BOUND ( 'NONE', #10924, .T. ) ;
#11155 = ORIENTED_EDGE ( 'NONE', *, *, #6427, .F. ) ;
#11156 = VECTOR ( 'NONE', #9205, 1000.000000000000227 ) ;
#11157 = ORIENTED_EDGE ( 'NONE', *, *, #53206, .T. ) ;
#11158 = EDGE_CURVE ( 'NONE', #39217, #49206, #18909, .T. ) ;
#11159 = CARTESIAN_POINT ( 'NONE',  ( 0.09621548157177267635, -1.683565401097097292, -3.964956190634383833E-16 ) ) ;
#11160 = DIRECTION ( 'NONE',  ( -0.5364919789714478471, 0.6444004775717705469, -0.5449076811759709926 ) ) ;
#11161 = VECTOR ( 'NONE', #2858, 999.9999999999998863 ) ;
#11162 = CARTESIAN_POINT ( 'NONE',  ( -16.06709938707323460, 0.000000000000000000, 13.13181314741652628 ) ) ;
#11163 = EDGE_CURVE ( 'NONE', #34812, #49013, #3035, .T. ) ;
#11164 = DIRECTION ( 'NONE',  ( -0.5364919789714478471, 0.6444004775717705469, -0.5449076811759709926 ) ) ;
#11165 = CARTESIAN_POINT ( 'NONE',  ( -10.31509125732617171, -0.1191753592594185784, 3.362807449136518745 ) ) ;
#11166 = VERTEX_POINT ( 'NONE', #27402 ) ;
#11167 = LINE ( 'NONE', #54900, #45846 ) ;
#11168 = DIRECTION ( 'NONE',  ( 0.9999697198139515519, 0.000000000000000000, 0.007781995580013368816 ) ) ;
#11169 = ORIENTED_EDGE ( 'NONE', *, *, #35516, .F. ) ;
#11171 = DIRECTION ( 'NONE',  ( 0.005002170337468016433, -0.7660444431189770143, -0.6427681459581293666 ) ) ;
#11170 = VECTOR ( 'NONE', #7162, 1000.000000000000114 ) ;
#11172 = LINE ( 'NONE', #50903, #42219 ) ;
#11173 = VERTEX_POINT ( 'NONE', #36785 ) ;
#11174 = AXIS2_PLACEMENT_3D ( 'NONE', #26034, #39067, #26285 ) ;
#11175 = EDGE_CURVE ( 'NONE', #44131, #26974, #53800, .T. ) ;
#11176 = VECTOR ( 'NONE', #43861, 999.9999999999998863 ) ;
#11177 = DIRECTION ( 'NONE',  ( 0.007781995580012663651, 0.000000000000000000, -0.9999697198139515519 ) ) ;
#11178 = FACE_OUTER_BOUND ( 'NONE', #55940, .T. ) ;
#11179 = CARTESIAN_POINT ( 'NONE',  ( -3.789478469635834568, -7.588859415764141580, -1.746411446826717340 ) ) ;
#11180 = DIRECTION ( 'NONE',  ( 0.000000000000000000, -1.000000000000000000, 0.000000000000000000 ) ) ;
#11181 = DIRECTION ( 'NONE',  ( 0.7660212471507180654, -0.6427876096865404731, 0.005961354470445141482 ) ) ;
#11182 = EDGE_CURVE ( 'NONE', #27005, #19751, #2408, .T. ) ;
#11183 = ORIENTED_EDGE ( 'NONE', *, *, #19735, .T. ) ;
#11184 = VECTOR ( 'NONE', #36642, 1000.000000000000000 ) ;
#11185 = VECTOR ( 'NONE', #54526, 1000.000000000000000 ) ;
#11186 = ORIENTED_EDGE ( 'NONE', *, *, #29565, .F. ) ;
#11187 = CARTESIAN_POINT ( 'NONE',  ( -15.86710544311044302, 0.000000000000000000, 13.13336954653252953 ) ) ;
#11188 = DIRECTION ( 'NONE',  ( -0.7660212471507179544, -0.6427876096865405842, -0.005961354470445141482 ) ) ;
#11189 = LINE ( 'NONE', #37596, #53315 ) ;
#11190 = DIRECTION ( 'NONE',  ( 0.007781995580012663651, -3.146120232559066537E-19, -0.9999697198139514409 ) ) ;
#11191 = CARTESIAN_POINT ( 'NONE',  ( -16.81345671998191449, 0.000000000000000000, 3.412238694616132495 ) ) ;
#11192 = LINE ( 'NONE', #31943, #10441 ) ;
#11193 = EDGE_LOOP ( 'NONE', ( #53811, #32851, #46850, #44740 ) ) ;
#11194 = CARTESIAN_POINT ( 'NONE',  ( -13.73672976910459909, 0.000000000000000000, 12.22661844811216270 ) ) ;
#11195 = FACE_OUTER_BOUND ( 'NONE', #42822, .T. ) ;
#11196 = DIRECTION ( 'NONE',  ( 0.000000000000000000, -1.000000000000000000, 0.000000000000000000 ) ) ;
#11197 = ORIENTED_EDGE ( 'NONE', *, *, #39971, .T. ) ;
#11198 = AXIS2_PLACEMENT_3D ( 'NONE', #43488, #21646, #313 ) ;
#11199 = CARTESIAN_POINT ( 'NONE',  ( -9.296538506125733292, 0.000000000000000000, 4.748059313280206695 ) ) ;
#11200 = PLANE ( 'NONE',  #30463 ) ;
#11201 = VECTOR ( 'NONE', #3484, 1000.000000000000227 ) ;
#11202 = FACE_OUTER_BOUND ( 'NONE', #16898, .T. ) ;
#11203 = EDGE_LOOP ( 'NONE', ( #17051, #41264, #551, #7576 ) ) ;
#11204 = PLANE ( 'NONE',  #11375 ) ;
#11205 = EDGE_CURVE ( 'NONE', #25448, #50616, #14086, .T. ) ;
#11206 = AXIS2_PLACEMENT_3D ( 'NONE', #27064, #27324, #40406 ) ;
#11207 = ORIENTED_EDGE ( 'NONE', *, *, #51450, .F. ) ;
#11208 = EDGE_LOOP ( 'NONE', ( #53462, #51161, #12914, #33883 ) ) ;
#11209 = VERTEX_POINT ( 'NONE', #10678 ) ;
#11210 = EDGE_CURVE ( 'NONE', #29764, #51468, #53525, .T. ) ;
#11211 = ORIENTED_EDGE ( 'NONE', *, *, #2240, .T. ) ;
#11212 = EDGE_CURVE ( 'NONE', #428, #34236, #19440, .T. ) ;
#11213 = ORIENTED_EDGE ( 'NONE', *, *, #11557, .F. ) ;
#11214 = VECTOR ( 'NONE', #14920, 1000.000000000000114 ) ;
#11215 = CARTESIAN_POINT ( 'NONE',  ( -20.54204810873173415, 0.000000000000000000, 4.860550213503115558 ) ) ;
#11217 = ADVANCED_FACE ( 'NONE', ( #14628 ), #31950, .F. ) ;
#11216 = ORIENTED_EDGE ( 'NONE', *, *, #47202, .F. ) ;
#11218 = ADVANCED_FACE ( 'NONE', ( #18620 ), #35966, .F. ) ;
#11219 = EDGE_CURVE ( 'NONE', #52348, #23769, #3249, .T. ) ;
#11220 = ORIENTED_EDGE ( 'NONE', *, *, #27054, .T. ) ;
#11221 = CARTESIAN_POINT ( 'NONE',  ( -19.12962290826653700, 0.000000000000000000, 14.40064212555863854 ) ) ;
#11222 = ORIENTED_EDGE ( 'NONE', *, *, #39773, .T. ) ;
#11223 = ORIENTED_EDGE ( 'NONE', *, *, #45570, .T. ) ;
#11224 = ORIENTED_EDGE ( 'NONE', *, *, #39015, .F. ) ;
#11225 = VECTOR ( 'NONE', #37170, 1000.000000000000227 ) ;
#11226 = VECTOR ( 'NONE', #5135, 999.9999999999998863 ) ;
#11227 = CARTESIAN_POINT ( 'NONE',  ( -13.17065887352947762, -0.1191753592594197858, 12.04635770780929427 ) ) ;
#11228 = FACE_OUTER_BOUND ( 'NONE', #21711, .T. ) ;
#11229 = CARTESIAN_POINT ( 'NONE',  ( -15.50102849149811135, -0.1191753592594197858, 12.95155240711365430 ) ) ;
#11230 = DIRECTION ( 'NONE',  ( 0.005961354470445682716, -0.6427876096865404731, -0.7660212471507180654 ) ) ;
#11231 = PLANE ( 'NONE',  #25579 ) ;
#11232 = ORIENTED_EDGE ( 'NONE', *, *, #45277, .F. ) ;
#11233 = ORIENTED_EDGE ( 'NONE', *, *, #14094, .T. ) ;
#11234 = ADVANCED_FACE ( 'NONE', ( #28822 ), #50669, .F. ) ;
#11235 = CARTESIAN_POINT ( 'NONE',  ( -16.29770654730013035, 0.000000000000000000, 8.756227372595473568 ) ) ;
#11236 = CARTESIAN_POINT ( 'NONE',  ( -20.18473747654950046, 0.000000000000000000, 4.863330887462772978 ) ) ;
#11237 = EDGE_CURVE ( 'NONE', #9210, #49710, #37898, .T. ) ;
#11238 = CARTESIAN_POINT ( 'NONE',  ( -37.63793934321780199, 10.92800143433129456, -4.933120776947167663 ) ) ;
#11239 = PLANE ( 'NONE',  #27641 ) ;
#11240 = VECTOR ( 'NONE', #30440, 999.9999999999998863 ) ;
#11241 = EDGE_CURVE ( 'NONE', #6281, #15209, #55205, .T. ) ;
#11242 = DIRECTION ( 'NONE',  ( -0.005961354470445682716, -0.6427876096865404731, 0.7660212471507180654 ) ) ;
#11243 = CARTESIAN_POINT ( 'NONE',  ( -16.48333022373650536, 0.000000000000000000, 6.908122457190647658 ) ) ;
#11244 = ORIENTED_EDGE ( 'NONE', *, *, #14063, .T. ) ;
#11245 = DIRECTION ( 'NONE',  ( 0.9999697198139515519, 0.000000000000000000, 0.007781995580013368816 ) ) ;
#11246 = AXIS2_PLACEMENT_3D ( 'NONE', #46719, #50124, #33109 ) ;
#11247 = EDGE_LOOP ( 'NONE', ( #34547, #49355, #33641, #19086 ) ) ;
#11248 = EDGE_CURVE ( 'NONE', #22811, #6333, #25386, .T. ) ;
#11249 = DIRECTION ( 'NONE',  ( -0.9999697198139514409, -0.000000000000000000, -0.007781995580013368816 ) ) ;
#11250 = PLANE ( 'NONE',  #9737 ) ;
#11251 = CARTESIAN_POINT ( 'NONE',  ( -14.99882292130570072, -0.1191753592594177180, 8.127674473807362077 ) ) ;
#11252 = AXIS2_PLACEMENT_3D ( 'NONE', #46210, #52716, #772 ) ;
#11253 = CARTESIAN_POINT ( 'NONE',  ( -11.83851765444165061, 0.000000000000000000, 7.144275518833531180 ) ) ;
#11254 = DIRECTION ( 'NONE',  ( 0.5449076811759707706, 0.6444004775717708799, -0.5364919789714476250 ) ) ;
#11255 = ORIENTED_EDGE ( 'NONE', *, *, #19785, .F. ) ;
#11256 = VECTOR ( 'NONE', #43542, 999.9999999999998863 ) ;
#11257 = DIRECTION ( 'NONE',  ( 0.000000000000000000, -0.000000000000000000, -1.000000000000000000 ) ) ;
#11258 = PLANE ( 'NONE',  #37681 ) ;
#11259 = FACE_OUTER_BOUND ( 'NONE', #26881, .T. ) ;
#11260 = CIRCLE ( 'NONE', #9440, 0.5000000000000004441 ) ;
#11261 = CARTESIAN_POINT ( 'NONE',  ( -14.94760462649100496, 0.000000000000000000, 2.488088991209854051 ) ) ;
#11262 = LINE ( 'NONE', #19214, #47550 ) ;
#11263 = DIRECTION ( 'NONE',  ( -0.6427681459581293666, -0.7660444431189770143, -0.005002170337467561935 ) ) ;
#11264 = PLANE ( 'NONE',  #19317 ) ;
#11265 = VECTOR ( 'NONE', #23500, 999.9999999999998863 ) ;
#11266 = VECTOR ( 'NONE', #7864, 999.9999999999998863 ) ;
#11267 = LINE ( 'NONE', #49634, #25989 ) ;
#11268 = DIRECTION ( 'NONE',  ( -0.9999697198139514409, -0.000000000000000000, -0.007781995580013368816 ) ) ;
#11269 = ORIENTED_EDGE ( 'NONE', *, *, #23120, .T. ) ;
#11270 = EDGE_LOOP ( 'NONE', ( #56160, #10865, #680, #38077 ) ) ;
#11271 = VECTOR ( 'NONE', #46997, 999.9999999999998863 ) ;
#11272 = ORIENTED_EDGE ( 'NONE', *, *, #23129, .F. ) ;
#11273 = ORIENTED_EDGE ( 'NONE', *, *, #29887, .T. ) ;
#11274 = ORIENTED_EDGE ( 'NONE', *, *, #47067, .T. ) ;
#11275 = VECTOR ( 'NONE', #51930, 1000.000000000000000 ) ;
#11276 = EDGE_LOOP ( 'NONE', ( #28444, #9832, #48569, #35141 ) ) ;
#11277 = DIRECTION ( 'NONE',  ( 0.007781995580012663651, 0.000000000000000000, -0.9999697198139515519 ) ) ;
#11278 = CARTESIAN_POINT ( 'NONE',  ( -10.34523968761605772, -0.1191753592594198830, 7.236815996152489383 ) ) ;
#11279 = CARTESIAN_POINT ( 'NONE',  ( -69.05674355170637568, -0.2656369956482378947, 7.481505251583919325 ) ) ;
#11280 = VECTOR ( 'NONE', #48309, 999.9999999999998863 ) ;
#11281 = ADVANCED_FACE ( 'NONE', ( #11760 ), #20273, .F. ) ;
#11282 = EDGE_CURVE ( 'NONE', #5725, #11899, #37059, .T. ) ;
#11283 = EDGE_LOOP ( 'NONE', ( #31728, #48581, #17399, #29032 ) ) ;
#11284 = CARTESIAN_POINT ( 'NONE',  ( -22.40634380310664397, 0.000000000000000000, 5.584705972946605534 ) ) ;
#11285 = EDGE_LOOP ( 'NONE', ( #30384, #43766, #40189, #30592 ) ) ;
#11286 = EDGE_CURVE ( 'NONE', #10342, #49938, #33067, .T. ) ;
#11287 = VERTEX_POINT ( 'NONE', #29076 ) ;
#11288 = VECTOR ( 'NONE', #46725, 999.9999999999998863 ) ;
#11289 = CARTESIAN_POINT ( 'NONE',  ( -65.57807222826096449, -9.214712059194194893, -3.769581895395211379 ) ) ;
#11290 = VECTOR ( 'NONE', #23022, 999.9999999999998863 ) ;
#11291 = CARTESIAN_POINT ( 'NONE',  ( -18.14631431975934817, 0.000000000000000000, 7.464518856455165441 ) ) ;
#11292 = DIRECTION ( 'NONE',  ( 0.9999697198139515519, 0.000000000000000000, 0.007781995580013368816 ) ) ;
#11293 = VERTEX_POINT ( 'NONE', #15453 ) ;
#11294 = DIRECTION ( 'NONE',  ( 0.7660212471507180654, -0.6427876096865404731, 0.005961354470445141482 ) ) ;
#11295 = ORIENTED_EDGE ( 'NONE', *, *, #10308, .T. ) ;
#11296 = AXIS2_PLACEMENT_3D ( 'NONE', #45130, #32055, #49376 ) ;
#11297 = LINE ( 'NONE', #20375, #53616 ) ;
#11298 = FACE_OUTER_BOUND ( 'NONE', #37330, .T. ) ;
#11299 = ADVANCED_FACE ( 'NONE', ( #6970 ), #24277, .F. ) ;
#11300 = AXIS2_PLACEMENT_3D ( 'NONE', #6390, #40756, #15726 ) ;
#11301 = LINE ( 'NONE', #37146, #13632 ) ;
#11302 = PLANE ( 'NONE',  #25145 ) ;
#11303 = VECTOR ( 'NONE', #26775, 1000.000000000000114 ) ;
#11304 = CARTESIAN_POINT ( 'NONE',  ( -11.36804826722768702, 24.91136206679766829, 3.000000000000000000 ) ) ;
#11305 = DIRECTION ( 'NONE',  ( 0.000000000000000000, -1.000000000000000000, 0.000000000000000000 ) ) ;
#11306 = LINE ( 'NONE', #45958, #24882 ) ;
#11307 = EDGE_CURVE ( 'NONE', #9919, #15150, #16573, .T. ) ;
#11308 = DIRECTION ( 'NONE',  ( 0.005961354470445682716, -0.6427876096865404731, -0.7660212471507180654 ) ) ;
#11309 = PLANE ( 'NONE',  #10250 ) ;
#11310 = VERTEX_POINT ( 'NONE', #24822 ) ;
#11311 = CARTESIAN_POINT ( 'NONE',  ( -15.60102546347950536, 0.000000000000000000, 12.95077420755565356 ) ) ;
#11312 = EDGE_LOOP ( 'NONE', ( #3646, #48317, #37175, #50405 ) ) ;
#11313 = ADVANCED_FACE ( 'NONE', ( #16039 ), #46975, .F. ) ;
#11314 = CARTESIAN_POINT ( 'NONE',  ( -18.02786093087172503, -2.622721114510660367, 7.988897312896254377 ) ) ;
#11315 = CARTESIAN_POINT ( 'NONE',  ( -11.30636317915456779, -0.1191753592594197858, 11.32220194836580340 ) ) ;
#11316 = CARTESIAN_POINT ( 'NONE',  ( -18.21022926198954295, -3.432230869623162928, 3.845286450084705265 ) ) ;
#11317 = CARTESIAN_POINT ( 'NONE',  ( -24.53375310857961367, 18.49370688441070953, 4.545578210335888159 ) ) ;
#11318 = PLANE ( 'NONE',  #26792 ) ;
#11319 = EDGE_CURVE ( 'NONE', #26378, #39170, #50086, .T. ) ;
#11320 = VECTOR ( 'NONE', #2525, 999.9999999999998863 ) ;
#11321 = CARTESIAN_POINT ( 'NONE',  ( 2.072287782118878319, 0.000000000000000000, -2.950529333540147015 ) ) ;
#11322 = VECTOR ( 'NONE', #40518, 1000.000000000000000 ) ;
#11323 = ORIENTED_EDGE ( 'NONE', *, *, #35942, .F. ) ;
#11324 = PLANE ( 'NONE',  #54602 ) ;
#11325 = LINE ( 'NONE', #15311, #15717 ) ;
#11326 = LINE ( 'NONE', #54756, #24010 ) ;
#11327 = CARTESIAN_POINT ( 'NONE',  ( -12.77501498680632608, -4.727446477803164626, 1.692740485850688481 ) ) ;
#11328 = VECTOR ( 'NONE', #1557, 1000.000000000000000 ) ;
#11329 = DIRECTION ( 'NONE',  ( 0.005002170337468016433, -0.7660444431189770143, -0.6427681459581293666 ) ) ;
#11330 = PLANE ( 'NONE',  #5554 ) ;
#11331 = VECTOR ( 'NONE', #48535, 999.9999999999998863 ) ;
#11332 = DIRECTION ( 'NONE',  ( -0.005002170337468016433, -0.7660444431189770143, 0.6427681459581293666 ) ) ;
#11333 = LINE ( 'NONE', #29199, #49596 ) ;
#11334 = LINE ( 'NONE', #41451, #53762 ) ;
#11335 = EDGE_LOOP ( 'NONE', ( #51249, #44482, #56132, #26658 ) ) ;
#11336 = CARTESIAN_POINT ( 'NONE',  ( 0.4518049228021099872, -3.655895688227116747, -5.998622290806042479 ) ) ;
#11337 = VECTOR ( 'NONE', #11139, 1000.000000000000227 ) ;
#11338 = VECTOR ( 'NONE', #13434, 999.9999999999998863 ) ;
#11339 = ORIENTED_EDGE ( 'NONE', *, *, #16387, .T. ) ;
#11340 = AXIS2_PLACEMENT_3D ( 'NONE', #7700, #25032, #3702 ) ;
#11341 = DIRECTION ( 'NONE',  ( -0.6427681459581293666, -0.7660444431189770143, -0.005002170337467561935 ) ) ;
#11342 = LINE ( 'NONE', #35876, #27392 ) ;
#11343 = AXIS2_PLACEMENT_3D ( 'NONE', #38639, #21603, #12223 ) ;
#11344 = VERTEX_POINT ( 'NONE', #12029 ) ;
#11345 = VERTEX_POINT ( 'NONE', #33363 ) ;
#11346 = DIRECTION ( 'NONE',  ( -0.005002170337468016433, -0.7660444431189770143, 0.6427681459581293666 ) ) ;
#11347 = AXIS2_PLACEMENT_3D ( 'NONE', #34970, #17337, #30956 ) ;
#11348 = ORIENTED_EDGE ( 'NONE', *, *, #3007, .T. ) ;
#11349 = VECTOR ( 'NONE', #41615, 1000.000000000000227 ) ;
#11350 = ORIENTED_EDGE ( 'NONE', *, *, #21055, .T. ) ;
#11351 = ORIENTED_EDGE ( 'NONE', *, *, #10782, .F. ) ;
#11352 = CARTESIAN_POINT ( 'NONE',  ( -25.20278734466900517, 0.000000000000000000, 6.670939612111840944 ) ) ;
#11353 = PLANE ( 'NONE',  #1507 ) ;
#11354 = LINE ( 'NONE', #5694, #46638 ) ;
#11355 = EDGE_CURVE ( 'NONE', #18340, #53438, #2668, .T. ) ;
#11356 = ORIENTED_EDGE ( 'NONE', *, *, #48008, .T. ) ;
#11357 = ORIENTED_EDGE ( 'NONE', *, *, #8176, .F. ) ;
#11358 = ADVANCED_FACE ( 'NONE', ( #19989 ), #7807, .F. ) ;
#11359 = EDGE_CURVE ( 'NONE', #27927, #29027, #3526, .T. ) ;
#11360 = AXIS2_PLACEMENT_3D ( 'NONE', #5280, #43876, #39900 ) ;
#11361 = CARTESIAN_POINT ( 'NONE',  ( -11.15664249260607654, 0.000000000000000000, 4.933589610170957762 ) ) ;
#11362 = LINE ( 'NONE', #6539, #18231 ) ;
#11363 = AXIS2_PLACEMENT_3D ( 'NONE', #25403, #42712, #55788 ) ;
#11364 = ORIENTED_EDGE ( 'NONE', *, *, #23780, .F. ) ;
#11365 = DIRECTION ( 'NONE',  ( 0.005002170337468016433, -0.7660444431189770143, -0.6427681459581293666 ) ) ;
#11366 = ORIENTED_EDGE ( 'NONE', *, *, #1230, .F. ) ;
#11367 = VECTOR ( 'NONE', #10716, 1000.000000000000227 ) ;
#11368 = DIRECTION ( 'NONE',  ( -0.005002170337468016433, -0.7660444431189770143, 0.6427681459581293666 ) ) ;
#11369 = CARTESIAN_POINT ( 'NONE',  ( -18.39746900504187010, 0.000000000000000000, 14.03700784672088808 ) ) ;
#11370 = VERTEX_POINT ( 'NONE', #20836 ) ;
#11371 = PLANE ( 'NONE',  #15914 ) ;
#11372 = VECTOR ( 'NONE', #4356, 1000.000000000000114 ) ;
#11373 = DIRECTION ( 'NONE',  ( -0.7660212471507179544, -0.6427876096865405842, -0.005961354470445141482 ) ) ;
#11374 = AXIS2_PLACEMENT_3D ( 'NONE', #1227, #53230, #14329 ) ;
#11375 = AXIS2_PLACEMENT_3D ( 'NONE', #10931, #50677, #11766 ) ;
#11376 = ORIENTED_EDGE ( 'NONE', *, *, #15292, .F. ) ;
#11377 = DIRECTION ( 'NONE',  ( 0.5000000000000011102, -0.8660254037844380415, 0.000000000000000000 ) ) ;
#11378 = DIRECTION ( 'NONE',  ( 0.007781995580012663651, -3.146120232559066537E-19, -0.9999697198139514409 ) ) ;
#11379 = CARTESIAN_POINT ( 'NONE',  ( -2.207734231944874725, 7.028681301134739989, 4.075932526321295768 ) ) ;
#11380 = VERTEX_POINT ( 'NONE', #38156 ) ;
#11381 = AXIS2_PLACEMENT_3D ( 'NONE', #18100, #13566, #9601 ) ;
#11382 = AXIS2_PLACEMENT_3D ( 'NONE', #6085, #23389, #40705 ) ;
#11383 = CARTESIAN_POINT ( 'NONE',  ( -19.32961685222932147, 0.000000000000000000, 14.39908572644263351 ) ) ;
#11384 = DIRECTION ( 'NONE',  ( 0.9999697198139515519, 0.000000000000000000, 0.007781995580013368816 ) ) ;
#11385 = LINE ( 'NONE', #3129, #25813 ) ;
#11386 = FACE_OUTER_BOUND ( 'NONE', #1516, .T. ) ;
#11387 = EDGE_CURVE ( 'NONE', #34545, #83, #12346, .T. ) ;
#11388 = CARTESIAN_POINT ( 'NONE',  ( -16.09107322271225016, -0.3560938001956550081, 3.516661618153204216 ) ) ;
#11389 = CARTESIAN_POINT ( 'NONE',  ( -17.51878260850159563, 5.143464774974012776, 3.322718381678418709 ) ) ;
#11390 = AXIS2_PLACEMENT_3D ( 'NONE', #21496, #47302, #8409 ) ;
#11391 = AXIS2_PLACEMENT_3D ( 'NONE', #47206, #4064, #51747 ) ;
#11392 = FACE_OUTER_BOUND ( 'NONE', #37119, .T. ) ;
#11393 = EDGE_LOOP ( 'NONE', ( #30968, #14745, #34254, #42848 ) ) ;
#11395 = ADVANCED_FACE ( 'NONE', ( #29929 ), #52058, .F. ) ;
#11394 =( NAMED_UNIT ( * ) SI_UNIT ( $, .STERADIAN. ) SOLID_ANGLE_UNIT ( ) );
#11396 = CARTESIAN_POINT ( 'NONE',  ( -18.67775241435682432, 0.000000000000000000, 4.136394454059623804 ) ) ;
#11397 = CARTESIAN_POINT ( 'NONE',  ( -66.73536025066610478, -1.070822993085610700E-11, -2.844731389951958622 ) ) ;
#11398 = ORIENTED_EDGE ( 'NONE', *, *, #34825, .T. ) ;
#11399 = DIRECTION ( 'NONE',  ( -0.5449076811759708816, 0.6444004775717707689, 0.5364919789714475140 ) ) ;
#11401 = EDGE_CURVE ( 'NONE', #37283, #46770, #51772, .T. ) ;
#11400 = CARTESIAN_POINT ( 'NONE',  ( -20.15755334212245842, 3.848249166794009302, 4.389030706747201194 ) ) ;
#11402 = EDGE_CURVE ( 'NONE', #43237, #36649, #21423, .T. ) ;
#11403 = CARTESIAN_POINT ( 'NONE',  ( -12.68505759159693014, -0.1191753592594172878, 8.145680730609152320 ) ) ;
#11404 = LINE ( 'NONE', #28734, #13322 ) ;
#11405 = DIRECTION ( 'NONE',  ( -0.5364919789714478471, 0.6444004775717705469, -0.5449076811759709926 ) ) ;
#11406 = VECTOR ( 'NONE', #29585, 1000.000000000000000 ) ;
#11407 = ORIENTED_EDGE ( 'NONE', *, *, #20620, .T. ) ;
#11408 = ORIENTED_EDGE ( 'NONE', *, *, #50647, .T. ) ;
#11409 = VECTOR ( 'NONE', #37176, 999.9999999999998863 ) ;
#11410 = CARTESIAN_POINT ( 'NONE',  ( -58.00000000000000711, 2.000000000000000000, -2.999999999999994227 ) ) ;
#11411 = VECTOR ( 'NONE', #35352, 999.9999999999998863 ) ;
#11412 = LINE ( 'NONE', #3450, #17540 ) ;
#11413 = FACE_OUTER_BOUND ( 'NONE', #11843, .T. ) ;
#11414 = ORIENTED_EDGE ( 'NONE', *, *, #40533, .T. ) ;
#11415 = DIRECTION ( 'NONE',  ( 0.9999697198139515519, 0.000000000000000000, 0.007781995580013368816 ) ) ;
#11416 = VECTOR ( 'NONE', #20160, 999.9999999999998863 ) ;
#11417 = ORIENTED_EDGE ( 'NONE', *, *, #54971, .F. ) ;
#11418 = DIRECTION ( 'NONE',  ( 0.007781995580012662783, 0.000000000000000000, -0.9999697198139514409 ) ) ;
#11419 = EDGE_CURVE ( 'NONE', #49166, #3505, #51520, .T. ) ;
#11420 = VECTOR ( 'NONE', #46218, 999.9999999999998863 ) ;
#11421 = VECTOR ( 'NONE', #38466, 1000.000000000000000 ) ;
#11422 = ORIENTED_EDGE ( 'NONE', *, *, #23705, .T. ) ;
#11423 = ORIENTED_EDGE ( 'NONE', *, *, #46266, .F. ) ;
#11424 = DIRECTION ( 'NONE',  ( 0.007781995580012663651, 0.000000000000000000, -0.9999697198139515519 ) ) ;
#11425 = AXIS2_PLACEMENT_3D ( 'NONE', #19192, #1617, #15490 ) ;
#11426 = ADVANCED_FACE ( 'NONE', ( #56060 ), #17711, .T. ) ;
#11427 = CARTESIAN_POINT ( 'NONE',  ( -18.66354898467281132, 0.000000000000000000, 14.21960318569776582 ) ) ;
#11428 = FACE_OUTER_BOUND ( 'NONE', #26675, .T. ) ;
#11429 = VECTOR ( 'NONE', #55522, 999.9999999999998863 ) ;
#11430 = VERTEX_POINT ( 'NONE', #25969 ) ;
#11431 = VECTOR ( 'NONE', #54721, 999.9999999999998863 ) ;
#11432 = CARTESIAN_POINT ( 'NONE',  ( -16.85162240165947978, -0.1191753592594174960, 7.374591420219792859 ) ) ;
#11433 = EDGE_CURVE ( 'NONE', #16969, #42632, #26491, .T. ) ;
#11434 = EDGE_LOOP ( 'NONE', ( #16119, #16902, #24548 ) ) ;
#11435 = ADVANCED_FACE ( 'NONE', ( #52613 ), #4382, .F. ) ;
#11436 = AXIS2_PLACEMENT_3D ( 'NONE', #27013, #21635, #4857 ) ;
#11437 = ORIENTED_EDGE ( 'NONE', *, *, #24733, .F. ) ;
#11438 = VECTOR ( 'NONE', #27460, 999.9999999999998863 ) ;
#11439 = ORIENTED_EDGE ( 'NONE', *, *, #39599, .T. ) ;
#11440 = CARTESIAN_POINT ( 'NONE',  ( 2.072287782118878319, 0.000000000000000000, -2.950529333540147015 ) ) ;
#11441 = CARTESIAN_POINT ( 'NONE',  ( -9.894967649688549471, -0.1191753592594202438, 1.519416599161745429 ) ) ;
#11442 = VERTEX_POINT ( 'NONE', #47230 ) ;
#11443 = CARTESIAN_POINT ( 'NONE',  ( -17.74065527477223725, 3.686347215771509145, 9.822317904363528029 ) ) ;
#11444 = VERTEX_POINT ( 'NONE', #39008 ) ;
#11445 = PLANE ( 'NONE',  #26738 ) ;
#11446 = DIRECTION ( 'NONE',  ( 0.5449076811759707706, 0.6444004775717708799, -0.5364919789714476250 ) ) ;
#11447 = ORIENTED_EDGE ( 'NONE', *, *, #40873, .F. ) ;
#11448 = CARTESIAN_POINT ( 'NONE',  ( -9.835408328977019110, -0.8172783914120439475, 1.672748508373830045 ) ) ;
#11449 = ORIENTED_EDGE ( 'NONE', *, *, #4055, .T. ) ;
#11450 = AXIS2_PLACEMENT_3D ( 'NONE', #16642, #37955, #56121 ) ;
#11451 = EDGE_CURVE ( 'NONE', #2187, #3168, #44112, .T. ) ;
#11452 = DIRECTION ( 'NONE',  ( -0.9999697198139514409, -0.000000000000000000, -0.007781995580013368816 ) ) ;
#11453 = DIRECTION ( 'NONE',  ( 0.7660212471507180654, -0.6427876096865404731, 0.005961354470445141482 ) ) ;
#11454 = LINE ( 'NONE', #45798, #38623 ) ;
#11455 = DIRECTION ( 'NONE',  ( 0.6427681459581294776, -0.7660444431189769032, 0.005002170337467562802 ) ) ;
#11456 = CARTESIAN_POINT ( 'NONE',  ( -19.32961685222932147, 0.000000000000000000, 14.39908572644263351 ) ) ;
#11457 = VECTOR ( 'NONE', #39180, 1000.000000000000227 ) ;
#11458 = ORIENTED_EDGE ( 'NONE', *, *, #45286, .F. ) ;
#11459 = ORIENTED_EDGE ( 'NONE', *, *, #40291, .T. ) ;
#11460 = CARTESIAN_POINT ( 'NONE',  ( 2.072287782118878319, 0.000000000000000000, -2.950529333540147015 ) ) ;
#11461 = VECTOR ( 'NONE', #53341, 1000.000000000000227 ) ;
#11462 = LINE ( 'NONE', #7195, #13080 ) ;
#11463 = CARTESIAN_POINT ( 'NONE',  ( -17.89448523529146229, 0.000000000000000000, 9.113132941433205403 ) ) ;
#11464 = CARTESIAN_POINT ( 'NONE',  ( -21.47263955680318404, 0.000000000000000000, 5.022634149262071190 ) ) ;
#11465 = FACE_OUTER_BOUND ( 'NONE', #11866, .T. ) ;
#11466 = VECTOR ( 'NONE', #34314, 1000.000000000000227 ) ;
#11467 = CARTESIAN_POINT ( 'NONE',  ( -12.15271748404464880, 0.000000000000000000, 1.601849296007406664 ) ) ;
#11468 = ORIENTED_EDGE ( 'NONE', *, *, #49746, .F. ) ;
#11469 = LINE ( 'NONE', #15426, #44922 ) ;
#11470 = CARTESIAN_POINT ( 'NONE',  ( -22.40634380310664397, 0.000000000000000000, 5.584705972946605534 ) ) ;
#11471 = ORIENTED_EDGE ( 'NONE', *, *, #20598, .T. ) ;
#11472 = DIRECTION ( 'NONE',  ( -0.8531650599175529814, -0.4028455766673920135, 0.3313982828793697877 ) ) ;
#11473 = PLANE ( 'NONE',  #44894 ) ;
#11474 = ORIENTED_EDGE ( 'NONE', *, *, #23546, .T. ) ;
#11475 = AXIS2_PLACEMENT_3D ( 'NONE', #6795, #24119, #15863 ) ;
#11476 = CARTESIAN_POINT ( 'NONE',  ( 2.072287782118878319, 0.000000000000000000, -2.950529333540147015 ) ) ;
#11477 = DIRECTION ( 'NONE',  ( -0.9999697198139514409, -0.000000000000000000, -0.007781995580013368816 ) ) ;
#11478 = VECTOR ( 'NONE', #39620, 1000.000000000000227 ) ;
#11479 = ADVANCED_FACE ( 'NONE', ( #369 ), #43812, .F. ) ;
#11480 = DIRECTION ( 'NONE',  ( 0.5449076811759707706, 0.6444004775717708799, -0.5364919789714476250 ) ) ;
#11481 = CARTESIAN_POINT ( 'NONE',  ( -14.23481991729512508, 4.010151117816509903, 2.083274387783130788 ) ) ;
#11482 = AXIS2_PLACEMENT_3D ( 'NONE', #43673, #13587, #17279 ) ;
#11483 = LINE ( 'NONE', #1813, #11074 ) ;
#11484 = ORIENTED_EDGE ( 'NONE', *, *, #29853, .T. ) ;
#11485 = VECTOR ( 'NONE', #12011, 999.9999999999998863 ) ;
#11486 = ORIENTED_EDGE ( 'NONE', *, *, #13925, .T. ) ;
#11487 = CARTESIAN_POINT ( 'NONE',  ( -16.93072279954589732, 0.000000000000000000, 4.688648325876052070 ) ) ;
#11488 = DIRECTION ( 'NONE',  ( -0.7660212471507179544, -0.6427876096865405842, -0.005961354470445141482 ) ) ;
#11489 = LINE ( 'NONE', #16030, #23349 ) ;
#11490 = EDGE_CURVE ( 'NONE', #28225, #51442, #4926, .T. ) ;
#11491 = CARTESIAN_POINT ( 'NONE',  ( -16.93934496006174228, 0.000000000000000000, 5.796577435649344245 ) ) ;
#11492 = CARTESIAN_POINT ( 'NONE',  ( 2.072287782118878319, 0.000000000000000000, -2.950529333540147015 ) ) ;
#11493 = LINE ( 'NONE', #55199, #13143 ) ;
#11495 = EDGE_CURVE ( 'NONE', #54842, #5666, #30208, .T. ) ;
#11494 = ORIENTED_EDGE ( 'NONE', *, *, #27772, .T. ) ;
#11496 = DIRECTION ( 'NONE',  ( -0.6427681459581293666, -0.7660444431189770143, -0.005002170337467561935 ) ) ;
#11497 = ADVANCED_FACE ( 'NONE', ( #13458 ), #26227, .F. ) ;
#11498 = VECTOR ( 'NONE', #32429, 999.9999999999998863 ) ;
#11499 = CARTESIAN_POINT ( 'NONE',  ( -13.59341601676131539, -0.1191753592594177180, 6.661283396080332153 ) ) ;
#11500 = DIRECTION ( 'NONE',  ( 0.000000000000000000, -0.000000000000000000, -1.000000000000000000 ) ) ;
#11501 = ORIENTED_EDGE ( 'NONE', *, *, #37957, .T. ) ;
#11502 = PLANE ( 'NONE',  #32910 ) ;
#11503 = ADVANCED_FACE ( 'NONE', ( #9179 ), #76, .F. ) ;
#11504 = LINE ( 'NONE', #46125, #28619 ) ;
#11505 = CARTESIAN_POINT ( 'NONE',  ( -9.110551994824897193, -1.000000000000000000, 3.538847790438064411 ) ) ;
#11506 = ORIENTED_EDGE ( 'NONE', *, *, #53734, .T. ) ;
#11507 = DIRECTION ( 'NONE',  ( -0.6427681459581293666, -0.7660444431189770143, -0.005002170337467561935 ) ) ;
#11508 = EDGE_CURVE ( 'NONE', #6097, #21737, #21697, .T. ) ;
#11509 = VECTOR ( 'NONE', #56122, 999.9999999999998863 ) ;
#11510 = ORIENTED_EDGE ( 'NONE', *, *, #44814, .F. ) ;
#11511 = EDGE_CURVE ( 'NONE', #1661, #21438, #52359, .T. ) ;
#11512 = ORIENTED_EDGE ( 'NONE', *, *, #289, .F. ) ;
#11513 = VECTOR ( 'NONE', #34256, 999.9999999999998863 ) ;
#11514 = ORIENTED_EDGE ( 'NONE', *, *, #4572, .F. ) ;
#11515 = ORIENTED_EDGE ( 'NONE', *, *, #54741, .T. ) ;
#11516 = ORIENTED_EDGE ( 'NONE', *, *, #32351, .T. ) ;
#11517 = CARTESIAN_POINT ( 'NONE',  ( -14.42191463890408798, 0.000000000000000000, 6.554832800120924396 ) ) ;
#11518 = ORIENTED_EDGE ( 'NONE', *, *, #15624, .F. ) ;
#11519 = EDGE_CURVE ( 'NONE', #33225, #37986, #17992, .T. ) ;
#11520 = VECTOR ( 'NONE', #11722, 1000.000000000000227 ) ;
#11521 = ORIENTED_EDGE ( 'NONE', *, *, #7885, .T. ) ;
#11522 = DIRECTION ( 'NONE',  ( 0.000000000000000000, -1.000000000000000000, 0.000000000000000000 ) ) ;
#11523 = ORIENTED_EDGE ( 'NONE', *, *, #32351, .F. ) ;
#11524 = ORIENTED_EDGE ( 'NONE', *, *, #27785, .F. ) ;
#11525 = EDGE_CURVE ( 'NONE', #8997, #26804, #18540, .T. ) ;
#11526 = AXIS2_PLACEMENT_3D ( 'NONE', #16781, #9095, #4557 ) ;
#11527 = LINE ( 'NONE', #29096, #24732 ) ;
#11528 = LINE ( 'NONE', #19471, #33052 ) ;
#11529 = FACE_OUTER_BOUND ( 'NONE', #4360, .T. ) ;
#11530 = CARTESIAN_POINT ( 'NONE',  ( 1.086233639165236964, -1.000000000000000000, 2.796443541562362078 ) ) ;
#11531 = EDGE_LOOP ( 'NONE', ( #37842, #43601, #9560, #54347 ) ) ;
#11532 = DIRECTION ( 'NONE',  ( 0.000000000000000000, -1.000000000000000000, 0.000000000000000000 ) ) ;
#11533 = EDGE_LOOP ( 'NONE', ( #43609, #43808, #34998, #4129 ) ) ;
#11534 = VERTEX_POINT ( 'NONE', #44644 ) ;
#11535 = CARTESIAN_POINT ( 'NONE',  ( -15.33394411155456716, 0.000000000000000000, 4.331742757038320235 ) ) ;
#11536 = PLANE ( 'NONE',  #1268 ) ;
#11537 = CARTESIAN_POINT ( 'NONE',  ( -29.06878564040112067, 15.87540463137980851, -4.727619564647471684 ) ) ;
#11538 = LINE ( 'NONE', #42471, #26699 ) ;
#11539 = CARTESIAN_POINT ( 'NONE',  ( -14.66887761629205222, 0.000000000000000000, 12.58869632783390990 ) ) ;
#11540 = CARTESIAN_POINT ( 'NONE',  ( -19.79569077582305070, 0.000000000000000000, 14.58012466630350445 ) ) ;
#11541 = EDGE_LOOP ( 'NONE', ( #48361, #25076, #17336, #32794 ) ) ;
#11542 = CARTESIAN_POINT ( 'NONE',  ( -10.00813838035478298, 0.000000000000000000, 10.77830692922518452 ) ) ;
#11543 = ORIENTED_EDGE ( 'NONE', *, *, #16462, .T. ) ;
#11544 = CARTESIAN_POINT ( 'NONE',  ( -20.83449926979080757, -4.889348428825663895, 4.818152362712800674 ) ) ;
#11545 = CARTESIAN_POINT ( 'NONE',  ( -32.65997012216863737, 0.000000000000000000, 9.567562649885804404 ) ) ;
#11547 = CARTESIAN_POINT ( 'NONE',  ( 2.072287782118878319, 0.000000000000000000, -2.950529333540147015 ) ) ;
#11546 = AXIS2_PLACEMENT_3D ( 'NONE', #39589, #43538, #21952 ) ;
#11548 = EDGE_CURVE ( 'NONE', #19068, #4538, #48098, .T. ) ;
#11549 = DIRECTION ( 'NONE',  ( 0.007781995580012662783, 0.000000000000000000, -0.9999697198139514409 ) ) ;
#11550 = CARTESIAN_POINT ( 'NONE',  ( -12.58811780613994813, -1.165603555308156736, 3.484538193242154414 ) ) ;
#11551 = VECTOR ( 'NONE', #25119, 1000.000000000000227 ) ;
#11552 = VERTEX_POINT ( 'NONE', #23086 ) ;
#11553 = EDGE_LOOP ( 'NONE', ( #38970, #22651, #19678, #34289 ) ) ;
#11554 = DIRECTION ( 'NONE',  ( 0.5364919789714477361, 0.6444004775717706579, 0.5449076811759711036 ) ) ;
#11555 = PLANE ( 'NONE',  #20437 ) ;
#11556 = DIRECTION ( 'NONE',  ( 0.007781995580012662783, 0.000000000000000000, -0.9999697198139514409 ) ) ;
#11557 = EDGE_CURVE ( 'NONE', #41770, #37828, #53208, .T. ) ;
#11558 = ADVANCED_FACE ( 'NONE', ( #44380 ), #10305, .F. ) ;
#11559 = VECTOR ( 'NONE', #7533, 999.9999999999998863 ) ;
#11560 = DIRECTION ( 'NONE',  ( -0.5449076811759708816, 0.6444004775717707689, 0.5364919789714475140 ) ) ;
#11561 = CARTESIAN_POINT ( 'NONE',  ( -13.21397773654151209, -4.079838673713161334, 8.510399755611151917 ) ) ;
#11562 = DIRECTION ( 'NONE',  ( 0.005002170337468016433, -0.7660444431189770143, -0.6427681459581293666 ) ) ;
#11563 = DIRECTION ( 'NONE',  ( -0.005961354470445682716, -0.6427876096865404731, 0.7660212471507180654 ) ) ;
#11564 = ADVANCED_FACE ( 'NONE', ( #22796 ), #40694, .F. ) ;
#11565 = DIRECTION ( 'NONE',  ( 0.005961354470445682716, -0.6427876096865404731, -0.7660212471507180654 ) ) ;
#11566 = CARTESIAN_POINT ( 'NONE',  ( -21.93567689722629765, 19.99370688441071309, 4.408989160011352659 ) ) ;
#11567 = EDGE_LOOP ( 'NONE', ( #19833, #42700, #55957, #55557 ) ) ;
#11568 = EDGE_CURVE ( 'NONE', #2911, #38353, #22537, .T. ) ;
#11569 = EDGE_CURVE ( 'NONE', #27005, #31631, #18248, .T. ) ;
#11570 = ORIENTED_EDGE ( 'NONE', *, *, #54005, .F. ) ;
#11571 = ORIENTED_EDGE ( 'NONE', *, *, #47299, .F. ) ;
#11572 = ORIENTED_EDGE ( 'NONE', *, *, #911, .T. ) ;
#11573 = EDGE_CURVE ( 'NONE', #12635, #1853, #31618, .T. ) ;
#11574 = ORIENTED_EDGE ( 'NONE', *, *, #26493, .T. ) ;
#11575 = FACE_OUTER_BOUND ( 'NONE', #8204, .T. ) ;
#11576 = DIRECTION ( 'NONE',  ( -0.000000000000000000, 1.000000000000000000, -0.000000000000000000 ) ) ;
#11577 = CARTESIAN_POINT ( 'NONE',  ( -16.47339040883137784, 0.000000000000000000, 5.630877588122378263 ) ) ;
#11578 = ADVANCED_FACE ( 'NONE', ( #27331 ), #27628, .F. ) ;
#11579 = ORIENTED_EDGE ( 'NONE', *, *, #41656, .F. ) ;
#11580 = ORIENTED_EDGE ( 'NONE', *, *, #27574, .F. ) ;
#11581 = ORIENTED_EDGE ( 'NONE', *, *, #55345, .T. ) ;
#11582 = CARTESIAN_POINT ( 'NONE',  ( -64.81968247311633036, -11.14085154100604669, 2.608662443145389087 ) ) ;
#11583 = EDGE_LOOP ( 'NONE', ( #44535, #35315, #2258, #53291 ) ) ;
#11584 = AXIS2_PLACEMENT_3D ( 'NONE', #36153, #40937, #18530 ) ;
#11585 = CARTESIAN_POINT ( 'NONE',  ( -67.83510688862511984, -9.473535711987191021, 6.778377825370747622 ) ) ;
#11586 = CARTESIAN_POINT ( 'NONE',  ( -16.43317633868556626, -0.1191753592594197858, 13.31363028683540151 ) ) ;
#11587 = DIRECTION ( 'NONE',  ( -0.6427681459581293666, -0.7660444431189770143, -0.005002170337467561935 ) ) ;
#11588 = ORIENTED_EDGE ( 'NONE', *, *, #54124, .T. ) ;
#11589 = LINE ( 'NONE', #46201, #22875 ) ;
#11590 = ORIENTED_EDGE ( 'NONE', *, *, #10546, .T. ) ;
#11591 = AXIS2_PLACEMENT_3D ( 'NONE', #30476, #52584, #22510 ) ;
#11592 = CARTESIAN_POINT ( 'NONE',  ( -17.35095301433918991, -0.1941918491731536578, 3.740333030968461703 ) ) ;
#11593 = DIRECTION ( 'NONE',  ( 0.9999697198139515519, 0.000000000000000000, 0.007781995580013368816 ) ) ;
#11594 = CARTESIAN_POINT ( 'NONE',  ( -11.87243407472968926, 0.000000000000000000, 11.50246268866867361 ) ) ;
#11595 = CARTESIAN_POINT ( 'NONE',  ( -10.94028622754223967, 0.000000000000000000, 11.14038480894692995 ) ) ;
#11596 = DIRECTION ( 'NONE',  ( -0.005961354470445682716, -0.6427876096865404731, 0.7660212471507180654 ) ) ;
#11597 = PLANE ( 'NONE',  #51186 ) ;
#11598 = DIRECTION ( 'NONE',  ( -0.6427681459581293666, -0.7660444431189770143, -0.005002170337467561935 ) ) ;
#11599 = DIRECTION ( 'NONE',  ( -0.2426528472758542054, 0.7422098413412800966, -0.6246952433987894571 ) ) ;
#11600 = EDGE_LOOP ( 'NONE', ( #14120, #38128, #28026, #43928 ) ) ;
#11601 = CARTESIAN_POINT ( 'NONE',  ( -9.542064456761055524, 0.000000000000000000, 10.59726798936431180 ) ) ;
#11602 = ORIENTED_EDGE ( 'NONE', *, *, #1547, .T. ) ;
#11603 = ADVANCED_FACE ( 'NONE', ( #924 ), #53461, .F. ) ;
#11604 = LINE ( 'NONE', #27825, #8393 ) ;
#11605 = PLANE ( 'NONE',  #22390 ) ;
#11606 = FACE_OUTER_BOUND ( 'NONE', #32599, .T. ) ;
#11607 = EDGE_CURVE ( 'NONE', #45422, #39433, #35883, .T. ) ;
#11608 = CARTESIAN_POINT ( 'NONE',  ( -9.075990533167328067, 0.000000000000000000, 10.41622904950343909 ) ) ;
#11609 = DIRECTION ( 'NONE',  ( -0.6427681459581293666, -0.7660444431189770143, -0.005002170337467561935 ) ) ;
#11610 = PLANE ( 'NONE',  #53823 ) ;
#11611 = DIRECTION ( 'NONE',  ( 0.9993050201082468442, 0.03727568626406034535, 1.007958083594035754E-15 ) ) ;
#11612 = VERTEX_POINT ( 'NONE', #17905 ) ;
#11613 = EDGE_CURVE ( 'NONE', #41926, #46588, #26389, .T. ) ;
#11614 = DIRECTION ( 'NONE',  ( 0.7660212471507180654, -0.6427876096865404731, 0.005961354470445141482 ) ) ;
#11615 = CARTESIAN_POINT ( 'NONE',  ( -27.99767448711536133, 0.000000000000000000, 7.557179307314289218 ) ) ;
#11616 = DIRECTION ( 'NONE',  ( 0.007781995580012663651, 0.000000000000000000, -0.9999697198139515519 ) ) ;
#11617 = LINE ( 'NONE', #11327, #5533 ) ;
#11618 = ADVANCED_FACE ( 'NONE', ( #48548 ), #17307, .F. ) ;
#11619 = CARTESIAN_POINT ( 'NONE',  ( -16.81190032086591302, 0.000000000000000000, 3.212244750653343583 ) ) ;
#11620 = EDGE_CURVE ( 'NONE', #12878, #45628, #43703, .T. ) ;
#11621 = ADVANCED_FACE ( 'NONE', ( #35478 ), #4542, .F. ) ;
#11622 = CARTESIAN_POINT ( 'NONE',  ( -13.76180149347061032, 0.1245042932765029059, 2.023510445493768906 ) ) ;
#11623 = LINE ( 'NONE', #28359, #6696 ) ;
#11624 = EDGE_CURVE ( 'NONE', #39606, #27112, #9666, .T. ) ;
#11625 = DIRECTION ( 'NONE',  ( -0.005961354470445682716, -0.6427876096865404731, 0.7660212471507180654 ) ) ;
#11626 = DIRECTION ( 'NONE',  ( -0.9999697198139514409, -0.000000000000000000, -0.007781995580013368816 ) ) ;
#11627 = ORIENTED_EDGE ( 'NONE', *, *, #40754, .T. ) ;
#11628 = FACE_OUTER_BOUND ( 'NONE', #15332, .T. ) ;
#11629 = DIRECTION ( 'NONE',  ( 0.007781995580012662783, 0.000000000000000000, -0.9999697198139514409 ) ) ;
#11630 = ORIENTED_EDGE ( 'NONE', *, *, #1624, .F. ) ;
#11631 = DIRECTION ( 'NONE',  ( -0.9997703818010067467, 0.000000000000000000, -0.02142857142857158143 ) ) ;
#11632 = DIRECTION ( 'NONE',  ( 0.000000000000000000, -1.000000000000000000, 0.000000000000000000 ) ) ;
#11633 = VECTOR ( 'NONE', #1257, 999.9999999999998863 ) ;
#11634 = VERTEX_POINT ( 'NONE', #47416 ) ;
#11635 = ORIENTED_EDGE ( 'NONE', *, *, #50425, .T. ) ;
#11636 = LINE ( 'NONE', #13255, #25690 ) ;
#11637 = ADVANCED_FACE ( 'NONE', ( #44294 ), #12780, .F. ) ;
#11638 = ORIENTED_EDGE ( 'NONE', *, *, #47373, .F. ) ;
#11639 = EDGE_LOOP ( 'NONE', ( #34676, #11072, #8078, #14922 ) ) ;
#11640 = ORIENTED_EDGE ( 'NONE', *, *, #19755, .T. ) ;
#11641 = EDGE_CURVE ( 'NONE', #46009, #46872, #21852, .T. ) ;
#11642 = FACE_OUTER_BOUND ( 'NONE', #1837, .T. ) ;
#11643 = CARTESIAN_POINT ( 'NONE',  ( -65.81867386097172812, -9.242302859876021515, 4.515874129472566167 ) ) ;
#11644 = CARTESIAN_POINT ( 'NONE',  ( -12.52756075508707667, 0.000000000000000000, 1.968264248804815209 ) ) ;
#11645 = EDGE_CURVE ( 'NONE', #41020, #17065, #13367, .T. ) ;
#11646 = ORIENTED_EDGE ( 'NONE', *, *, #43413, .F. ) ;
#11647 = VERTEX_POINT ( 'NONE', #836 ) ;
#11648 = ADVANCED_FACE ( 'NONE', ( #22702 ), #26680, .F. ) ;
#11649 = DIRECTION ( 'NONE',  ( 0.000000000000000000, -1.000000000000000000, 0.000000000000000000 ) ) ;
#11650 = FACE_OUTER_BOUND ( 'NONE', #33457, .T. ) ;
#11651 = ORIENTED_EDGE ( 'NONE', *, *, #27525, .F. ) ;
#11652 = CARTESIAN_POINT ( 'NONE',  ( -19.60990026154428278, 0.000000000000000000, 4.498472333781370125 ) ) ;
#11653 = ORIENTED_EDGE ( 'NONE', *, *, #20539, .T. ) ;
#11654 = DIRECTION ( 'NONE',  ( -0.5449076811759708816, 0.6444004775717707689, 0.5364919789714475140 ) ) ;
#11655 = LINE ( 'NONE', #28969, #3122 ) ;
#11656 = ORIENTED_EDGE ( 'NONE', *, *, #29719, .F. ) ;
#11657 = DIRECTION ( 'NONE',  ( 0.007781995580012663651, 0.000000000000000000, -0.9999697198139515519 ) ) ;
#11658 = LINE ( 'NONE', #28973, #43616 ) ;
#11659 = ORIENTED_EDGE ( 'NONE', *, *, #22192, .T. ) ;
#11660 = PLANE ( 'NONE',  #24024 ) ;
#11661 = FILL_AREA_STYLE ('',( #10570 ) ) ;
#11662 = DIRECTION ( 'NONE',  ( -0.8531650599175529814, -0.4028455766673920135, 0.3313982828793697877 ) ) ;
#11663 = ORIENTED_EDGE ( 'NONE', *, *, #41490, .T. ) ;
#11664 = VECTOR ( 'NONE', #14536, 1000.000000000000227 ) ;
#11665 = CARTESIAN_POINT ( 'NONE',  ( -31.72626587586518099, 0.000000000000000000, 9.005490826201270949 ) ) ;
#11666 = DIRECTION ( 'NONE',  ( 0.005961354470445682716, -0.6427876096865404731, -0.7660212471507180654 ) ) ;
#11667 = LINE ( 'NONE', #32430, #13118 ) ;
#11668 = DIRECTION ( 'NONE',  ( 0.000000000000000000, -0.000000000000000000, -1.000000000000000000 ) ) ;
#11669 = CARTESIAN_POINT ( 'NONE',  ( -9.026147446236871374, 0.000000000000000000, 4.011499419416683310 ) ) ;
#11670 = LINE ( 'NONE', #12523, #37903 ) ;
#11671 = CARTESIAN_POINT ( 'NONE',  ( -67.50471298836741596, -11.44875527771900714, -8.536061506171076729 ) ) ;
#11672 = ORIENTED_EDGE ( 'NONE', *, *, #45827, .F. ) ;
#11673 = DIRECTION ( 'NONE',  ( 0.000000000000000000, -1.000000000000000000, 0.000000000000000000 ) ) ;
#11674 = DIRECTION ( 'NONE',  ( 0.007781995580012662783, 0.000000000000000000, -0.9999697198139514409 ) ) ;
#11675 = CARTESIAN_POINT ( 'NONE',  ( -18.61095121660043361, 0.000000000000000000, 7.460902944687155980 ) ) ;
#11676 = EDGE_LOOP ( 'NONE', ( #52611, #36564, #42857 ) ) ;
#11677 = CARTESIAN_POINT ( 'NONE',  ( -16.40828346936073245, 1.581621852479006440, 5.850566556248715244 ) ) ;
#11678 = CARTESIAN_POINT ( 'NONE',  ( 5.128790131151321319, -6.249319155997272723, 2.187078792930187809 ) ) ;
#11679 = EDGE_CURVE ( 'NONE', #48505, #11768, #17602, .T. ) ;
#11680 = EDGE_CURVE ( 'NONE', #2289, #4025, #22143, .T. ) ;
#11681 = CARTESIAN_POINT ( 'NONE',  ( -17.73140113748535285, 0.000000000000000000, 13.85752530597602039 ) ) ;
#11682 = EDGE_CURVE ( 'NONE', #4466, #42667, #44000, .T. ) ;
#11683 = CARTESIAN_POINT ( 'NONE',  ( -20.36251083028806619, 2.391131607591507446, 8.715066169111624461 ) ) ;
#11684 = DIRECTION ( 'NONE',  ( 0.005002170337468016433, -0.7660444431189770143, -0.6427681459581293666 ) ) ;
#11685 = VERTEX_POINT ( 'NONE', #52786 ) ;
#11686 = ORIENTED_EDGE ( 'NONE', *, *, #8906, .F. ) ;
#11687 = CARTESIAN_POINT ( 'NONE',  ( -27.06708303904391144, 0.000000000000000000, 7.395095371555332697 ) ) ;
#11688 = DIRECTION ( 'NONE',  ( -0.005002170337468016433, -0.7660444431189770143, 0.6427681459581293666 ) ) ;
#11689 = ORIENTED_EDGE ( 'NONE', *, *, #26993, .T. ) ;
#11690 = LINE ( 'NONE', #12252, #33130 ) ;
#11691 = ORIENTED_EDGE ( 'NONE', *, *, #50385, .F. ) ;
#11692 = CARTESIAN_POINT ( 'NONE',  ( -14.24822155599092888, -3.108426967578160394, 7.317883074450481473 ) ) ;
#11693 = ORIENTED_EDGE ( 'NONE', *, *, #18834, .F. ) ;
#11694 = ORIENTED_EDGE ( 'NONE', *, *, #7228, .F. ) ;
#11695 = ORIENTED_EDGE ( 'NONE', *, *, #3269, .T. ) ;
#11696 = DIRECTION ( 'NONE',  ( 0.7660212471507180654, -0.6427876096865404731, 0.005961354470445141482 ) ) ;
#11697 = DIRECTION ( 'NONE',  ( 0.9999697198139515519, 0.000000000000000000, 0.007781995580013368816 ) ) ;
#11698 = DIRECTION ( 'NONE',  ( 0.005002170337468016433, -0.7660444431189770143, -0.6427681459581293666 ) ) ;
#11699 = VERTEX_POINT ( 'NONE', #43187 ) ;
#11700 =( GEOMETRIC_REPRESENTATION_CONTEXT ( 3 ) GLOBAL_UNCERTAINTY_ASSIGNED_CONTEXT ( ( #15487 ) ) GLOBAL_UNIT_ASSIGNED_CONTEXT ( ( #40020, #53103, #22454 ) ) REPRESENTATION_CONTEXT ( 'NONE', 'WORKASPACE' ) );
#11701 = PLANE ( 'NONE',  #20175 ) ;
#11702 = ORIENTED_EDGE ( 'NONE', *, *, #20276, .F. ) ;
#11703 = EDGE_CURVE ( 'NONE', #28441, #7819, #51948, .T. ) ;
#11704 = VERTEX_POINT ( 'NONE', #39474 ) ;
#11705 = ORIENTED_EDGE ( 'NONE', *, *, #8788, .F. ) ;
#11706 = CARTESIAN_POINT ( 'NONE',  ( -21.47263955680318404, 0.000000000000000000, 5.022634149262071190 ) ) ;
#11707 = EDGE_CURVE ( 'NONE', #12718, #8024, #56218, .T. ) ;
#11708 = FACE_OUTER_BOUND ( 'NONE', #46194, .T. ) ;
#11709 = ORIENTED_EDGE ( 'NONE', *, *, #37964, .F. ) ;
#11710 = DIRECTION ( 'NONE',  ( -0.005961354470445682716, -0.6427876096865404731, 0.7660212471507180654 ) ) ;
#11711 = ORIENTED_EDGE ( 'NONE', *, *, #241, .T. ) ;
#11712 = LINE ( 'NONE', #15673, #32230 ) ;
#11713 = CARTESIAN_POINT ( 'NONE',  ( 0.000000000000000000, 2.000000000000000000, 0.000000000000000000 ) ) ;
#11714 = ORIENTED_EDGE ( 'NONE', *, *, #12741, .F. ) ;
#11715 = EDGE_CURVE ( 'NONE', #2289, #19074, #34371, .T. ) ;
#11716 = CARTESIAN_POINT ( 'NONE',  ( -9.808144436391993182, 0.000000000000000000, 10.77986332834118777 ) ) ;
#11717 = ORIENTED_EDGE ( 'NONE', *, *, #37989, .F. ) ;
#11718 = DIRECTION ( 'NONE',  ( -0.8531650599175527594, 0.4028455766673922356, 0.3313982828793700652 ) ) ;
#11719 = DIRECTION ( 'NONE',  ( 0.5449076811759707706, 0.6444004775717708799, -0.5364919789714476250 ) ) ;
#11720 = DIRECTION ( 'NONE',  ( 0.000000000000000000, -1.000000000000000000, 0.000000000000000000 ) ) ;
#11721 = PLANE ( 'NONE',  #20250 ) ;
#11722 = DIRECTION ( 'NONE',  ( -0.5449076811759708816, 0.6444004775717707689, 0.5364919789714475140 ) ) ;
#11723 = CARTESIAN_POINT ( 'NONE',  ( -16.53317331066696383, 0.000000000000000000, 13.31285208727739899 ) ) ;
#11724 = VERTEX_POINT ( 'NONE', #5124 ) ;
#11725 = ORIENTED_EDGE ( 'NONE', *, *, #36419, .T. ) ;
#11726 = FACE_OUTER_BOUND ( 'NONE', #28457, .T. ) ;
#11727 = CARTESIAN_POINT ( 'NONE',  ( -67.59754387994223634, -9.446293363096273765, 7.461800464507162722 ) ) ;
#11728 = CARTESIAN_POINT ( 'NONE',  ( -68.69403907479946270, 0.1329702639046175805, 5.527125342194959323 ) ) ;
#11729 = CARTESIAN_POINT ( 'NONE',  ( 3.882677180727608590, -1.000000000000000000, 1.710209902397122672 ) ) ;
#11730 = CARTESIAN_POINT ( 'NONE',  ( -25.20123094555300369, 0.000000000000000000, 6.470945668149052032 ) ) ;
#11731 = DIRECTION ( 'NONE',  ( 0.005002170337468016433, -0.7660444431189770143, -0.6427681459581293666 ) ) ;
#11732 = ORIENTED_EDGE ( 'NONE', *, *, #5946, .T. ) ;
#11733 = LINE ( 'NONE', #54590, #36784 ) ;
#11734 = DIRECTION ( 'NONE',  ( 0.007781995580012662783, 0.000000000000000000, -0.9999697198139514409 ) ) ;
#11735 = ORIENTED_EDGE ( 'NONE', *, *, #45155, .T. ) ;
#11736 = DIRECTION ( 'NONE',  ( -0.7660212471507179544, -0.6427876096865405842, -0.005961354470445141482 ) ) ;
#11737 = EDGE_CURVE ( 'NONE', #5309, #18585, #34630, .T. ) ;
#11738 = CARTESIAN_POINT ( 'NONE',  ( -19.69569380384165669, -0.1191753592594177458, 14.58090286586150697 ) ) ;
#11739 = ORIENTED_EDGE ( 'NONE', *, *, #9612, .F. ) ;
#11740 = EDGE_CURVE ( 'NONE', #5490, #2403, #6239, .T. ) ;
#11741 = CARTESIAN_POINT ( 'NONE',  ( -70.97773365363613607, 1.999999999999998224, -8.809708619959527809 ) ) ;
#11742 = DIRECTION ( 'NONE',  ( 0.9999697198139515519, 0.000000000000000000, 0.007781995580013368816 ) ) ;
#11743 = DIRECTION ( 'NONE',  ( 0.007781995580012663651, 0.000000000000000000, -0.9999697198139515519 ) ) ;
#11744 = EDGE_CURVE ( 'NONE', #41657, #37529, #14211, .T. ) ;
#11745 = ADVANCED_FACE ( 'NONE', ( #44549 ), #14471, .F. ) ;
#11746 = PLANE ( 'NONE',  #47768 ) ;
#11747 = DIRECTION ( 'NONE',  ( 0.007781995580012663651, 0.000000000000000000, -0.9999697198139515519 ) ) ;
#11748 = ORIENTED_EDGE ( 'NONE', *, *, #40363, .T. ) ;
#11749 = EDGE_LOOP ( 'NONE', ( #38603, #35732, #42157 ) ) ;
#11750 = DIRECTION ( 'NONE',  ( 0.6427681459581294776, -0.7660444431189769032, 0.005002170337467562802 ) ) ;
#11751 = DIRECTION ( 'NONE',  ( -0.005002170337468016433, -0.7660444431189770143, 0.6427681459581293666 ) ) ;
#11752 = DIRECTION ( 'NONE',  ( 0.8660254037844380415, 0.5000000000000011102, 0.000000000000000000 ) ) ;
#11753 = CARTESIAN_POINT ( 'NONE',  ( -18.73788634529089236, 2.714935509636508204, 3.873742472295404138 ) ) ;
#11754 = DIRECTION ( 'NONE',  ( 0.005961354470445682716, -0.6427876096865404731, -0.7660212471507180654 ) ) ;
#11755 = CARTESIAN_POINT ( 'NONE',  ( -20.18150129800645587, 0.9810866208979801550, 5.686756014922062619 ) ) ;
#11756 = EDGE_LOOP ( 'NONE', ( #14848, #47819, #11581, #14853 ) ) ;
#11757 = DIRECTION ( 'NONE',  ( -0.6427681459581293666, -0.7660444431189770143, -0.005002170337467561935 ) ) ;
#11758 = EDGE_CURVE ( 'NONE', #10857, #20993, #5656, .T. ) ;
#11759 = DIRECTION ( 'NONE',  ( 0.000000000000000000, -1.000000000000000000, 0.000000000000000000 ) ) ;
#11760 = FACE_OUTER_BOUND ( 'NONE', #53063, .T. ) ;
#11761 = VERTEX_POINT ( 'NONE', #48836 ) ;
#11762 = CARTESIAN_POINT ( 'NONE',  ( -46.55906441860520317, 5.863990010960497656, -5.000000000000000000 ) ) ;
#11763 = LINE ( 'NONE', #16578, #40427 ) ;
#11764 = DIRECTION ( 'NONE',  ( -0.9999697198139514409, -0.000000000000000000, -0.007781995580013368816 ) ) ;
#11765 = VERTEX_POINT ( 'NONE', #10771 ) ;
#11766 = DIRECTION ( 'NONE',  ( -0.005002170337468016433, -0.7660444431189770143, 0.6427681459581293666 ) ) ;
#11767 = ORIENTED_EDGE ( 'NONE', *, *, #36755, .T. ) ;
#11768 = VERTEX_POINT ( 'NONE', #53915 ) ;
#11769 = ORIENTED_EDGE ( 'NONE', *, *, #38711, .F. ) ;
#11770 = VERTEX_POINT ( 'NONE', #1936 ) ;
#11771 = CARTESIAN_POINT ( 'NONE',  ( -17.21835818046645628, 0.000000000000000000, 7.641066439286161582 ) ) ;
#11772 = VERTEX_POINT ( 'NONE', #44842 ) ;
#11773 = ORIENTED_EDGE ( 'NONE', *, *, #35962, .T. ) ;
#11774 = DIRECTION ( 'NONE',  ( 0.9999697198139515519, 0.000000000000000000, 0.007781995580013368816 ) ) ;
#11775 = ADVANCED_FACE ( 'NONE', ( #36072 ), #19566, .F. ) ;
#11776 = VERTEX_POINT ( 'NONE', #5960 ) ;
#11777 = ORIENTED_EDGE ( 'NONE', *, *, #41228, .T. ) ;
#11778 = DIRECTION ( 'NONE',  ( 0.9999697198139515519, 0.000000000000000000, 0.007781995580013368816 ) ) ;
#11779 = DIRECTION ( 'NONE',  ( 0.9321478471874541372, 0.000000000000000000, -0.3620778797217453771 ) ) ;
#11780 = DIRECTION ( 'NONE',  ( -0.5364919789714478471, 0.6444004775717705469, -0.5449076811759709926 ) ) ;
#11781 = DIRECTION ( 'NONE',  ( -0.5364919789714478471, 0.6444004775717705469, -0.5449076811759709926 ) ) ;
#11782 = PLANE ( 'NONE',  #20174 ) ;
#11783 = ORIENTED_EDGE ( 'NONE', *, *, #33265, .F. ) ;
#11784 = ADVANCED_FACE ( 'NONE', ( #18743 ), #41139, .F. ) ;
#11785 = EDGE_LOOP ( 'NONE', ( #7881, #11797, #10697, #27531 ) ) ;
#11786 = CARTESIAN_POINT ( 'NONE',  ( -26.03813301551774728, 17.43270265044663603, 4.490773887887535842 ) ) ;
#11787 = CARTESIAN_POINT ( 'NONE',  ( -16.72653714768854627, 0.000000000000000000, 4.151579262439313744 ) ) ;
#11788 = EDGE_CURVE ( 'NONE', #13281, #22170, #32367, .T. ) ;
#11789 = EDGE_CURVE ( 'NONE', #23263, #3650, #27521, .T. ) ;
#11790 = DIRECTION ( 'NONE',  ( 0.9999697198139515519, 0.000000000000000000, 0.007781995580013368816 ) ) ;
#11791 = CARTESIAN_POINT ( 'NONE',  ( -17.73140113748535285, 0.000000000000000000, 13.85752530597602039 ) ) ;
#11792 = FACE_OUTER_BOUND ( 'NONE', #48879, .T. ) ;
#11793 = CARTESIAN_POINT ( 'NONE',  ( -16.83811138606217739, 0.4483081953215036219, 4.157565528459807425 ) ) ;
#11794 = ORIENTED_EDGE ( 'NONE', *, *, #5289, .F. ) ;
#11795 = DIRECTION ( 'NONE',  ( -0.3620778797217457656, 0.000000000000000000, -0.9321478471874539151 ) ) ;
#11796 = ADVANCED_FACE ( 'NONE', ( #54207 ), #36905, .F. ) ;
#11797 = ORIENTED_EDGE ( 'NONE', *, *, #38784, .F. ) ;
#11798 = LINE ( 'NONE', #1939, #21613 ) ;
#11799 = FACE_OUTER_BOUND ( 'NONE', #45848, .T. ) ;
#11800 = DIRECTION ( 'NONE',  ( 0.007781995580012663651, -3.146120232559066537E-19, -0.9999697198139514409 ) ) ;
#11801 = EDGE_CURVE ( 'NONE', #32796, #31826, #23807, .T. ) ;
#11802 = CARTESIAN_POINT ( 'NONE',  ( -3.789478469635834568, -7.588859415764141580, -1.746411446826717340 ) ) ;
#11803 = CARTESIAN_POINT ( 'NONE',  ( -12.13851405436063047, 0.000000000000000000, 11.68505802764555135 ) ) ;
#11804 = EDGE_CURVE ( 'NONE', #46401, #45947, #32615, .T. ) ;
#11805 = LINE ( 'NONE', #28870, #35952 ) ;
#11806 = AXIS2_PLACEMENT_3D ( 'NONE', #14676, #27761, #49618 ) ;
#11807 = VERTEX_POINT ( 'NONE', #9936 ) ;
#11808 = ORIENTED_EDGE ( 'NONE', *, *, #54700, .T. ) ;
#11809 = DIRECTION ( 'NONE',  ( -0.005002170337468016433, -0.7660444431189770143, 0.6427681459581293666 ) ) ;
#11810 = LINE ( 'NONE', #33135, #50354 ) ;
#11811 = LINE ( 'NONE', #46746, #41498 ) ;
#11812 = ADVANCED_FACE ( 'NONE', ( #10502 ), #28344, .F. ) ;
#11813 = CARTESIAN_POINT ( 'NONE',  ( -10.00813838035478298, 0.000000000000000000, 10.77830692922518452 ) ) ;
#11814 = CARTESIAN_POINT ( 'NONE',  ( -28.93137873341882127, 0.000000000000000000, 8.119251130998824451 ) ) ;
#11815 = LINE ( 'NONE', #26033, #7406 ) ;
#11816 = CARTESIAN_POINT ( 'NONE',  ( -14.33979583046189887, 3.524445264749008988, 8.235599918570057909 ) ) ;
#11817 = ADVANCED_FACE ( 'NONE', ( #53631 ), #40013, .F. ) ;
#11818 = CARTESIAN_POINT ( 'NONE',  ( -16.53317331066696383, 0.000000000000000000, 13.31285208727739899 ) ) ;
#11819 = B_SPLINE_CURVE_WITH_KNOTS ( 'NONE', 3,
 ( #4701, #34519, #43346, #3851 ),
 .UNSPECIFIED., .F., .F.,
 ( 4, 4 ),
 ( 0.0002388585478777321643, 0.0002669665482816597568 ),
 .UNSPECIFIED. ) ;
#11820 = LINE ( 'NONE', #7034, #52806 ) ;
#11821 = ORIENTED_EDGE ( 'NONE', *, *, #28999, .T. ) ;
#11822 = PLANE ( 'NONE',  #34061 ) ;
#11823 = EDGE_LOOP ( 'NONE', ( #14876, #24990, #19629, #39530 ) ) ;
#11824 = EDGE_LOOP ( 'NONE', ( #55214, #45054, #13858, #45079 ) ) ;
#11825 = ORIENTED_EDGE ( 'NONE', *, *, #17117, .T. ) ;
#11826 = VERTEX_POINT ( 'NONE', #32069 ) ;
#11827 = EDGE_LOOP ( 'NONE', ( #7233, #29383, #37162, #13745 ) ) ;
#11828 = DIRECTION ( 'NONE',  ( -0.005002170337468016433, -0.7660444431189770143, 0.6427681459581293666 ) ) ;
#11829 = LINE ( 'NONE', #38233, #47432 ) ;
#11830 = CARTESIAN_POINT ( 'NONE',  ( -24.27063949748155380, 0.000000000000000000, 6.308861732390097288 ) ) ;
#11831 = ORIENTED_EDGE ( 'NONE', *, *, #8568, .T. ) ;
#11832 = CARTESIAN_POINT ( 'NONE',  ( -22.40634380310664397, 0.000000000000000000, 5.584705972946605534 ) ) ;
#11833 = ADVANCED_FACE ( 'NONE', ( #18437 ), #35771, .F. ) ;
#11834 = VERTEX_POINT ( 'NONE', #51042 ) ;
#11835 = CARTESIAN_POINT ( 'NONE',  ( 2.072287782118878319, 0.000000000000000000, -2.950529333540147015 ) ) ;
#11836 = VERTEX_POINT ( 'NONE', #7613 ) ;
#11837 = VECTOR ( 'NONE', #32442, 1000.000000000000000 ) ;
#11838 = CARTESIAN_POINT ( 'NONE',  ( -67.65173211775538675, -9.452507356115830817, 6.473804834638488437 ) ) ;
#11839 = DIRECTION ( 'NONE',  ( -0.005961354470445682716, -0.6427876096865404731, 0.7660212471507180654 ) ) ;
#11840 = DIRECTION ( 'NONE',  ( 0.9999697198139515519, 0.000000000000000000, 0.007781995580013368816 ) ) ;
#11841 = ORIENTED_EDGE ( 'NONE', *, *, #29944, .F. ) ;
#11842 = DIRECTION ( 'NONE',  ( 0.9999697198139515519, 0.000000000000000000, 0.007781995580013368816 ) ) ;
#11843 = EDGE_LOOP ( 'NONE', ( #8009, #30158, #38851 ) ) ;
#11844 = CARTESIAN_POINT ( 'NONE',  ( -21.47263955680318404, 0.000000000000000000, 5.022634149262071190 ) ) ;
#11845 = DIRECTION ( 'NONE',  ( 0.007781995580012663651, -3.146120232559066537E-19, -0.9999697198139514409 ) ) ;
#11846 = EDGE_CURVE ( 'NONE', #20292, #55275, #37732, .T. ) ;
#11847 = CARTESIAN_POINT ( 'NONE',  ( -12.05517860703720778, 1.419719901456504507, 1.319276000146733185 ) ) ;
#11848 = CARTESIAN_POINT ( 'NONE',  ( -19.60990026154428278, 0.000000000000000000, 4.498472333781370125 ) ) ;
#11849 = FACE_OUTER_BOUND ( 'NONE', #20354, .T. ) ;
#11850 = DIRECTION ( 'NONE',  ( 0.005961354470445682716, -0.6427876096865404731, -0.7660212471507180654 ) ) ;
#11851 = CARTESIAN_POINT ( 'NONE',  ( -18.67697421479882181, -0.1191753592594197858, 4.036397482078229793 ) ) ;
#11852 = CARTESIAN_POINT ( 'NONE',  ( -28.93137873341882127, 0.000000000000000000, 8.119251130998824451 ) ) ;
#11853 = EDGE_LOOP ( 'NONE', ( #47170, #12003, #37517, #25099 ) ) ;
#11854 = DIRECTION ( 'NONE',  ( -0.6427681459581293666, -0.7660444431189770143, -0.005002170337467561935 ) ) ;
#11855 = ORIENTED_EDGE ( 'NONE', *, *, #52598, .F. ) ;
#11856 = VECTOR ( 'NONE', #49880, 1000.000000000000227 ) ;
#11857 = DIRECTION ( 'NONE',  ( 0.007781995580012662783, 0.000000000000000000, -0.9999697198139514409 ) ) ;
#11858 = LINE ( 'NONE', #38564, #9696 ) ;
#11859 = ADVANCED_FACE ( 'NONE', ( #55055 ), #16144, .F. ) ;
#11860 = DIRECTION ( 'NONE',  ( -0.5449076811759708816, 0.6444004775717707689, 0.5364919789714475140 ) ) ;
#11861 = CARTESIAN_POINT ( 'NONE',  ( -25.20200914511100265, -0.1191753592594197858, 6.570942640130446932 ) ) ;
#11862 = LINE ( 'NONE', #47081, #16824 ) ;
#11863 = EDGE_CURVE ( 'NONE', #54767, #24397, #15850, .T. ) ;
#11864 = DIRECTION ( 'NONE',  ( 0.000000000000000000, -1.000000000000000000, 0.000000000000000000 ) ) ;
#11865 = SURFACE_STYLE_USAGE ( .BOTH. , #32620 ) ;
#11866 = EDGE_LOOP ( 'NONE', ( #20002, #18329, #29030, #20905 ) ) ;
#11867 = DIRECTION ( 'NONE',  ( 0.6246952433987894571, -0.7422098413412800966, -0.2426528472758541777 ) ) ;
#11868 = CARTESIAN_POINT ( 'NONE',  ( -9.391748698554145847, 7.045229895792196828, 0.4297005639829583057 ) ) ;
#11869 = LINE ( 'NONE', #12729, #6787 ) ;
#11870 = DIRECTION ( 'NONE',  ( -0.5449076811759708816, 0.6444004775717707689, 0.5364919789714475140 ) ) ;
#11871 = ADVANCED_FACE ( 'NONE', ( #7079 ), #28648, .F. ) ;
#11872 = VECTOR ( 'NONE', #16192, 999.9999999999998863 ) ;
#11873 = LINE ( 'NONE', #54468, #48179 ) ;
#11874 = DIRECTION ( 'NONE',  ( -0.005961354470445682716, -0.6427876096865404731, 0.7660212471507180654 ) ) ;
#11875 = FACE_OUTER_BOUND ( 'NONE', #40128, .T. ) ;
#11876 = FACE_OUTER_BOUND ( 'NONE', #34332, .T. ) ;
#11877 = ORIENTED_EDGE ( 'NONE', *, *, #26754, .F. ) ;
#11878 = AXIS2_PLACEMENT_3D ( 'NONE', #18107, #26340, #30341 ) ;
#11879 = EDGE_CURVE ( 'NONE', #8877, #2394, #41435, .T. ) ;
#11880 = DIRECTION ( 'NONE',  ( 0.6246952433987893460, 0.7422098413412802076, -0.2426528472758539279 ) ) ;
#11881 = DIRECTION ( 'NONE',  ( -0.005961354470445682716, -0.6427876096865404731, 0.7660212471507180654 ) ) ;
#11882 = ORIENTED_EDGE ( 'NONE', *, *, #17125, .T. ) ;
#11883 = ORIENTED_EDGE ( 'NONE', *, *, #8949, .F. ) ;
#11884 = DIRECTION ( 'NONE',  ( -0.1139275668495183524, 0.9934890585767659488, 4.694855797473117491E-16 ) ) ;
#11885 = ORIENTED_EDGE ( 'NONE', *, *, #52086, .F. ) ;
#11886 = ORIENTED_EDGE ( 'NONE', *, *, #44063, .T. ) ;
#11887 = DIRECTION ( 'NONE',  ( -0.5449076811759708816, 0.6444004775717707689, 0.5364919789714475140 ) ) ;
#11888 = ORIENTED_EDGE ( 'NONE', *, *, #54239, .T. ) ;
#11889 = EDGE_LOOP ( 'NONE', ( #6368, #44574, #41343, #2950 ) ) ;
#11890 = ORIENTED_EDGE ( 'NONE', *, *, #21220, .F. ) ;
#11891 = CARTESIAN_POINT ( 'NONE',  ( -17.70179579745524023, 0.000000000000000000, 10.05330269102752716 ) ) ;
#11892 = LINE ( 'NONE', #8211, #22403 ) ;
#11893 = DIRECTION ( 'NONE',  ( 0.5364919789714477361, 0.6444004775717706579, 0.5449076811759711036 ) ) ;
#11894 = EDGE_CURVE ( 'NONE', #29513, #18849, #2517, .T. ) ;
#11895 = VECTOR ( 'NONE', #24652, 1000.000000000000227 ) ;
#11896 = AXIS2_PLACEMENT_3D ( 'NONE', #25479, #42527, #9015 ) ;
#11897 = EDGE_LOOP ( 'NONE', ( #11571, #36923, #30928, #53469 ) ) ;
#11899 = VERTEX_POINT ( 'NONE', #15557 ) ;
#11898 = ADVANCED_FACE ( 'NONE', ( #11606 ), #38005, .F. ) ;
#11900 = ADVANCED_FACE ( 'NONE', ( #24943 ), #32888, .F. ) ;
#11901 = CARTESIAN_POINT ( 'NONE',  ( -11.09739355201212163, -0.5179957512181557755, 1.175398865385032465 ) ) ;
#11902 = FACE_OUTER_BOUND ( 'NONE', #53032, .T. ) ;
#11904 = ADVANCED_FACE ( 'NONE', ( #19837 ), #33725, .F. ) ;
#11903 = ORIENTED_EDGE ( 'NONE', *, *, #28371, .T. ) ;
#11905 = DIRECTION ( 'NONE',  ( 0.9999697198139515519, 0.000000000000000000, 0.007781995580013368816 ) ) ;
#11906 = ORIENTED_EDGE ( 'NONE', *, *, #29677, .T. ) ;
#11907 = CARTESIAN_POINT ( 'NONE',  ( -11.20636620717317378, 0.000000000000000000, 11.32298014792380414 ) ) ;
#11908 = CARTESIAN_POINT ( 'NONE',  ( -26.25138199253913385, 17.50203338588876179, 4.621929860192643069 ) ) ;
#11909 = EDGE_CURVE ( 'NONE', #4790, #18162, #37421, .T. ) ;
#11910 = EDGE_CURVE ( 'NONE', #54304, #30596, #50207, .T. ) ;
#11911 = EDGE_CURVE ( 'NONE', #19103, #7431, #20690, .T. ) ;
#11912 = ORIENTED_EDGE ( 'NONE', *, *, #34594, .T. ) ;
#11913 = DIRECTION ( 'NONE',  ( 0.005961354470445682716, -0.6427876096865404731, -0.7660212471507180654 ) ) ;
#11914 = AXIS2_PLACEMENT_3D ( 'NONE', #1452, #23329, #5174 ) ;
#11915 = PLANE ( 'NONE',  #12776 ) ;
#11916 = ORIENTED_EDGE ( 'NONE', *, *, #6079, .T. ) ;
#11917 = CARTESIAN_POINT ( 'NONE',  ( -21.31610270512911143, 5.143464774974011888, 13.60252126457413624 ) ) ;
#11918 = PLANE ( 'NONE',  #7610 ) ;
#11919 = DIRECTION ( 'NONE',  ( -0.9999697198139514409, -0.000000000000000000, -0.007781995580013368816 ) ) ;
#11920 = EDGE_LOOP ( 'NONE', ( #4020, #51555, #11948, #41936 ) ) ;
#11921 = FACE_OUTER_BOUND ( 'NONE', #16799, .T. ) ;
#11922 = CARTESIAN_POINT ( 'NONE',  ( -3.184385661761863773, -6.114012816731704270, -1.981450042443219539 ) ) ;
#11923 = CARTESIAN_POINT ( 'NONE',  ( -10.68182703613314644, 0.000000000000000000, 3.629282468202884804 ) ) ;
#11924 = EDGE_CURVE ( 'NONE', #43321, #30466, #29486, .T. ) ;
#11925 = DIRECTION ( 'NONE',  ( 0.5449076811759707706, 0.6444004775717708799, -0.5364919789714476250 ) ) ;
#11926 = DIRECTION ( 'NONE',  ( -0.005002170337468016433, -0.7660444431189770143, 0.6427681459581293666 ) ) ;
#11927 = PLANE ( 'NONE',  #22504 ) ;
#11928 = EDGE_CURVE ( 'NONE', #5052, #33685, #7924, .T. ) ;
#11929 = LINE ( 'NONE', #50278, #26739 ) ;
#11930 = ORIENTED_EDGE ( 'NONE', *, *, #30971, .T. ) ;
#11931 = PLANE ( 'NONE',  #47088 ) ;
#11932 = EDGE_CURVE ( 'NONE', #15628, #23911, #3633, .T. ) ;
#11933 = CARTESIAN_POINT ( 'NONE',  ( -66.92698279747418155, 1.734723475976807094E-15, 5.887047890942916695 ) ) ;
#11934 = ORIENTED_EDGE ( 'NONE', *, *, #50033, .F. ) ;
#11935 = FACE_OUTER_BOUND ( 'NONE', #13631, .T. ) ;
#11936 = DIRECTION ( 'NONE',  ( 0.000000000000000000, -1.000000000000000000, 0.000000000000000000 ) ) ;
#11937 = VECTOR ( 'NONE', #41311, 1000.000000000000000 ) ;
#11938 = EDGE_CURVE ( 'NONE', #51942, #3988, #3061, .T. ) ;
#11939 = AXIS2_PLACEMENT_3D ( 'NONE', #32201, #14591, #6104 ) ;
#11940 = DIRECTION ( 'NONE',  ( -0.7660212471507179544, -0.6427876096865405842, -0.005961354470445141482 ) ) ;
#11941 = CARTESIAN_POINT ( 'NONE',  ( -11.23861694399777633, -0.1191753592594189115, 2.616956219084973334 ) ) ;
#11942 = LINE ( 'NONE', #17073, #55590 ) ;
#11943 = ORIENTED_EDGE ( 'NONE', *, *, #51679, .F. ) ;
#11944 = AXIS2_PLACEMENT_3D ( 'NONE', #19402, #14879, #36743 ) ;
#11945 = ORIENTED_EDGE ( 'NONE', *, *, #24663, .F. ) ;
#11946 = CARTESIAN_POINT ( 'NONE',  ( -10.74029228357944987, 0.000000000000000000, 11.14194120806293320 ) ) ;
#11947 = PLANE ( 'NONE',  #4849 ) ;
#11948 = ORIENTED_EDGE ( 'NONE', *, *, #48040, .T. ) ;
#11949 = LINE ( 'NONE', #3161, #39498 ) ;
#11950 = VECTOR ( 'NONE', #21781, 1000.000000000000114 ) ;
#11951 = ORIENTED_EDGE ( 'NONE', *, *, #41587, .T. ) ;
#11952 = PLANE ( 'NONE',  #37429 ) ;
#11953 = VECTOR ( 'NONE', #45118, 1000.000000000000227 ) ;
#11954 = EDGE_LOOP ( 'NONE', ( #17493, #14990, #9405, #26622 ) ) ;
#11955 = ORIENTED_EDGE ( 'NONE', *, *, #24551, .T. ) ;
#11956 = ORIENTED_EDGE ( 'NONE', *, *, #32420, .T. ) ;
#11957 = CARTESIAN_POINT ( 'NONE',  ( -9.342070512798265725, 0.000000000000000000, 10.59882438848031505 ) ) ;
#11958 = CARTESIAN_POINT ( 'NONE',  ( 2.072287782118878319, 0.000000000000000000, -2.950529333540147015 ) ) ;
#11959 = LINE ( 'NONE', #51153, #18512 ) ;
#11960 = LINE ( 'NONE', #29608, #30306 ) ;
#11961 = EDGE_LOOP ( 'NONE', ( #48692, #16461, #27139, #42486 ) ) ;
#11962 = EDGE_LOOP ( 'NONE', ( #6899, #12890, #36401, #46262 ) ) ;
#11963 = EDGE_LOOP ( 'NONE', ( #17016, #38725, #51683, #36362 ) ) ;
#11964 = DIRECTION ( 'NONE',  ( -0.7660212471507179544, -0.6427876096865405842, -0.005961354470445141482 ) ) ;
#11965 = LINE ( 'NONE', #50870, #22209 ) ;
#11966 = ORIENTED_EDGE ( 'NONE', *, *, #34585, .F. ) ;
#11967 = VECTOR ( 'NONE', #8946, 1000.000000000000227 ) ;
#11968 = CARTESIAN_POINT ( 'NONE',  ( -17.57195112297145556, 2.945294577023091609, 12.40488687576302773 ) ) ;
#11969 = ORIENTED_EDGE ( 'NONE', *, *, #36689, .F. ) ;
#11970 = DIRECTION ( 'NONE',  ( -0.7660212471507179544, -0.6427876096865405842, -0.005961354470445141482 ) ) ;
#11971 = DIRECTION ( 'NONE',  ( 0.007781995580012662783, 0.000000000000000000, -0.9999697198139514409 ) ) ;
#11972 = EDGE_CURVE ( 'NONE', #11534, #5052, #16699, .T. ) ;
#11973 = EDGE_CURVE ( 'NONE', #29528, #38022, #49675, .T. ) ;
#11974 = AXIS2_PLACEMENT_3D ( 'NONE', #38147, #13167, #38741 ) ;
#11975 = VECTOR ( 'NONE', #48236, 1000.000000000000000 ) ;
#11976 = ORIENTED_EDGE ( 'NONE', *, *, #45559, .T. ) ;
#11977 = LINE ( 'NONE', #28469, #21353 ) ;
#11978 = ORIENTED_EDGE ( 'NONE', *, *, #7537, .T. ) ;
#11979 = EDGE_CURVE ( 'NONE', #44660, #46056, #54205, .T. ) ;
#11980 = VECTOR ( 'NONE', #9246, 1000.000000000000000 ) ;
#11981 = CARTESIAN_POINT ( 'NONE',  ( -16.65852666505410795, 1.905425754524007642, 3.091876156576410128 ) ) ;
#11982 = CARTESIAN_POINT ( 'NONE',  ( -56.75000000000000711, -9.000000000000000000, -2.449489742783172108 ) ) ;
#11983 = VECTOR ( 'NONE', #16843, 1000.000000000000227 ) ;
#11984 = VERTEX_POINT ( 'NONE', #15556 ) ;
#11985 = DIRECTION ( 'NONE',  ( 0.000000000000000000, -1.000000000000000000, 0.000000000000000000 ) ) ;
#11986 = CARTESIAN_POINT ( 'NONE',  ( -17.41292333033276307, 3.848249166794008413, 9.960724371270012867 ) ) ;
#11987 = PLANE ( 'NONE',  #2388 ) ;
#11988 = DIRECTION ( 'NONE',  ( 1.007958083594381472E-15, -3.869188571150965146E-16, 1.000000000000000000 ) ) ;
#11989 = ORIENTED_EDGE ( 'NONE', *, *, #42422, .F. ) ;
#11990 = ORIENTED_EDGE ( 'NONE', *, *, #53589, .F. ) ;
#11991 = DIRECTION ( 'NONE',  ( 0.9999697198139515519, 0.000000000000000000, 0.007781995580013368816 ) ) ;
#11992 = CARTESIAN_POINT ( 'NONE',  ( -11.33364400852660658, 0.000000000000000000, 1.977555584992839455 ) ) ;
#11993 = VECTOR ( 'NONE', #54966, 999.9999999999998863 ) ;
#11994 = CARTESIAN_POINT ( 'NONE',  ( -67.39275645683859750, 0.1329239778084786161, -1.367274824955979851 ) ) ;
#11995 = DIRECTION ( 'NONE',  ( 0.9999697198139515519, 0.000000000000000000, 0.007781995580013368816 ) ) ;
#11997 = ADVANCED_FACE ( 'NONE', ( #19265 ), #32067, .F. ) ;
#11996 = DIRECTION ( 'NONE',  ( 0.007781995580012663651, 0.000000000000000000, -0.9999697198139515519 ) ) ;
#11998 = DIRECTION ( 'NONE',  ( -0.5449076811759708816, 0.6444004775717707689, 0.5364919789714475140 ) ) ;
#11999 = EDGE_LOOP ( 'NONE', ( #36793, #295, #47154, #11351 ) ) ;
#12000 = DIRECTION ( 'NONE',  ( -0.7660212471507179544, -0.6427876096865405842, -0.005961354470445141482 ) ) ;
#12001 = EDGE_CURVE ( 'NONE', #2953, #50886, #28343, .T. ) ;
#12002 = DIRECTION ( 'NONE',  ( 0.5364919789714477361, 0.6444004775717706579, 0.5449076811759711036 ) ) ;
#12003 = ORIENTED_EDGE ( 'NONE', *, *, #12741, .T. ) ;
#12004 = DIRECTION ( 'NONE',  ( 0.6427681459581294776, -0.7660444431189769032, 0.005002170337467562802 ) ) ;
#12005 = VERTEX_POINT ( 'NONE', #2515 ) ;
#12006 = FACE_OUTER_BOUND ( 'NONE', #44665, .T. ) ;
#12007 = DIRECTION ( 'NONE',  ( 0.007781995580012663651, 0.000000000000000000, -0.9999697198139515519 ) ) ;
#12008 = ADVANCED_FACE ( 'NONE', ( #18741 ), #14469, .F. ) ;
#12009 = PLANE ( 'NONE',  #45884 ) ;
#12010 = AXIS2_PLACEMENT_3D ( 'NONE', #36912, #37163, #14221 ) ;
#12011 = DIRECTION ( 'NONE',  ( 0.9999697198139515519, 0.000000000000000000, 0.007781995580013368816 ) ) ;
#12012 = CARTESIAN_POINT ( 'NONE',  ( -67.68419632946157094, 1.999999999973934850, -3.410887992491007825 ) ) ;
#12013 = ORIENTED_EDGE ( 'NONE', *, *, #20693, .F. ) ;
#12014 = ORIENTED_EDGE ( 'NONE', *, *, #45332, .T. ) ;
#12015 = CARTESIAN_POINT ( 'NONE',  ( -67.90158791901538393, -0.6013636351494499044, -4.591303796237528267 ) ) ;
#12016 = CARTESIAN_POINT ( 'NONE',  ( 5.515120863165694942, -1.062156740595928683, 2.500028430129012325 ) ) ;
#12017 = AXIS2_PLACEMENT_3D ( 'NONE', #31945, #27702, #6137 ) ;
#12018 = DIRECTION ( 'NONE',  ( 0.2113248654051873565, 0.7886751345948123104, 0.5773502691896265082 ) ) ;
#12019 = EDGE_CURVE ( 'NONE', #54483, #3178, #19564, .T. ) ;
#12020 = VECTOR ( 'NONE', #16418, 999.9999999999998863 ) ;
#12021 = CARTESIAN_POINT ( 'NONE',  ( -9.500962902709808588, 0.000000000000000000, 5.315806561384757600 ) ) ;
#12022 = VECTOR ( 'NONE', #6714, 1000.000000000000227 ) ;
#12023 = DIRECTION ( 'NONE',  ( 0.005961354470445682716, -0.6427876096865404731, -0.7660212471507180654 ) ) ;
#12024 = CARTESIAN_POINT ( 'NONE',  ( 2.072287782118878319, 0.000000000000000000, -2.950529333540147015 ) ) ;
#12025 = ORIENTED_EDGE ( 'NONE', *, *, #8084, .T. ) ;
#12026 = DIRECTION ( 'NONE',  ( 0.000000000000000000, -1.000000000000000000, 0.000000000000000000 ) ) ;
#12027 = DIRECTION ( 'NONE',  ( -0.9999697198139514409, -0.000000000000000000, -0.007781995580013368816 ) ) ;
#12028 = AXIS2_PLACEMENT_3D ( 'NONE', #27924, #35579, #14311 ) ;
#12029 = CARTESIAN_POINT ( 'NONE',  ( -18.72166620304495410, -0.1191753592594162470, 8.837366586178813321 ) ) ;
#12030 = VECTOR ( 'NONE', #16697, 1000.000000000000227 ) ;
#12031 = ORIENTED_EDGE ( 'NONE', *, *, #13023, .T. ) ;
#12032 = LINE ( 'NONE', #50671, #6605 ) ;
#12033 = CARTESIAN_POINT ( 'NONE',  ( -8.351072905600126717, 0.000000000000000000, 5.494081284814476440 ) ) ;
#12034 = PLANE ( 'NONE',  #31163 ) ;
#12035 = ORIENTED_EDGE ( 'NONE', *, *, #11548, .F. ) ;
#12036 = DIRECTION ( 'NONE',  ( 0.005961354470445682716, -0.6427876096865404731, -0.7660212471507180654 ) ) ;
#12037 = VECTOR ( 'NONE', #14198, 1000.000000000000114 ) ;
#12038 = EDGE_LOOP ( 'NONE', ( #21513, #54935, #7587, #49279 ) ) ;
#12039 = VECTOR ( 'NONE', #2611, 1000.000000000000227 ) ;
#12040 = ORIENTED_EDGE ( 'NONE', *, *, #55092, .F. ) ;
#12041 = ORIENTED_EDGE ( 'NONE', *, *, #50497, .F. ) ;
#12042 = ORIENTED_EDGE ( 'NONE', *, *, #18230, .F. ) ;
#12043 = CARTESIAN_POINT ( 'NONE',  ( -12.56624110504503022, 0.000000000000000000, 6.938606150450726595 ) ) ;
#12044 = VERTEX_POINT ( 'NONE', #53374 ) ;
#12045 = VECTOR ( 'NONE', #19181, 1000.000000000000227 ) ;
#12046 = LINE ( 'NONE', #51787, #47623 ) ;
#12047 = EDGE_CURVE ( 'NONE', #31757, #54495, #19836, .T. ) ;
#12048 = ORIENTED_EDGE ( 'NONE', *, *, #29606, .T. ) ;
#12049 = DIRECTION ( 'NONE',  ( 0.5364919789714477361, 0.6444004775717706579, 0.5449076811759711036 ) ) ;
#12050 = ORIENTED_EDGE ( 'NONE', *, *, #49637, .F. ) ;
#12051 = AXIS2_PLACEMENT_3D ( 'NONE', #51690, #25035, #8253 ) ;
#12052 = VERTEX_POINT ( 'NONE', #15303 ) ;
#12053 = EDGE_CURVE ( 'NONE', #42246, #35922, #28647, .T. ) ;
#12054 = EDGE_CURVE ( 'NONE', #41830, #39497, #11022, .T. ) ;
#12055 = CARTESIAN_POINT ( 'NONE',  ( -19.65677579747983472, 21.21320419402555402, 4.265613255886147925 ) ) ;
#12056 = DIRECTION ( 'NONE',  ( -0.7660212471507179544, -0.6427876096865405842, -0.005961354470445141482 ) ) ;
#12057 = DIRECTION ( 'NONE',  ( 0.7660212471507180654, -0.6427876096865404731, 0.005961354470445141482 ) ) ;
#12058 = DIRECTION ( 'NONE',  ( 0.5000000000000011102, -0.8660254037844380415, 0.000000000000000000 ) ) ;
#12059 = VECTOR ( 'NONE', #44949, 1000.000000000000227 ) ;
#12060 = CARTESIAN_POINT ( 'NONE',  ( -9.935302865382064752, 0.000000000000000000, 1.419099673076315016 ) ) ;
#12061 = EDGE_LOOP ( 'NONE', ( #50807, #2614, #21953, #43063 ) ) ;
#12062 = VECTOR ( 'NONE', #48424, 999.9999999999998863 ) ;
#12063 = VECTOR ( 'NONE', #8381, 999.9999999999998863 ) ;
#12064 = VERTEX_POINT ( 'NONE', #15030 ) ;
#12065 = CARTESIAN_POINT ( 'NONE',  ( -8.409922665610809034, 0.000000000000000000, 10.23674650875856962 ) ) ;
#12066 = LINE ( 'NONE', #54660, #40273 ) ;
#12067 = DIRECTION ( 'NONE',  ( 0.007781995580012662783, 0.000000000000000000, -0.9999697198139514409 ) ) ;
#12068 = VECTOR ( 'NONE', #44879, 1000.000000000000227 ) ;
#12069 = VECTOR ( 'NONE', #16477, 1000.000000000000227 ) ;
#12070 = CARTESIAN_POINT ( 'NONE',  ( -17.46532115785441519, 0.000000000000000000, 13.67492996699914265 ) ) ;
#12071 = DIRECTION ( 'NONE',  ( 0.005961354470445682716, -0.6427876096865404731, -0.7660212471507180654 ) ) ;
#12072 = CARTESIAN_POINT ( 'NONE',  ( -14.12721349658369085, 0.000000000000000000, 2.694479520900311620 ) ) ;
#12073 = ORIENTED_EDGE ( 'NONE', *, *, #43420, .T. ) ;
#12074 = DIRECTION ( 'NONE',  ( 0.5449076811759707706, 0.6444004775717708799, -0.5364919789714476250 ) ) ;
#12075 = CARTESIAN_POINT ( 'NONE',  ( -17.19780905594623732, -1.651309408375658538, 6.072224872292091291 ) ) ;
#12076 = ORIENTED_EDGE ( 'NONE', *, *, #46266, .T. ) ;
#12077 = FACE_OUTER_BOUND ( 'NONE', #38151, .T. ) ;
#12078 = LINE ( 'NONE', #50137, #17846 ) ;
#12079 = DIRECTION ( 'NONE',  ( 0.9999697198139515519, 0.000000000000000000, 0.007781995580013368816 ) ) ;
#12080 = CARTESIAN_POINT ( 'NONE',  ( -20.54204810873173415, 0.000000000000000000, 4.860550213503115558 ) ) ;
#12081 = VECTOR ( 'NONE', #29754, 1000.000000000000000 ) ;
#12082 = EDGE_CURVE ( 'NONE', #16969, #5084, #45666, .T. ) ;
#12083 = DIRECTION ( 'NONE',  ( 0.7660212471507180654, -0.6427876096865404731, 0.005961354470445141482 ) ) ;
#12084 = ORIENTED_EDGE ( 'NONE', *, *, #55919, .F. ) ;
#12085 = ADVANCED_FACE ( 'NONE', ( #2222 ), #32365, .F. ) ;
#12086 = EDGE_LOOP ( 'NONE', ( #50003, #37908, #27018, #6304 ) ) ;
#12087 = LINE ( 'NONE', #17470, #52986 ) ;
#12088 = CARTESIAN_POINT ( 'NONE',  ( -13.53673582514181106, 0.000000000000000000, 12.22817484722816772 ) ) ;
#12089 = DIRECTION ( 'NONE',  ( -0.005961354470445682716, -0.6427876096865404731, 0.7660212471507180654 ) ) ;
#12090 = EDGE_CURVE ( 'NONE', #16969, #42927, #28078, .T. ) ;
#12091 = AXIS2_PLACEMENT_3D ( 'NONE', #27356, #10044, #14333 ) ;
#12092 = DIRECTION ( 'NONE',  ( 0.007781995580012662783, 0.000000000000000000, -0.9999697198139514409 ) ) ;
#12093 = EDGE_CURVE ( 'NONE', #41034, #1167, #49381, .T. ) ;
#12094 = DIRECTION ( 'NONE',  ( -0.005961354470445682716, -0.6427876096865404731, 0.7660212471507180654 ) ) ;
#12095 = AXIS2_PLACEMENT_3D ( 'NONE', #40938, #48919, #10600 ) ;
#12096 = DIRECTION ( 'NONE',  ( -0.9999697198139514409, -0.000000000000000000, -0.007781995580013368816 ) ) ;
#12097 = FACE_OUTER_BOUND ( 'NONE', #17370, .T. ) ;
#12098 = CARTESIAN_POINT ( 'NONE',  ( -21.52029464965303518, 3.200641362704007786, 10.49333214280930093 ) ) ;
#12099 = FACE_OUTER_BOUND ( 'NONE', #2616, .T. ) ;
#12100 = AXIS2_PLACEMENT_3D ( 'NONE', #6674, #45555, #36790 ) ;
#12101 = LINE ( 'NONE', #3324, #21964 ) ;
#12102 = ORIENTED_EDGE ( 'NONE', *, *, #48544, .F. ) ;
#12103 = DIRECTION ( 'NONE',  ( -0.1139275668495183524, 0.9934890585767659488, 4.694855797473114533E-16 ) ) ;
#12104 = AXIS2_PLACEMENT_3D ( 'NONE', #44676, #9495, #18868 ) ;
#12105 = AXIS2_PLACEMENT_3D ( 'NONE', #18679, #10442, #9882 ) ;
#12106 = EDGE_LOOP ( 'NONE', ( #21816, #43293, #33467, #30516 ) ) ;
#12107 = ORIENTED_EDGE ( 'NONE', *, *, #5673, .F. ) ;
#12108 = ADVANCED_FACE ( 'NONE', ( #53629 ), #5653, .F. ) ;
#12109 = AXIS2_PLACEMENT_3D ( 'NONE', #30346, #11874, #25246 ) ;
#12110 = EDGE_LOOP ( 'NONE', ( #54085, #878, #4937, #38221 ) ) ;
#12111 = ORIENTED_EDGE ( 'NONE', *, *, #18771, .T. ) ;
#12112 = AXIS2_PLACEMENT_3D ( 'NONE', #19275, #36614, #53923 ) ;
#12113 = VERTEX_POINT ( 'NONE', #41137 ) ;
#12114 = ORIENTED_EDGE ( 'NONE', *, *, #4685, .T. ) ;
#12115 = LINE ( 'NONE', #42508, #38686 ) ;
#12116 = CARTESIAN_POINT ( 'NONE',  ( -21.47263955680318404, 0.000000000000000000, 5.022634149262071190 ) ) ;
#12117 = EDGE_CURVE ( 'NONE', #17901, #48104, #1394, .T. ) ;
#12118 = DIRECTION ( 'NONE',  ( 0.9999697198139515519, 0.000000000000000000, 0.007781995580013368816 ) ) ;
#12120 = EDGE_CURVE ( 'NONE', #28372, #24636, #10196, .T. ) ;
#12119 = ORIENTED_EDGE ( 'NONE', *, *, #41163, .T. ) ;
#12121 = LINE ( 'NONE', #20914, #15856 ) ;
#12122 = EDGE_LOOP ( 'NONE', ( #32534, #421, #7692, #40158 ) ) ;
#12123 = DIRECTION ( 'NONE',  ( 0.5449076811759707706, 0.6444004775717708799, -0.5364919789714476250 ) ) ;
#12124 = ORIENTED_EDGE ( 'NONE', *, *, #51420, .T. ) ;
#12125 = EDGE_CURVE ( 'NONE', #31757, #46955, #5958, .T. ) ;
#12126 = CARTESIAN_POINT ( 'NONE',  ( -65.94712367639533568, -9.257032740197443488, 4.837977870786231982 ) ) ;
#12127 = AXIS2_PLACEMENT_3D ( 'NONE', #939, #14020, #31633 ) ;
#12128 = DIRECTION ( 'NONE',  ( -0.005002170337468016433, -0.7660444431189770143, 0.6427681459581293666 ) ) ;
#12129 = CARTESIAN_POINT ( 'NONE',  ( -68.86155229709348191, -10.74924159303523830, -7.491897809418652798 ) ) ;
#12130 = EDGE_LOOP ( 'NONE', ( #25970, #46764, #51985, #29232 ) ) ;
#12131 = CARTESIAN_POINT ( 'NONE',  ( -11.00050607007353776, -1.489407457353157049, 3.399273247333383985 ) ) ;
#12132 = VECTOR ( 'NONE', #9278, 999.9999999999998863 ) ;
#12133 = ORIENTED_EDGE ( 'NONE', *, *, #37949, .T. ) ;
#12134 = ADVANCED_FACE ( 'NONE', ( #29781 ), #46806, .F. ) ;
#12135 = LINE ( 'NONE', #7907, #21915 ) ;
#12137 = VECTOR ( 'NONE', #33717, 1000.000000000000227 ) ;
#12136 = LINE ( 'NONE', #55573, #23890 ) ;
#12138 = EDGE_CURVE ( 'NONE', #27027, #34052, #42264, .T. ) ;
#12139 = DIRECTION ( 'NONE',  ( 0.6427681459581294776, -0.7660444431189769032, 0.005002170337467562802 ) ) ;
#12140 = DIRECTION ( 'NONE',  ( 0.007781995580012663651, 0.000000000000000000, -0.9999697198139515519 ) ) ;
#12141 = LINE ( 'NONE', #43100, #41071 ) ;
#12142 = CARTESIAN_POINT ( 'NONE',  ( -18.67775241435682432, 0.000000000000000000, 4.136394454059623804 ) ) ;
#12143 = DIRECTION ( 'NONE',  ( -0.9999697198139514409, -0.000000000000000000, -0.007781995580013368816 ) ) ;
#12144 = VECTOR ( 'NONE', #15145, 1000.000000000000227 ) ;
#12145 = LINE ( 'NONE', #43103, #7776 ) ;
#12146 = ORIENTED_EDGE ( 'NONE', *, *, #13053, .T. ) ;
#12147 = CARTESIAN_POINT ( 'NONE',  ( 2.072287782118878319, 0.000000000000000000, -2.950529333540147015 ) ) ;
#12148 = ORIENTED_EDGE ( 'NONE', *, *, #36620, .T. ) ;
#12149 = MECHANICAL_DESIGN_GEOMETRIC_PRESENTATION_REPRESENTATION (  '', ( #43002 ), #55684 ) ;
#12150 = CARTESIAN_POINT ( 'NONE',  ( -18.70442188201326061, -0.1191753592594160388, 6.621508366632224529 ) ) ;
#12151 = DIRECTION ( 'NONE',  ( -0.005961354470445682716, -0.6427876096865404731, 0.7660212471507180654 ) ) ;
#12152 = DIRECTION ( 'NONE',  ( -0.6427681459581293666, -0.7660444431189770143, -0.005002170337467561935 ) ) ;
#12153 = PLANE ( 'NONE',  #46808 ) ;
#12154 = LINE ( 'NONE', #43394, #4145 ) ;
#12155 = CIRCLE ( 'NONE', #15802, 6.999999999999999112 ) ;
#12156 = FACE_OUTER_BOUND ( 'NONE', #39852, .T. ) ;
#12157 = VECTOR ( 'NONE', #49814, 999.9999999999998863 ) ;
#12158 = CONTEXT_DEPENDENT_SHAPE_REPRESENTATION ( #15505, #40036 ) ;
#12159 = ORIENTED_EDGE ( 'NONE', *, *, #32639, .F. ) ;
#12160 = LINE ( 'NONE', #29495, #53719 ) ;
#12161 = CARTESIAN_POINT ( 'NONE',  ( -19.66742376178725493, 19.57123263517775769, 4.314754536491465231 ) ) ;
#12162 = CARTESIAN_POINT ( 'NONE',  ( -22.40556560354864146, -0.1191753592594197858, 5.484709000965211523 ) ) ;
#12163 = CARTESIAN_POINT ( 'NONE',  ( -32.65997012216863737, 0.000000000000000000, 9.567562649885804404 ) ) ;
#12164 = DIRECTION ( 'NONE',  ( 0.9999697198139515519, 0.000000000000000000, 0.007781995580013368816 ) ) ;
#12165 = EDGE_CURVE ( 'NONE', #48572, #29343, #37731, .T. ) ;
#12166 = DIRECTION ( 'NONE',  ( 0.7660212471507180654, -0.6427876096865404731, 0.005961354470445141482 ) ) ;
#12167 = CARTESIAN_POINT ( 'NONE',  ( -11.87243407472968926, 0.000000000000000000, 11.50246268866867361 ) ) ;
#12168 = CARTESIAN_POINT ( 'NONE',  ( -32.47108885958310509, 0.000000000000000000, 15.83124721154520387 ) ) ;
#12169 = ORIENTED_EDGE ( 'NONE', *, *, #2698, .T. ) ;
#12170 = AXIS2_PLACEMENT_3D ( 'NONE', #31444, #18932, #19182 ) ;
#12171 = CARTESIAN_POINT ( 'NONE',  ( -17.93139508144814442, 0.000000000000000000, 13.85596890686001537 ) ) ;
#12172 = CARTESIAN_POINT ( 'NONE',  ( -50.27554558092695913, 4.209026340267034705, 5.000000000000000000 ) ) ;
#12173 = ORIENTED_EDGE ( 'NONE', *, *, #43466, .T. ) ;
#12174 = VECTOR ( 'NONE', #34468, 999.9999999999998863 ) ;
#12175 = EDGE_LOOP ( 'NONE', ( #54070, #24289, #3808, #47227 ) ) ;
#12176 = CARTESIAN_POINT ( 'NONE',  ( -16.46764230182081334, 0.000000000000000000, 4.892258181606849554 ) ) ;
#12177 = VECTOR ( 'NONE', #12916, 1000.000000000000114 ) ;
#12178 = EDGE_CURVE ( 'NONE', #8704, #50967, #16996, .T. ) ;
#12179 = VERTEX_POINT ( 'NONE', #25235 ) ;
#12180 = FACE_OUTER_BOUND ( 'NONE', #54385, .T. ) ;
#12181 = ADVANCED_FACE ( 'NONE', ( #7612 ), #11605, .F. ) ;
#12182 = EDGE_CURVE ( 'NONE', #27886, #27953, #12720, .T. ) ;
#12183 = ORIENTED_EDGE ( 'NONE', *, *, #6216, .T. ) ;
#12184 = ORIENTED_EDGE ( 'NONE', *, *, #48013, .T. ) ;
#12185 = ORIENTED_EDGE ( 'NONE', *, *, #53984, .T. ) ;
#12186 = DIRECTION ( 'NONE',  ( -0.005961354470445682716, -0.6427876096865404731, 0.7660212471507180654 ) ) ;
#12187 = AXIS2_PLACEMENT_3D ( 'NONE', #36354, #15336, #49423 ) ;
#12188 = LINE ( 'NONE', #47110, #616 ) ;
#12189 = DIRECTION ( 'NONE',  ( -0.6427681459581293666, -0.7660444431189770143, -0.005002170337467561935 ) ) ;
#12190 = VECTOR ( 'NONE', #2371, 1000.000000000000000 ) ;
#12191 = ADVANCED_FACE ( 'NONE', ( #21233 ), #55054, .F. ) ;
#12192 = ORIENTED_EDGE ( 'NONE', *, *, #55303, .T. ) ;
#12193 = ORIENTED_EDGE ( 'NONE', *, *, #42887, .F. ) ;
#12194 = EDGE_CURVE ( 'NONE', #53603, #32511, #33194, .T. ) ;
#12195 = VECTOR ( 'NONE', #51768, 1000.000000000000114 ) ;
#12196 = VECTOR ( 'NONE', #51762, 1000.000000000000227 ) ;
#12197 = CARTESIAN_POINT ( 'NONE',  ( 2.072287782118878319, 0.000000000000000000, -2.950529333540147015 ) ) ;
#12198 = DIRECTION ( 'NONE',  ( 0.000000000000000000, -1.000000000000000000, 0.000000000000000000 ) ) ;
#12199 = VERTEX_POINT ( 'NONE', #3370 ) ;
#12200 = LINE ( 'NONE', #47394, #51807 ) ;
#12201 = LINE ( 'NONE', #51402, #33160 ) ;
#12202 = VERTEX_POINT ( 'NONE', #20940 ) ;
#12203 = CARTESIAN_POINT ( 'NONE',  ( -19.30682298318506085, 0.6102101463440048335, 5.382205634531532112 ) ) ;
#12204 = PLANE ( 'NONE',  #43026 ) ;
#12205 = EDGE_CURVE ( 'NONE', #11344, #39446, #3632, .T. ) ;
#12206 = ORIENTED_EDGE ( 'NONE', *, *, #3269, .F. ) ;
#12207 = PLANE ( 'NONE',  #21880 ) ;
#12208 = VECTOR ( 'NONE', #19788, 1000.000000000000227 ) ;
#12209 = EDGE_CURVE ( 'NONE', #56036, #695, #41954, .T. ) ;
#12210 = DIRECTION ( 'NONE',  ( -0.6427681459581293666, -0.7660444431189770143, -0.005002170337467561935 ) ) ;
#12211 = EDGE_LOOP ( 'NONE', ( #36866, #9539, #43610, #50816, #35988 ) ) ;
#12212 = CARTESIAN_POINT ( 'NONE',  ( -11.79540685186240800, 0.000000000000000000, 1.604629969967065195 ) ) ;
#12213 = CARTESIAN_POINT ( 'NONE',  ( -23.33849165029409889, 0.000000000000000000, 5.946783852668351855 ) ) ;
#12215 = VECTOR ( 'NONE', #19290, 1000.000000000000114 ) ;
#12214 = CARTESIAN_POINT ( 'NONE',  ( -13.37731649229117181, -4.889348428825665671, 1.921529324938835437 ) ) ;
#12216 = LINE ( 'NONE', #49974, #30155 ) ;
#12217 = ORIENTED_EDGE ( 'NONE', *, *, #29841, .T. ) ;
#12218 = VECTOR ( 'NONE', #17116, 1000.000000000000227 ) ;
#12219 = CARTESIAN_POINT ( 'NONE',  ( -19.60834386242827776, 0.000000000000000000, 4.298478389818581213 ) ) ;
#12220 = CARTESIAN_POINT ( 'NONE',  ( -46.27156441860557123, 5.366025403784241199, -5.000000000000000000 ) ) ;
#12221 = VECTOR ( 'NONE', #6552, 1000.000000000000227 ) ;
#12222 = FACE_OUTER_BOUND ( 'NONE', #28212, .T. ) ;
#12223 = DIRECTION ( 'NONE',  ( 0.6427681459581294776, -0.7660444431189769032, 0.005002170337467562802 ) ) ;
#12224 = DIRECTION ( 'NONE',  ( 0.9999697198139515519, 0.000000000000000000, 0.007781995580013368816 ) ) ;
#12225 = VECTOR ( 'NONE', #36176, 1000.000000000000227 ) ;
#12226 = CARTESIAN_POINT ( 'NONE',  ( -69.27886756364613063, -9.773082162198893030, -7.306024462451856216 ) ) ;
#12227 = AXIS2_PLACEMENT_3D ( 'NONE', #42342, #38066, #33269 ) ;
#12228 = ORIENTED_EDGE ( 'NONE', *, *, #5869, .F. ) ;
#12229 = DIRECTION ( 'NONE',  ( 0.6427681459581294776, -0.7660444431189769032, 0.005002170337467562802 ) ) ;
#12230 = ORIENTED_EDGE ( 'NONE', *, *, #7507, .F. ) ;
#12231 = VECTOR ( 'NONE', #55704, 999.9999999999998863 ) ;
#12232 = CARTESIAN_POINT ( 'NONE',  ( -22.04728230093569152, 19.65758605842115969, -4.422151119964278010 ) ) ;
#12233 = DIRECTION ( 'NONE',  ( 0.9090593428863090741, 0.000000000000000000, 0.4166666666666674623 ) ) ;
#12234 = VECTOR ( 'NONE', #53991, 1000.000000000000114 ) ;
#12235 = FACE_OUTER_BOUND ( 'NONE', #13401, .T. ) ;
#12236 = ADVANCED_FACE ( 'NONE', ( #51619 ), #50769, .F. ) ;
#12237 = CARTESIAN_POINT ( 'NONE',  ( -31.72704407542318350, -0.1191753592594197858, 9.105487798182664960 ) ) ;
#12238 = CARTESIAN_POINT ( 'NONE',  ( -24.83619032682412353, 18.20871928901600256, 4.561852666301203563 ) ) ;
#12239 = ORIENTED_EDGE ( 'NONE', *, *, #52216, .T. ) ;
#12240 = VECTOR ( 'NONE', #14839, 1000.000000000000114 ) ;
#12241 = VECTOR ( 'NONE', #12388, 999.9999999999998863 ) ;
#12242 = EDGE_CURVE ( 'NONE', #54113, #37795, #24371, .T. ) ;
#12243 = ORIENTED_EDGE ( 'NONE', *, *, #35806, .T. ) ;
#12244 = DIRECTION ( 'NONE',  ( -0.005002170337468016433, -0.7660444431189770143, 0.6427681459581293666 ) ) ;
#12245 = DIRECTION ( 'NONE',  ( -0.005002170337468016433, -0.7660444431189770143, 0.6427681459581293666 ) ) ;
#12246 = ORIENTED_EDGE ( 'NONE', *, *, #38700, .F. ) ;
#12247 = EDGE_CURVE ( 'NONE', #35835, #43081, #42800, .T. ) ;
#12248 = EDGE_CURVE ( 'NONE', #24292, #1300, #41682, .T. ) ;
#12249 = EDGE_CURVE ( 'NONE', #21318, #30294, #33723, .T. ) ;
#12250 = LINE ( 'NONE', #7710, #43835 ) ;
#12251 = VERTEX_POINT ( 'NONE', #28926 ) ;
#12252 = CARTESIAN_POINT ( 'NONE',  ( -16.81190032086591302, 0.000000000000000000, 3.212244750653343583 ) ) ;
#12253 = EDGE_LOOP ( 'NONE', ( #47893, #38887, #15228, #50105 ) ) ;
#12254 = LINE ( 'NONE', #11692, #22043 ) ;
#12255 = EDGE_CURVE ( 'NONE', #29153, #20285, #11858, .T. ) ;
#12256 = VECTOR ( 'NONE', #12939, 999.9999999999998863 ) ;
#12257 = EDGE_LOOP ( 'NONE', ( #17899, #25073, #11769, #23168 ) ) ;
#12258 = ORIENTED_EDGE ( 'NONE', *, *, #31174, .F. ) ;
#12259 = VERTEX_POINT ( 'NONE', #46216 ) ;
#12260 = VECTOR ( 'NONE', #39677, 999.9999999999998863 ) ;
#12261 = DIRECTION ( 'NONE',  ( 0.5449076811759707706, 0.6444004775717708799, -0.5364919789714476250 ) ) ;
#12262 = DIRECTION ( 'NONE',  ( 0.007781995580012663651, 0.000000000000000000, -0.9999697198139515519 ) ) ;
#12263 = AXIS2_PLACEMENT_3D ( 'NONE', #9082, #9355, #36071 ) ;
#12264 = LINE ( 'NONE', #25323, #22118 ) ;
#12265 = PLANE ( 'NONE',  #4794 ) ;
#12266 = EDGE_CURVE ( 'NONE', #39740, #28953, #7325, .T. ) ;
#12267 = VECTOR ( 'NONE', #7196, 999.9999999999998863 ) ;
#12268 = ORIENTED_EDGE ( 'NONE', *, *, #44272, .F. ) ;
#12270 = ORIENTED_EDGE ( 'NONE', *, *, #53050, .T. ) ;
#12269 = EDGE_CURVE ( 'NONE', #56078, #14391, #5056, .T. ) ;
#12271 = ORIENTED_EDGE ( 'NONE', *, *, #31806, .T. ) ;
#12272 = VECTOR ( 'NONE', #21368, 1000.000000000000114 ) ;
#12273 = PLANE ( 'NONE',  #29520 ) ;
#12274 = AXIS2_PLACEMENT_3D ( 'NONE', #24349, #16666, #37979 ) ;
#12275 = LINE ( 'NONE', #29616, #14594 ) ;
#12276 = EDGE_CURVE ( 'NONE', #31601, #26572, #39411, .T. ) ;
#12277 = ORIENTED_EDGE ( 'NONE', *, *, #40844, .T. ) ;
#12278 = VECTOR ( 'NONE', #1751, 1000.000000000000114 ) ;
#12279 = DIRECTION ( 'NONE',  ( -0.5449076811759708816, 0.6444004775717707689, 0.5364919789714475140 ) ) ;
#12280 = ORIENTED_EDGE ( 'NONE', *, *, #21641, .F. ) ;
#12281 = PLANE ( 'NONE',  #21476 ) ;
#12282 = PLANE ( 'NONE',  #6789 ) ;
#12283 = VECTOR ( 'NONE', #43648, 1000.000000000000114 ) ;
#12284 = EDGE_CURVE ( 'NONE', #6407, #23847, #26921, .T. ) ;
#12285 = ORIENTED_EDGE ( 'NONE', *, *, #19801, .T. ) ;
#12286 = VECTOR ( 'NONE', #12968, 1000.000000000000000 ) ;
#12287 = DIRECTION ( 'NONE',  ( -0.6427681459581293666, -0.7660444431189770143, -0.005002170337467561935 ) ) ;
#12288 = ORIENTED_EDGE ( 'NONE', *, *, #50732, .F. ) ;
#12289 = AXIS2_PLACEMENT_3D ( 'NONE', #17929, #22472, #44029 ) ;
#12290 = CARTESIAN_POINT ( 'NONE',  ( -18.81801092196306513, 0.000000000000000000, 8.367281711381659548 ) ) ;
#12291 = VECTOR ( 'NONE', #19709, 1000.000000000000227 ) ;
#12292 = LINE ( 'NONE', #25079, #51976 ) ;
#12293 = VERTEX_POINT ( 'NONE', #502 ) ;
#12294 = SHAPE_REPRESENTATION ( 'Integrated Nail File & Cleaner Flip-Out', ( #2610 ), #48882 ) ;
#12295 = CARTESIAN_POINT ( 'NONE',  ( -12.15271748404464880, 0.000000000000000000, 1.601849296007406664 ) ) ;
#12296 = DIRECTION ( 'NONE',  ( 0.7660212471507180654, -0.6427876096865404731, 0.005961354470445141482 ) ) ;
#12297 = CARTESIAN_POINT ( 'NONE',  ( -20.27233569796318946, 2.876837460659008361, 4.464609191105296304 ) ) ;
#12298 = DIRECTION ( 'NONE',  ( 0.5449076811759707706, 0.6444004775717708799, -0.5364919789714476250 ) ) ;
#12299 = EDGE_LOOP ( 'NONE', ( #53970, #12505, #44953, #38103 ) ) ;
#12300 = EDGE_LOOP ( 'NONE', ( #1302, #55084, #26289, #36249 ) ) ;
#12301 = DIRECTION ( 'NONE',  ( 0.5364919789714477361, 0.6444004775717706579, 0.5449076811759711036 ) ) ;
#12302 = DIRECTION ( 'NONE',  ( -0.6427681459581293666, -0.7660444431189770143, -0.005002170337467561935 ) ) ;
#12303 = DIRECTION ( 'NONE',  ( 0.7660212471507180654, -0.6427876096865404731, 0.005961354470445141482 ) ) ;
#12304 = DIRECTION ( 'NONE',  ( -0.005002170337468016433, -0.7660444431189770143, 0.6427681459581293666 ) ) ;
#12305 = LINE ( 'NONE', #43261, #35199 ) ;
#12306 = VECTOR ( 'NONE', #8001, 999.9999999999998863 ) ;
#12307 = CARTESIAN_POINT ( 'NONE',  ( -10.94028622754223967, 0.000000000000000000, 11.14038480894692995 ) ) ;
#12308 = EDGE_LOOP ( 'NONE', ( #37152, #48214, #52904, #45171 ) ) ;
#12309 = VECTOR ( 'NONE', #13733, 999.9999999999998863 ) ;
#12310 = CARTESIAN_POINT ( 'NONE',  ( -13.93296765963146733, 0.000000000000000000, 3.434655326531841357 ) ) ;
#12311 = CARTESIAN_POINT ( 'NONE',  ( -17.66000264926527663, 0.000000000000000000, 4.682972901456035508 ) ) ;
#12312 = ORIENTED_EDGE ( 'NONE', *, *, #20555, .F. ) ;
#12313 = LINE ( 'NONE', #21087, #15028 ) ;
#12314 = AXIS2_PLACEMENT_3D ( 'NONE', #25634, #42960, #4068 ) ;
#12315 = VERTEX_POINT ( 'NONE', #43645 ) ;
#12316 = EDGE_CURVE ( 'NONE', #33009, #28898, #21540, .T. ) ;
#12317 = CARTESIAN_POINT ( 'NONE',  ( -18.86354292863559579, 0.000000000000000000, 14.21804678658176080 ) ) ;
#12318 = LINE ( 'NONE', #20817, #53233 ) ;
#12319 = VECTOR ( 'NONE', #26681, 999.9999999999998863 ) ;
#12320 = ADVANCED_FACE ( 'NONE', ( #34870 ), #22384, .F. ) ;
#12321 = LINE ( 'NONE', #7784, #15047 ) ;
#12322 = FACE_OUTER_BOUND ( 'NONE', #18823, .T. ) ;
#12323 = CARTESIAN_POINT ( 'NONE',  ( -69.53817124046049969, 0.1329910790360524786, -6.894786738958806005 ) ) ;
#12324 = EDGE_LOOP ( 'NONE', ( #3342, #8932, #10374, #15342 ) ) ;
#12325 = VECTOR ( 'NONE', #12839, 999.9999999999998863 ) ;
#12326 = VECTOR ( 'NONE', #3255, 999.9999999999998863 ) ;
#12327 = ORIENTED_EDGE ( 'NONE', *, *, #34822, .T. ) ;
#12328 = CARTESIAN_POINT ( 'NONE',  ( -67.03776378471746966, -0.6009246745546259483, 0.6758588499069816402 ) ) ;
#12329 = DIRECTION ( 'NONE',  ( 0.6427681459581294776, -0.7660444431189769032, 0.005002170337467562802 ) ) ;
#12330 = CARTESIAN_POINT ( 'NONE',  ( -14.20280369269832832, 0.000000000000000000, 12.40765738797303719 ) ) ;
#12331 = ADVANCED_FACE ( 'NONE', ( #22644 ), #47648, .F. ) ;
#12332 = AXIS2_PLACEMENT_3D ( 'NONE', #2650, #37292, #54601 ) ;
#12333 = ADVANCED_FACE ( 'NONE', ( #30327 ), #5335, .F. ) ;
#12334 = ADVANCED_FACE ( 'NONE', ( #26085 ), #1040, .F. ) ;
#12335 = LINE ( 'NONE', #7795, #42366 ) ;
#12337 = CARTESIAN_POINT ( 'NONE',  ( -30.79489622823572859, -0.1191753592594197858, 8.743409918460921304 ) ) ;
#12336 = VECTOR ( 'NONE', #46474, 1000.000000000000227 ) ;
#12338 = DIRECTION ( 'NONE',  ( -0.005961354470445682716, -0.6427876096865404731, 0.7660212471507180654 ) ) ;
#12339 = VECTOR ( 'NONE', #22097, 1000.000000000000000 ) ;
#12341 = EDGE_CURVE ( 'NONE', #34812, #24159, #18096, .T. ) ;
#12340 = ORIENTED_EDGE ( 'NONE', *, *, #42529, .F. ) ;
#12342 = DIRECTION ( 'NONE',  ( 0.000000000000000000, -0.000000000000000000, -1.000000000000000000 ) ) ;
#12343 = VECTOR ( 'NONE', #30213, 999.9999999999998863 ) ;
#12344 = CARTESIAN_POINT ( 'NONE',  ( -20.54126990917373519, -0.1191753592594197858, 4.760553241521720658 ) ) ;
#12345 = AXIS2_PLACEMENT_3D ( 'NONE', #54523, #49739, #2838 ) ;
#12346 = LINE ( 'NONE', #17151, #38755 ) ;
#12347 = EDGE_LOOP ( 'NONE', ( #41857, #23866, #30000, #16819 ) ) ;
#12348 = CARTESIAN_POINT ( 'NONE',  ( -11.64304826722768382, 25.38767603887911051, -3.000000000000000000 ) ) ;
#12349 = CARTESIAN_POINT ( 'NONE',  ( -12.80458192191714595, 0.000000000000000000, 11.86454056839041726 ) ) ;
#12350 = DIRECTION ( 'NONE',  ( 0.007781995580012663651, -3.146120232559066537E-19, -0.9999697198139514409 ) ) ;
#12351 = ORIENTED_EDGE ( 'NONE', *, *, #26354, .F. ) ;
#12352 = CARTESIAN_POINT ( 'NONE',  ( -18.67619601524082285, 0.000000000000000000, 3.936400510096834893 ) ) ;
#12353 = ORIENTED_EDGE ( 'NONE', *, *, #23718, .T. ) ;
#12354 = ADVANCED_FACE ( 'NONE', ( #17839 ), #35171, .F. ) ;
#12355 = VECTOR ( 'NONE', #45687, 1000.000000000000227 ) ;
#12356 = ORIENTED_EDGE ( 'NONE', *, *, #47474, .T. ) ;
#12357 = ORIENTED_EDGE ( 'NONE', *, *, #8340, .F. ) ;
#12358 = ADVANCED_FACE ( 'NONE', ( #190 ), #52465, .F. ) ;
#12359 = VERTEX_POINT ( 'NONE', #48182 ) ;
#12360 = DIRECTION ( 'NONE',  ( -0.005961354470445682716, -0.6427876096865404731, 0.7660212471507180654 ) ) ;
#12361 = AXIS2_PLACEMENT_3D ( 'NONE', #19412, #37285, #49802 ) ;
#12362 = ORIENTED_EDGE ( 'NONE', *, *, #23846, .F. ) ;
#12363 = CARTESIAN_POINT ( 'NONE',  ( -12.29957260759845106, 23.82506348239776273, -3.515194272803603415 ) ) ;
#12364 = EDGE_CURVE ( 'NONE', #17653, #45526, #25784, .T. ) ;
#12365 = ORIENTED_EDGE ( 'NONE', *, *, #22339, .T. ) ;
#12366 = CARTESIAN_POINT ( 'NONE',  ( -19.12962290826653700, 0.000000000000000000, 14.40064212555863854 ) ) ;
#12367 = ORIENTED_EDGE ( 'NONE', *, *, #12266, .T. ) ;
#12368 = VECTOR ( 'NONE', #19568, 1000.000000000000227 ) ;
#12369 = EDGE_LOOP ( 'NONE', ( #42617, #1226 ) ) ;
#12370 = EDGE_CURVE ( 'NONE', #20361, #45048, #38853, .T. ) ;
#12371 = AXIS2_PLACEMENT_3D ( 'NONE', #25855, #39757, #47984 ) ;
#12372 = VECTOR ( 'NONE', #41801, 1000.000000000000227 ) ;
#12373 = DIRECTION ( 'NONE',  ( 0.9999697198139515519, 0.000000000000000000, 0.007781995580013368816 ) ) ;
#12374 = DIRECTION ( 'NONE',  ( -0.9999697198139514409, -0.000000000000000000, -0.007781995580013368816 ) ) ;
#12375 = LINE ( 'NONE', #43318, #23152 ) ;
#12376 = DIRECTION ( 'NONE',  ( 0.000000000000000000, -0.000000000000000000, -1.000000000000000000 ) ) ;
#12377 = FILL_AREA_STYLE ('',( #29957 ) ) ;
#12378 = VERTEX_POINT ( 'NONE', #43932 ) ;
#12379 = VECTOR ( 'NONE', #33100, 999.9999999999998863 ) ;
#12380 = ORIENTED_EDGE ( 'NONE', *, *, #1843, .T. ) ;
#12381 = AXIS2_PLACEMENT_3D ( 'NONE', #19694, #2362, #6923 ) ;
#12382 = DIRECTION ( 'NONE',  ( -0.6427681459581293666, -0.7660444431189770143, -0.005002170337467561935 ) ) ;
#12383 = PLANE ( 'NONE',  #53881 ) ;
#12384 = VECTOR ( 'NONE', #6896, 1000.000000000000000 ) ;
#12385 = CARTESIAN_POINT ( 'NONE',  ( -18.66354898467281132, 0.000000000000000000, 14.21960318569776582 ) ) ;
#12386 = VECTOR ( 'NONE', #54082, 1000.000000000000114 ) ;
#12387 = DIRECTION ( 'NONE',  ( 0.007781995580012663651, 0.000000000000000000, -0.9999697198139515519 ) ) ;
#12388 = DIRECTION ( 'NONE',  ( 0.5364919789714477361, 0.6444004775717706579, 0.5449076811759711036 ) ) ;
#12389 = DIRECTION ( 'NONE',  ( 0.9999697198139515519, 0.000000000000000000, 0.007781995580013368816 ) ) ;
#12390 = ORIENTED_EDGE ( 'NONE', *, *, #24149, .F. ) ;
#12391 = CARTESIAN_POINT ( 'NONE',  ( -21.47419595591918906, 0.000000000000000000, 5.222628093224860102 ) ) ;
#12392 = PLANE ( 'NONE',  #53047 ) ;
#12393 = EDGE_LOOP ( 'NONE', ( #47804, #13207, #4412, #8143 ) ) ;
#12394 = CARTESIAN_POINT ( 'NONE',  ( -17.36532418587302473, -0.1191753592594177458, 13.67570816655714516 ) ) ;
#12395 = DIRECTION ( 'NONE',  ( 0.000000000000000000, -0.000000000000000000, -1.000000000000000000 ) ) ;
#12396 = DIRECTION ( 'NONE',  ( 0.5364919789714477361, 0.6444004775717706579, 0.5449076811759711036 ) ) ;
#12397 = DIRECTION ( 'NONE',  ( 0.007781995580012663651, -3.146120232559066537E-19, -0.9999697198139514409 ) ) ;
#12398 = PLANE ( 'NONE',  #37707 ) ;
#12399 = VECTOR ( 'NONE', #20744, 1000.000000000000227 ) ;
#12400 = ORIENTED_EDGE ( 'NONE', *, *, #3666, .F. ) ;
#12401 = ORIENTED_EDGE ( 'NONE', *, *, #1583, .T. ) ;
#12402 = CARTESIAN_POINT ( 'NONE',  ( -18.79082678602624057, 0.000000000000000000, 4.874178622766801361 ) ) ;
#12403 = DIRECTION ( 'NONE',  ( -0.7660212471507179544, -0.6427876096865405842, -0.005961354470445141482 ) ) ;
#12404 = DIRECTION ( 'NONE',  ( -0.5449076811759708816, 0.6444004775717707689, 0.5364919789714475140 ) ) ;
#12405 = AXIS2_PLACEMENT_3D ( 'NONE', #44084, #9998, #31001 ) ;
#12406 = ADVANCED_FACE ( 'NONE', ( #39700 ), #52724, .F. ) ;
#12407 = CARTESIAN_POINT ( 'NONE',  ( 5.681647518099910421, -6.217723448642447082, -2.166220689508504549 ) ) ;
#12408 = VECTOR ( 'NONE', #41842, 1000.000000000000227 ) ;
#12409 = DIRECTION ( 'NONE',  ( 0.005002170337468016433, -0.7660444431189770143, -0.6427681459581293666 ) ) ;
#12410 = EDGE_CURVE ( 'NONE', #49806, #22744, #17249, .T. ) ;
#12411 = PLANE ( 'NONE',  #51837 ) ;
#12412 = EDGE_CURVE ( 'NONE', #21743, #52239, #2157, .T. ) ;
#12413 = PLANE ( 'NONE',  #21103 ) ;
#12415 = AXIS2_PLACEMENT_3D ( 'NONE', #13829, #39954, #31155 ) ;
#12414 = CARTESIAN_POINT ( 'NONE',  ( -8.898634305293546376, -0.08571482049900724931, 4.084417208347257855 ) ) ;
#12416 = CARTESIAN_POINT ( 'NONE',  ( -30.79567442779373110, 0.000000000000000000, 8.843406890442315316 ) ) ;
#12417 = FACE_OUTER_BOUND ( 'NONE', #24610, .T. ) ;
#12418 = ORIENTED_EDGE ( 'NONE', *, *, #47573, .T. ) ;
#12419 = DIRECTION ( 'NONE',  ( 0.007781995580012663651, 0.000000000000000000, -0.9999697198139515519 ) ) ;
#12420 = ORIENTED_EDGE ( 'NONE', *, *, #30848, .T. ) ;
#12421 = VECTOR ( 'NONE', #1316, 999.9999999999998863 ) ;
#12422 = EDGE_LOOP ( 'NONE', ( #49865, #19031, #49649, #38823 ) ) ;
#12423 = VECTOR ( 'NONE', #47688, 1000.000000000000227 ) ;
#12424 = ORIENTED_EDGE ( 'NONE', *, *, #47031, .F. ) ;
#12425 = AXIS2_PLACEMENT_3D ( 'NONE', #44858, #13910, #40031 ) ;
#12426 = ORIENTED_EDGE ( 'NONE', *, *, #28155, .F. ) ;
#12427 = VERTEX_POINT ( 'NONE', #23219 ) ;
#12428 = ORIENTED_EDGE ( 'NONE', *, *, #16396, .T. ) ;
#12429 = CARTESIAN_POINT ( 'NONE',  ( -20.29244006095147412, 0.000000000000000000, 5.401150804439980746 ) ) ;
#12430 = PLANE ( 'NONE',  #3894 ) ;
#12431 = CARTESIAN_POINT ( 'NONE',  ( -12.33850799832341849, 0.000000000000000000, 11.68350162852954632 ) ) ;
#12432 = VERTEX_POINT ( 'NONE', #1627 ) ;
#12433 = CARTESIAN_POINT ( 'NONE',  ( -0.08953432831225546784, -3.865803998196977176, 3.253151749378868640 ) ) ;
#12434 = ORIENTED_EDGE ( 'NONE', *, *, #21921, .T. ) ;
#12435 = CARTESIAN_POINT ( 'NONE',  ( -19.03250079184375210, -4.889348428825662118, 12.09905512791755555 ) ) ;
#12436 = ORIENTED_EDGE ( 'NONE', *, *, #15634, .F. ) ;
#12437 = EDGE_CURVE ( 'NONE', #12832, #15388, #44486, .T. ) ;
#12438 = VECTOR ( 'NONE', #33565, 1000.000000000000000 ) ;
#12439 = PLANE ( 'NONE',  #34719 ) ;
#12440 = EDGE_CURVE ( 'NONE', #32724, #43237, #19494, .T. ) ;
#12441 = DIRECTION ( 'NONE',  ( 0.007781995580012663651, -3.146120232559066537E-19, -0.9999697198139514409 ) ) ;
#12442 = DIRECTION ( 'NONE',  ( 0.3535533905932752297, -0.6123724356957952475, -0.7071067811865462405 ) ) ;
#12443 = EDGE_CURVE ( 'NONE', #30915, #26710, #45081, .T. ) ;
#12444 = ORIENTED_EDGE ( 'NONE', *, *, #44847, .T. ) ;
#12445 = DIRECTION ( 'NONE',  ( 0.7660212471507180654, -0.6427876096865404731, 0.005961354470445141482 ) ) ;
#12446 = ORIENTED_EDGE ( 'NONE', *, *, #44847, .F. ) ;
#12447 = CARTESIAN_POINT ( 'NONE',  ( -17.74560456716937296, 0.000000000000000000, 3.774316574337878372 ) ) ;
#12448 = VECTOR ( 'NONE', #47822, 1000.000000000000227 ) ;
#12449 = EDGE_CURVE ( 'NONE', #55206, #46834, #45334, .T. ) ;
#12450 = LINE ( 'NONE', #7311, #34805 ) ;
#12451 = CARTESIAN_POINT ( 'NONE',  ( -25.20200914511100265, -0.1191753592594197858, 6.570942640130446932 ) ) ;
#12452 = VECTOR ( 'NONE', #29059, 1000.000000000000227 ) ;
#12453 = DIRECTION ( 'NONE',  ( -0.005961354470445682716, -0.6427876096865404731, 0.7660212471507180654 ) ) ;
#12454 = DIRECTION ( 'NONE',  ( -0.5364919789714478471, 0.6444004775717705469, -0.5449076811759709926 ) ) ;
#12455 = DIRECTION ( 'NONE',  ( -0.005002170337468016433, -0.7660444431189770143, 0.6427681459581293666 ) ) ;
#12456 = LINE ( 'NONE', #51033, #7599 ) ;
#12457 = DIRECTION ( 'NONE',  ( -0.005961354470445682716, -0.6427876096865404731, 0.7660212471507180654 ) ) ;
#12458 = ORIENTED_EDGE ( 'NONE', *, *, #46552, .T. ) ;
#12459 = CARTESIAN_POINT ( 'NONE',  ( -19.60912206198628027, -0.1191753592594197858, 4.398475361799976113 ) ) ;
#12460 = EDGE_LOOP ( 'NONE', ( #52919, #52718, #12703, #14349, #21656 ) ) ;
#12461 = VECTOR ( 'NONE', #35927, 1000.000000000000227 ) ;
#12462 = DIRECTION ( 'NONE',  ( 0.5449076811759707706, 0.6444004775717708799, -0.5364919789714476250 ) ) ;
#12463 = CARTESIAN_POINT ( 'NONE',  ( -15.96710241509184058, -0.1191753592594218814, 13.13259134697452879 ) ) ;
#12464 = DIRECTION ( 'NONE',  ( 0.000000000000000000, -1.000000000000000000, 0.000000000000000000 ) ) ;
#12465 = LINE ( 'NONE', #29783, #15872 ) ;
#12466 = LINE ( 'NONE', #20692, #8692 ) ;
#12467 = CARTESIAN_POINT ( 'NONE',  ( -18.89843909413720624, 4.495856970884009485, 11.60058387806120273 ) ) ;
#12468 = APPLICATION_PROTOCOL_DEFINITION ( 'draft international standard', 'automotive_design', 1998, #24239 ) ;
#12469 = ORIENTED_EDGE ( 'NONE', *, *, #17190, .F. ) ;
#12470 = DIRECTION ( 'NONE',  ( -0.9999697198139514409, -0.000000000000000000, -0.007781995580013368816 ) ) ;
#12471 = LINE ( 'NONE', #21244, #1347 ) ;
#12472 = EDGE_CURVE ( 'NONE', #35002, #41926, #19780, .T. ) ;
#12473 = DIRECTION ( 'NONE',  ( 0.000000000000000000, 0.000000000000000000, 1.000000000000000000 ) ) ;
#12474 = EDGE_CURVE ( 'NONE', #44163, #52435, #23748, .T. ) ;
#12475 = FACE_OUTER_BOUND ( 'NONE', #24600, .T. ) ;
#12476 = DIRECTION ( 'NONE',  ( 1.000000000000000000, 0.000000000000000000, 0.000000000000000000 ) ) ;
#12477 = CARTESIAN_POINT ( 'NONE',  ( 2.072287782118878319, 0.000000000000000000, -2.950529333540147015 ) ) ;
#12478 = EDGE_CURVE ( 'NONE', #41818, #7991, #5595, .T. ) ;
#12479 = DIRECTION ( 'NONE',  ( 0.007781995580012663651, -3.146120232559066537E-19, -0.9999697198139514409 ) ) ;
#12480 = ORIENTED_EDGE ( 'NONE', *, *, #55712, .T. ) ;
#12481 = CARTESIAN_POINT ( 'NONE',  ( -14.61771687497231653, 0.000000000000000000, 6.014650938452181350 ) ) ;
#12482 = PLANE ( 'NONE',  #49577 ) ;
#12483 = ORIENTED_EDGE ( 'NONE', *, *, #41415, .T. ) ;
#12484 = ORIENTED_EDGE ( 'NONE', *, *, #9442, .F. ) ;
#12485 = DIRECTION ( 'NONE',  ( 0.005961354470445682716, -0.6427876096865404731, -0.7660212471507180654 ) ) ;
#12486 = ORIENTED_EDGE ( 'NONE', *, *, #26071, .T. ) ;
#12487 = EDGE_CURVE ( 'NONE', #26117, #30596, #10136, .T. ) ;
#12488 = AXIS2_PLACEMENT_3D ( 'NONE', #3578, #25186, #41901 ) ;
#12489 = EDGE_LOOP ( 'NONE', ( #20501, #39140, #24285, #34960 ) ) ;
#12490 = EDGE_LOOP ( 'NONE', ( #23406, #18410, #3307, #4350 ) ) ;
#12491 = ORIENTED_EDGE ( 'NONE', *, *, #19403, .F. ) ;
#12492 = DIRECTION ( 'NONE',  ( -0.005002170337468016433, -0.7660444431189770143, 0.6427681459581293666 ) ) ;
#12493 = LINE ( 'NONE', #25266, #5170 ) ;
#12494 = DIRECTION ( 'NONE',  ( 0.005002170337468016433, -0.7660444431189770143, -0.6427681459581293666 ) ) ;
#12495 = VECTOR ( 'NONE', #45452, 999.9999999999998863 ) ;
#12496 = EDGE_LOOP ( 'NONE', ( #48702, #50376, #48646, #34538 ) ) ;
#12497 = EDGE_LOOP ( 'NONE', ( #39158, #4250, #38101, #12960 ) ) ;
#12498 = LINE ( 'NONE', #8807, #27466 ) ;
#12499 = LINE ( 'NONE', #46853, #20938 ) ;
#12500 = VERTEX_POINT ( 'NONE', #36272 ) ;
#12501 = FACE_OUTER_BOUND ( 'NONE', #28683, .T. ) ;
#12502 = LINE ( 'NONE', #26370, #36776 ) ;
#12503 = EDGE_LOOP ( 'NONE', ( #710, #50096, #10170, #52663 ) ) ;
#12504 = LINE ( 'NONE', #38313, #4969 ) ;
#12505 = ORIENTED_EDGE ( 'NONE', *, *, #52272, .T. ) ;
#12506 = CARTESIAN_POINT ( 'NONE',  ( -11.83121314831507931, 0.000000000000000000, 6.205662168355214448 ) ) ;
#12507 = ADVANCED_FACE ( 'NONE', ( #49319 ), #6443, .F. ) ;
#12508 = CARTESIAN_POINT ( 'NONE',  ( -17.39147930267917275, 1.095915999411505082, 5.435347155529250962 ) ) ;
#12509 = VERTEX_POINT ( 'NONE', #44779 ) ;
#12510 = DIRECTION ( 'NONE',  ( 0.9999697198139515519, 0.000000000000000000, 0.007781995580013368816 ) ) ;
#12511 = LINE ( 'NONE', #21295, #27489 ) ;
#12512 = CARTESIAN_POINT ( 'NONE',  ( -17.76077782080467315, -0.1191753592594195638, 4.782191673879427007 ) ) ;
#12513 = LINE ( 'NONE', #26383, #11086 ) ;
#12514 = ORIENTED_EDGE ( 'NONE', *, *, #44107, .T. ) ;
#12515 = EDGE_CURVE ( 'NONE', #42394, #52748, #6263, .T. ) ;
#12516 = B_SPLINE_CURVE_WITH_KNOTS ( 'NONE', 3,
 ( #44984, #31363, #697, #9795 ),
 .UNSPECIFIED., .F., .F.,
 ( 4, 4 ),
 ( 0.0001724778598249929792, 0.0003421153678589267371 ),
 .UNSPECIFIED. ) ;
#12517 = DIRECTION ( 'NONE',  ( -0.6427681459581293666, -0.7660444431189770143, -0.005002170337467561935 ) ) ;
#12518 = CARTESIAN_POINT ( 'NONE',  ( -17.32488145901641374, -0.1191753592594153865, 8.478904618225078238 ) ) ;
#12519 = FACE_OUTER_BOUND ( 'NONE', #2155, .T. ) ;
#12520 = CARTESIAN_POINT ( 'NONE',  ( -18.67697421479883602, -0.1191753592594185784, 4.036397482078228904 ) ) ;
#12521 = EDGE_CURVE ( 'NONE', #32241, #50224, #40805, .T. ) ;
#12522 = FACE_OUTER_BOUND ( 'NONE', #33133, .T. ) ;
#12524 = EDGE_CURVE ( 'NONE', #27823, #2633, #1878, .T. ) ;
#12523 = CARTESIAN_POINT ( 'NONE',  ( -9.442067484779661513, -0.1191753592594197858, 10.59804618892231254 ) ) ;
#12525 = DIRECTION ( 'NONE',  ( -0.5449076811759708816, 0.6444004775717707689, 0.5364919789714475140 ) ) ;
#12526 = ORIENTED_EDGE ( 'NONE', *, *, #32056, .T. ) ;
#12527 = CARTESIAN_POINT ( 'NONE',  ( -67.66270444019232855, -5.290906601729261638E-14, 7.224227263221078665 ) ) ;
#12528 = ORIENTED_EDGE ( 'NONE', *, *, #22411, .T. ) ;
#12529 = DIRECTION ( 'NONE',  ( 0.7660212471507180654, -0.6427876096865404731, 0.005961354470445141482 ) ) ;
#12530 = ADVANCED_FACE ( 'NONE', ( #41370 ), #45604, .F. ) ;
#12531 = LINE ( 'NONE', #47145, #3694 ) ;
#12532 = AXIS2_PLACEMENT_3D ( 'NONE', #43333, #20876, #38198 ) ;
#12533 = EDGE_CURVE ( 'NONE', #12359, #38932, #36532, .T. ) ;
#12534 = CARTESIAN_POINT ( 'NONE',  ( -17.85867893883878565, 0.000000000000000000, 4.512100743045057705 ) ) ;
#12535 = FACE_OUTER_BOUND ( 'NONE', #16900, .T. ) ;
#12536 = EDGE_CURVE ( 'NONE', #26517, #3186, #9877, .T. ) ;
#12537 = CARTESIAN_POINT ( 'NONE',  ( -24.92324054119748311, 18.23204432365830030, 4.564397195367118520 ) ) ;
#12538 = ORIENTED_EDGE ( 'NONE', *, *, #13491, .F. ) ;
#12539 = ORIENTED_EDGE ( 'NONE', *, *, #17856, .F. ) ;
#12540 = DIRECTION ( 'NONE',  ( 0.7660212471507180654, -0.6427876096865404731, 0.005961354470445141482 ) ) ;
#12541 = DIRECTION ( 'NONE',  ( 0.7660212471507180654, -0.6427876096865404731, 0.005961354470445141482 ) ) ;
#12542 = ORIENTED_EDGE ( 'NONE', *, *, #22951, .F. ) ;
#12543 = LINE ( 'NONE', #16791, #30234 ) ;
#12544 = EDGE_CURVE ( 'NONE', #35256, #40645, #32301, .T. ) ;
#12545 = ORIENTED_EDGE ( 'NONE', *, *, #5224, .F. ) ;
#12546 = DIRECTION ( 'NONE',  ( 0.9659258262890682012, -0.2588190451025213501, 0.000000000000000000 ) ) ;
#12547 = ORIENTED_EDGE ( 'NONE', *, *, #42390, .T. ) ;
#12548 = DIRECTION ( 'NONE',  ( 0.5364919789714477361, 0.6444004775717706579, 0.5449076811759711036 ) ) ;
#12549 = EDGE_CURVE ( 'NONE', #22074, #4830, #14421, .T. ) ;
#12550 = VERTEX_POINT ( 'NONE', #49033 ) ;
#12551 = ORIENTED_EDGE ( 'NONE', *, *, #9529, .F. ) ;
#12552 = ORIENTED_EDGE ( 'NONE', *, *, #2312, .T. ) ;
#12553 = DIRECTION ( 'NONE',  ( 0.007781995580012663651, 0.000000000000000000, -0.9999697198139515519 ) ) ;
#12554 = PLANE ( 'NONE',  #13276 ) ;
#12555 = CARTESIAN_POINT ( 'NONE',  ( -11.25586126502947337, -0.1191753592594179401, 4.832814438631556797 ) ) ;
#12556 = DIRECTION ( 'NONE',  ( 0.007781995580012663651, 0.000000000000000000, -0.9999697198139515519 ) ) ;
#12557 = ORIENTED_EDGE ( 'NONE', *, *, #17194, .F. ) ;
#12558 = ORIENTED_EDGE ( 'NONE', *, *, #46702, .T. ) ;
#12559 = ORIENTED_EDGE ( 'NONE', *, *, #2563, .F. ) ;
#12560 = CARTESIAN_POINT ( 'NONE',  ( -12.52654812221797442, 3.038739411681507185, 6.734146878685358217 ) ) ;
#12561 = CARTESIAN_POINT ( 'NONE',  ( -9.489466688688677820, 0.000000000000000000, 3.838567748353698850 ) ) ;
#12562 = ORIENTED_EDGE ( 'NONE', *, *, #11519, .T. ) ;
#12563 = CARTESIAN_POINT ( 'NONE',  ( -12.91543455048469369, 4.657758921906512306, 1.550118225248739101 ) ) ;
#12564 = VERTEX_POINT ( 'NONE', #15497 ) ;
#12565 = DIRECTION ( 'NONE',  ( 0.9999697198139515519, 0.000000000000000000, 0.007781995580013368816 ) ) ;
#12566 = LINE ( 'NONE', #30455, #39430 ) ;
#12567 = VECTOR ( 'NONE', #11177, 999.9999999999998863 ) ;
#12568 = EDGE_LOOP ( 'NONE', ( #46939, #7165, #33075, #51824 ) ) ;
#12569 = FACE_OUTER_BOUND ( 'NONE', #31918, .T. ) ;
#12570 = ADVANCED_FACE ( 'NONE', ( #7267 ), #24318, .F. ) ;
#12571 = VERTEX_POINT ( 'NONE', #29120 ) ;
#12572 = CARTESIAN_POINT ( 'NONE',  ( -10.82591808402700551, -0.1941918491731536578, 1.205787872916244341 ) ) ;
#12573 = DIRECTION ( 'NONE',  ( -0.9999697198139514409, -0.000000000000000000, -0.007781995580013368816 ) ) ;
#12574 = VERTEX_POINT ( 'NONE', #55246 ) ;
#12575 = DIRECTION ( 'NONE',  ( -0.005961354470445682716, -0.6427876096865404731, 0.7660212471507180654 ) ) ;
#12576 = LINE ( 'NONE', #30468, #17552 ) ;
#12577 = FACE_OUTER_BOUND ( 'NONE', #50426, .T. ) ;
#12578 = PLANE ( 'NONE',  #136 ) ;
#12579 = EDGE_LOOP ( 'NONE', ( #984, #8749, #312, #41465 ) ) ;
#12580 = ADVANCED_FACE ( 'NONE', ( #24871 ), #50971, .F. ) ;
#12581 = PLANE ( 'NONE',  #27357 ) ;
#12582 = PLANE ( 'NONE',  #41241 ) ;
#12583 = FACE_OUTER_BOUND ( 'NONE', #554, .T. ) ;
#12584 = DIRECTION ( 'NONE',  ( -0.005002170337468016433, -0.7660444431189770143, 0.6427681459581293666 ) ) ;
#12586 = ADVANCED_FACE ( 'NONE', ( #47019 ), #15781, .F. ) ;
#12585 = PLANE ( 'NONE',  #47878 ) ;
#12587 = DIRECTION ( 'NONE',  ( 0.3313982828793700097, 0.4028455766673916805, 0.8531650599175528704 ) ) ;
#12588 = EDGE_LOOP ( 'NONE', ( #55360, #52892, #10241, #21289 ) ) ;
#12589 = CARTESIAN_POINT ( 'NONE',  ( -21.17348044452715783, -5.213152330870663320, 13.46210170089576508 ) ) ;
#12590 = FACE_OUTER_BOUND ( 'NONE', #49118, .T. ) ;
#12591 = FACE_OUTER_BOUND ( 'NONE', #54135, .T. ) ;
#12592 = ORIENTED_EDGE ( 'NONE', *, *, #19549, .T. ) ;
#12593 = CARTESIAN_POINT ( 'NONE',  ( -17.75790376729938913, -0.1191753592594196193, 4.412881970621663541 ) ) ;
#12594 = ORIENTED_EDGE ( 'NONE', *, *, #5523, .F. ) ;
#12595 = DIRECTION ( 'NONE',  ( -0.6427681459581293666, -0.7660444431189770143, -0.005002170337467561935 ) ) ;
#12596 = DIRECTION ( 'NONE',  ( -0.7660212471507179544, -0.6427876096865405842, -0.005961354470445141482 ) ) ;
#12597 = EDGE_CURVE ( 'NONE', #21470, #31183, #32823, .T. ) ;
#12598 = LINE ( 'NONE', #48061, #41397 ) ;
#12599 = EDGE_CURVE ( 'NONE', #33755, #14988, #16335, .T. ) ;
#12600 = CARTESIAN_POINT ( 'NONE',  ( -65.33958530469845982, 1.999999999999986233, 0.8132580553645364363 ) ) ;
#12601 = ORIENTED_EDGE ( 'NONE', *, *, #39939, .F. ) ;
#12602 = ORIENTED_EDGE ( 'NONE', *, *, #6549, .F. ) ;
#12603 = CARTESIAN_POINT ( 'NONE',  ( -68.18363897928762185, -0.6010854823554140358, 5.199837068550145602 ) ) ;
#12604 = DIRECTION ( 'NONE',  ( 0.6427681459581294776, -0.7660444431189769032, 0.005002170337467562802 ) ) ;
#12605 = DIRECTION ( 'NONE',  ( -0.7660212471507179544, -0.6427876096865405842, -0.005961354470445141482 ) ) ;
#12606 = LINE ( 'NONE', #29924, #13922 ) ;
#12607 = EDGE_CURVE ( 'NONE', #15806, #37866, #33126, .T. ) ;
#12608 = VECTOR ( 'NONE', #55184, 1000.000000000000227 ) ;
#12609 = PLANE ( 'NONE',  #1993 ) ;
#12610 = CARTESIAN_POINT ( 'NONE',  ( -20.35841145877394354, 0.000000000000000000, 5.231311386181617173 ) ) ;
#12611 = ORIENTED_EDGE ( 'NONE', *, *, #11355, .T. ) ;
#12612 = DIRECTION ( 'NONE',  ( 0.9999697198139515519, 0.000000000000000000, 0.007781995580013368816 ) ) ;
#12613 = EDGE_CURVE ( 'NONE', #5013, #28164, #20877, .T. ) ;
#12614 = CARTESIAN_POINT ( 'NONE',  ( -16.71693315311381767, -3.270328918600659218, 8.542523180522204385 ) ) ;
#12615 = EDGE_LOOP ( 'NONE', ( #40946, #30822, #28320, #35744 ) ) ;
#12616 = LINE ( 'NONE', #25663, #4781 ) ;
#12617 = CARTESIAN_POINT ( 'NONE',  ( -15.54124256164392293, 0.000000000000000000, 5.268799708400632831 ) ) ;
#12618 = CARTESIAN_POINT ( 'NONE',  ( -10.91056151514876049, 0.000000000000000000, 7.320823101664526433 ) ) ;
#12619 = ORIENTED_EDGE ( 'NONE', *, *, #46255, .T. ) ;
#12620 = DIRECTION ( 'NONE',  ( 0.7660212471507180654, -0.6427876096865404731, 0.005961354470445141482 ) ) ;
#12621 = ORIENTED_EDGE ( 'NONE', *, *, #48483, .T. ) ;
#12622 = ORIENTED_EDGE ( 'NONE', *, *, #43984, .F. ) ;
#12623 = VERTEX_POINT ( 'NONE', #3570 ) ;
#12624 = EDGE_LOOP ( 'NONE', ( #31781, #10248, #49327, #10229 ) ) ;
#12625 = DIRECTION ( 'NONE',  ( 0.000000000000000000, -1.000000000000000000, 0.000000000000000000 ) ) ;
#12626 = APPLICATION_CONTEXT ( 'automotive_design' ) ;
#12628 = ADVANCED_FACE ( 'NONE', ( #41891 ), #54674, .F. ) ;
#12627 = ORIENTED_EDGE ( 'NONE', *, *, #26257, .T. ) ;
#12629 = PLANE ( 'NONE',  #53974 ) ;
#12630 = ORIENTED_EDGE ( 'NONE', *, *, #34700, .F. ) ;
#12631 = LINE ( 'NONE', #3809, #5064 ) ;
#12632 = ORIENTED_EDGE ( 'NONE', *, *, #14826, .F. ) ;
#12633 = PLANE ( 'NONE',  #32852 ) ;
#12634 = EDGE_CURVE ( 'NONE', #55568, #44513, #25174, .T. ) ;
#12635 = VERTEX_POINT ( 'NONE', #55519 ) ;
#12636 = DIRECTION ( 'NONE',  ( 0.7660212471507180654, -0.6427876096865404731, 0.005961354470445141482 ) ) ;
#12637 = DIRECTION ( 'NONE',  ( 0.9999697198139515519, 0.000000000000000000, 0.007781995580013368816 ) ) ;
#12638 = EDGE_CURVE ( 'NONE', #83, #36758, #7545, .T. ) ;
#12639 = CARTESIAN_POINT ( 'NONE',  ( -15.86710544311044302, 0.000000000000000000, 13.13336954653252953 ) ) ;
#12640 = LINE ( 'NONE', #16601, #43228 ) ;
#12641 = DIRECTION ( 'NONE',  ( 0.6427681459581294776, -0.7660444431189769032, 0.005002170337467562802 ) ) ;
#12642 = ORIENTED_EDGE ( 'NONE', *, *, #22172, .F. ) ;
#12643 = ADVANCED_FACE ( 'NONE', ( #28865 ), #37940, .F. ) ;
#12644 = EDGE_CURVE ( 'NONE', #30203, #45792, #12078, .T. ) ;
#12645 = ADVANCED_FACE ( 'NONE', ( #29416 ), #7015, .F. ) ;
#12646 = VECTOR ( 'NONE', #20752, 1000.000000000000114 ) ;
#12647 = ORIENTED_EDGE ( 'NONE', *, *, #16736, .F. ) ;
#12648 = CARTESIAN_POINT ( 'NONE',  ( -13.63673279712320507, -0.1191753592594197858, 12.22739664767016521 ) ) ;
#12649 = CARTESIAN_POINT ( 'NONE',  ( -11.87243407472968926, 0.000000000000000000, 11.50246268866867361 ) ) ;
#12650 = LINE ( 'NONE', #26010, #41471 ) ;
#12651 = CYLINDRICAL_SURFACE ( 'NONE', #41209, 2.750000000000001776 ) ;
#12652 = LINE ( 'NONE', #43027, #23116 ) ;
#12653 = CARTESIAN_POINT ( 'NONE',  ( -14.01701317841955508, 0.000000000000000000, 2.326005055450897085 ) ) ;
#12654 = EDGE_LOOP ( 'NONE', ( #10622, #14090, #40823, #12258 ) ) ;
#12655 = PLANE ( 'NONE',  #40210 ) ;
#12656 = CARTESIAN_POINT ( 'NONE',  ( -16.43317633868556626, -0.1191753592594197858, 13.31363028683540151 ) ) ;
#12657 = ORIENTED_EDGE ( 'NONE', *, *, #10640, .F. ) ;
#12658 = CARTESIAN_POINT ( 'NONE',  ( -11.82702144042051984, 0.000000000000000000, 5.667036705802473762 ) ) ;
#12659 = CARTESIAN_POINT ( 'NONE',  ( -13.21362762481721020, 0.000000000000000000, 4.717575620020126870 ) ) ;
#12660 = ADVANCED_FACE ( 'NONE', ( #21165 ), #11250, .F. ) ;
#12661 = CARTESIAN_POINT ( 'NONE',  ( -22.94167088982010583, 19.41289598198349253, 4.465499946586994895 ) ) ;
#12662 = EDGE_CURVE ( 'NONE', #2262, #19938, #20033, .T. ) ;
#12663 = DIRECTION ( 'NONE',  ( -0.3313982828793700652, 0.4028455766673916250, -0.8531650599175529814 ) ) ;
#12664 = ADVANCED_FACE ( 'NONE', ( #47868 ), #12931, .F. ) ;
#12665 = EDGE_LOOP ( 'NONE', ( #15752, #37726, #25275, #44776 ) ) ;
#12666 = VERTEX_POINT ( 'NONE', #26843 ) ;
#12667 = EDGE_CURVE ( 'NONE', #38691, #32780, #30260, .T. ) ;
#12668 = CARTESIAN_POINT ( 'NONE',  ( -16.84047315302936454, -5.051250379848161387, 11.51330583538055130 ) ) ;
#12669 = CARTESIAN_POINT ( 'NONE',  ( -11.35795409095814712, 0.000000000000000000, 5.101348970349929068 ) ) ;
#12670 = CARTESIAN_POINT ( 'NONE',  ( -15.79726335400637183, 0.000000000000000000, 4.158811085975333555 ) ) ;
#12671 = EDGE_CURVE ( 'NONE', #39021, #883, #25711, .T. ) ;
#12672 = DIRECTION ( 'NONE',  ( 0.000000000000000000, -1.000000000000000000, 0.000000000000000000 ) ) ;
#12673 = DIRECTION ( 'NONE',  ( 0.5364919789714477361, 0.6444004775717706579, 0.5449076811759711036 ) ) ;
#12674 = CARTESIAN_POINT ( 'NONE',  ( -24.26986129792355129, -0.1191753592594197858, 6.208864760408702388 ) ) ;
#12675 = PLANE ( 'NONE',  #11174 ) ;
#12676 = EDGE_CURVE ( 'NONE', #12635, #12199, #8694, .T. ) ;
#12677 = VERTEX_POINT ( 'NONE', #17767 ) ;
#12678 = FACE_OUTER_BOUND ( 'NONE', #54792, .T. ) ;
#12679 = FACE_OUTER_BOUND ( 'NONE', #43523, .T. ) ;
#12680 = CARTESIAN_POINT ( 'NONE',  ( -18.67775241435682432, 0.000000000000000000, 4.136394454059623804 ) ) ;
#12681 = VERTEX_POINT ( 'NONE', #8969 ) ;
#12682 = LINE ( 'NONE', #7880, #37706 ) ;
#12683 = MECHANICAL_DESIGN_GEOMETRIC_PRESENTATION_REPRESENTATION (  '', ( #46182 ), #19000 ) ;
#12684 = VERTEX_POINT ( 'NONE', #9224 ) ;
#12685 = ORIENTED_EDGE ( 'NONE', *, *, #6546, .F. ) ;
#12686 = ORIENTED_EDGE ( 'NONE', *, *, #141, .T. ) ;
#12687 = ORIENTED_EDGE ( 'NONE', *, *, #5348, .T. ) ;
#12688 = EDGE_LOOP ( 'NONE', ( #40683, #20850, #3959, #25054 ) ) ;
#12689 = EDGE_LOOP ( 'NONE', ( #47404, #55466, #16359, #40454 ) ) ;
#12690 = CARTESIAN_POINT ( 'NONE',  ( -18.34507117752021088, 3.848249166794009746, 10.32280225099176185 ) ) ;
#12691 = LINE ( 'NONE', #39673, #7550 ) ;
#12692 = DIRECTION ( 'NONE',  ( 0.007781995580012662783, 0.000000000000000000, -0.9999697198139514409 ) ) ;
#12693 = ORIENTED_EDGE ( 'NONE', *, *, #45271, .T. ) ;
#12694 = CARTESIAN_POINT ( 'NONE',  ( -14.20280369269832832, 0.000000000000000000, 12.40765738797303719 ) ) ;
#12695 = ORIENTED_EDGE ( 'NONE', *, *, #18408, .F. ) ;
#12696 = CARTESIAN_POINT ( 'NONE',  ( -66.39152944734560435, -11.32110184138706721, -6.891906871564133397 ) ) ;
#12697 = ORIENTED_EDGE ( 'NONE', *, *, #52905, .T. ) ;
#12698 = CARTESIAN_POINT ( 'NONE',  ( -19.59569683186026268, 0.000000000000000000, 14.58168106541950948 ) ) ;
#12699 = CARTESIAN_POINT ( 'NONE',  ( -20.18761906488554914, -0.7980104508677885455, 5.671006189966389499 ) ) ;
#12700 = CARTESIAN_POINT ( 'NONE',  ( -17.34043131654819092, 1.581621852479005552, 6.212644435970458900 ) ) ;
#12701 = ORIENTED_EDGE ( 'NONE', *, *, #9911, .T. ) ;
#12702 = CARTESIAN_POINT ( 'NONE',  ( -27.99923088623136636, 0.000000000000000000, 7.757173251277078130 ) ) ;
#12703 = ORIENTED_EDGE ( 'NONE', *, *, #5500, .T. ) ;
#12704 = EDGE_CURVE ( 'NONE', #27150, #39340, #122, .T. ) ;
#12705 = ADVANCED_FACE ( 'NONE', ( #52110 ), #55979, .T. ) ;
#12706 = DIRECTION ( 'NONE',  ( -0.6427681459581293666, -0.7660444431189770143, -0.005002170337467561935 ) ) ;
#12707 = CARTESIAN_POINT ( 'NONE',  ( -18.67619601524082285, 0.000000000000000000, 3.936400510096834893 ) ) ;
#12708 = EDGE_CURVE ( 'NONE', #46096, #37185, #52404, .T. ) ;
#12709 = VECTOR ( 'NONE', #14637, 1000.000000000000227 ) ;
#12710 = DIRECTION ( 'NONE',  ( 0.007781995580012662783, 0.000000000000000000, -0.9999697198139514409 ) ) ;
#12711 = PLANE ( 'NONE',  #46720 ) ;
#12712 = PLANE ( 'NONE',  #6618 ) ;
#12713 = CARTESIAN_POINT ( 'NONE',  ( -68.13729736978412177, -4.474875060344467114E-15, -7.461798308327053597 ) ) ;
#12714 = LINE ( 'NONE', #47341, #34809 ) ;
#12715 = PLANE ( 'NONE',  #41337 ) ;
#12716 = EDGE_LOOP ( 'NONE', ( #15741, #32594, #8936, #28617 ) ) ;
#12717 = CARTESIAN_POINT ( 'NONE',  ( -56.40927410319390134, 6.683688692736960313, -2.245073662639579304 ) ) ;
#12718 = VERTEX_POINT ( 'NONE', #26272 ) ;
#12719 = CARTESIAN_POINT ( 'NONE',  ( -14.01545677930355183, 0.000000000000000000, 2.126011111488108174 ) ) ;
#12720 = LINE ( 'NONE', #12463, #11466 ) ;
#12721 = CARTESIAN_POINT ( 'NONE',  ( -16.06709938707323460, 0.000000000000000000, 13.13181314741652628 ) ) ;
#12722 = CARTESIAN_POINT ( 'NONE',  ( -23.33693525117809386, 0.000000000000000000, 5.746789908705562944 ) ) ;
#12723 = DIRECTION ( 'NONE',  ( 0.7660212471507180654, -0.6427876096865404731, 0.005961354470445141482 ) ) ;
#12724 = DIRECTION ( 'NONE',  ( -0.9321478471874540261, 0.000000000000000000, 0.3620778797217457656 ) ) ;
#12725 = LINE ( 'NONE', #8189, #35580 ) ;
#12726 = SHAPE_DEFINITION_REPRESENTATION ( #6089, #55389 ) ;
#12727 = VERTEX_POINT ( 'NONE', #4430 ) ;
#12728 = CARTESIAN_POINT ( 'NONE',  ( -23.33693525117809386, 0.000000000000000000, 5.746789908705562944 ) ) ;
#12729 = CARTESIAN_POINT ( 'NONE',  ( -18.29747203306047609, -0.1191753592594177458, 14.03778604627889059 ) ) ;
#12730 = CARTESIAN_POINT ( 'NONE',  ( -16.79925329029790149, 0.000000000000000000, 13.49544742625427496 ) ) ;
#12731 = EDGE_CURVE ( 'NONE', #17974, #54313, #48407, .T. ) ;
#12732 = CARTESIAN_POINT ( 'NONE',  ( -20.54126990917373874, 0.000000000000000000, 4.760553241521714440 ) ) ;
#12733 = DIRECTION ( 'NONE',  ( -0.000000000000000000, 1.000000000000000000, -0.000000000000000000 ) ) ;
#12734 = EDGE_CURVE ( 'NONE', #8596, #19207, #22309, .T. ) ;
#12735 = CARTESIAN_POINT ( 'NONE',  ( -8.846271876811060864, 0.000000000000000000, 6.598223741337037040 ) ) ;
#12736 = CARTESIAN_POINT ( 'NONE',  ( -24.27063949748155380, 0.000000000000000000, 6.308861732390097288 ) ) ;
#12737 = VERTEX_POINT ( 'NONE', #51563 ) ;
#12738 = CARTESIAN_POINT ( 'NONE',  ( -30.79567442779373110, 0.000000000000000000, 8.843406890442315316 ) ) ;
#12739 = DIRECTION ( 'NONE',  ( 0.000000000000000000, -1.000000000000000000, 0.000000000000000000 ) ) ;
#12740 = ORIENTED_EDGE ( 'NONE', *, *, #55088, .F. ) ;
#12741 = EDGE_CURVE ( 'NONE', #21963, #30486, #43334, .T. ) ;
#12742 = EDGE_LOOP ( 'NONE', ( #22355, #9484, #7046, #24675 ) ) ;
#12743 = CARTESIAN_POINT ( 'NONE',  ( 2.072287782118878319, 0.000000000000000000, -2.950529333540147015 ) ) ;
#12744 = EDGE_CURVE ( 'NONE', #38231, #14055, #55819, .T. ) ;
#12745 = ORIENTED_EDGE ( 'NONE', *, *, #37662, .F. ) ;
#12746 = ADVANCED_FACE ( 'NONE', ( #35103 ), #43865, .F. ) ;
#12747 = VECTOR ( 'NONE', #20034, 1000.000000000000227 ) ;
#12748 = ORIENTED_EDGE ( 'NONE', *, *, #38213, .T. ) ;
#12749 = ORIENTED_EDGE ( 'NONE', *, *, #44255, .T. ) ;
#12750 = VERTEX_POINT ( 'NONE', #38793 ) ;
#12751 = CARTESIAN_POINT ( 'NONE',  ( -13.08486533123210194, 0.000000000000000000, 1.963927175729152541 ) ) ;
#12752 = ORIENTED_EDGE ( 'NONE', *, *, #11789, .T. ) ;
#12753 = FACE_OUTER_BOUND ( 'NONE', #23953, .T. ) ;
#12754 = LINE ( 'NONE', #24404, #18557 ) ;
#12755 = VERTEX_POINT ( 'NONE', #4689 ) ;
#12756 = ORIENTED_EDGE ( 'NONE', *, *, #19225, .T. ) ;
#12757 = LINE ( 'NONE', #52497, #37512 ) ;
#12758 = ORIENTED_EDGE ( 'NONE', *, *, #50347, .F. ) ;
#12759 = CARTESIAN_POINT ( 'NONE',  ( -12.15271748404464880, 0.000000000000000000, 1.601849296007406664 ) ) ;
#12760 = LINE ( 'NONE', #42580, #5039 ) ;
#12761 = ORIENTED_EDGE ( 'NONE', *, *, #48405, .T. ) ;
#12762 = LINE ( 'NONE', #21586, #22064 ) ;
#12764 = ORIENTED_EDGE ( 'NONE', *, *, #9959, .T. ) ;
#12763 = EDGE_CURVE ( 'NONE', #40825, #41994, #16932, .T. ) ;
#12765 = VECTOR ( 'NONE', #41182, 1000.000000000000227 ) ;
#12766 = PLANE ( 'NONE',  #41810 ) ;
#12767 = ADVANCED_FACE ( 'NONE', ( #39052 ), #34794, .F. ) ;
#12768 = EDGE_CURVE ( 'NONE', #21349, #22899, #35358, .T. ) ;
#12769 = CARTESIAN_POINT ( 'NONE',  ( -17.74482636761137044, -0.1191753592594197858, 3.674319602356483916 ) ) ;
#12770 = ORIENTED_EDGE ( 'NONE', *, *, #55046, .F. ) ;
#12771 = DIRECTION ( 'NONE',  ( 0.7660212471507180654, -0.6427876096865404731, 0.005961354470445141482 ) ) ;
#12772 = CARTESIAN_POINT ( 'NONE',  ( -12.13851405436063047, 0.000000000000000000, 11.68505802764555135 ) ) ;
#12773 = CARTESIAN_POINT ( 'NONE',  ( -21.10098843074258923, -2.946525016555658016, 9.714021765596209335 ) ) ;
#12774 = CARTESIAN_POINT ( 'NONE',  ( -8.828121567967061267, 0.000000000000000000, 4.265948033562787955 ) ) ;
#12775 = VERTEX_POINT ( 'NONE', #12659 ) ;
#12776 = AXIS2_PLACEMENT_3D ( 'NONE', #42019, #46021, #24423 ) ;
#12777 = DIRECTION ( 'NONE',  ( 0.007781995580012663651, -3.146120232559066537E-19, -0.9999697198139514409 ) ) ;
#12778 = DIRECTION ( 'NONE',  ( -0.005961354470445682716, -0.6427876096865404731, 0.7660212471507180654 ) ) ;
#12779 = PLANE ( 'NONE',  #44855 ) ;
#12780 = PLANE ( 'NONE',  #41387 ) ;
#12781 = LINE ( 'NONE', #47417, #35033 ) ;
#12782 = CARTESIAN_POINT ( 'NONE',  ( -15.34256627207041390, 0.000000000000000000, 5.439671866811612411 ) ) ;
#12783 = DIRECTION ( 'NONE',  ( 0.6427681459581294776, -0.7660444431189769032, 0.005002170337467562802 ) ) ;
#12784 = EDGE_CURVE ( 'NONE', #21737, #26746, #29975, .T. ) ;
#12785 = VECTOR ( 'NONE', #25501, 1000.000000000000227 ) ;
#12786 = LINE ( 'NONE', #4547, #3923 ) ;
#12787 = DIRECTION ( 'NONE',  ( 0.5364919789714477361, 0.6444004775717706579, 0.5449076811759711036 ) ) ;
#12788 = ORIENTED_EDGE ( 'NONE', *, *, #33158, .F. ) ;
#12789 = CARTESIAN_POINT ( 'NONE',  ( -67.68550200468050093, 4.300705092652487184E-12, 5.522897687430759817 ) ) ;
#12790 = ORIENTED_EDGE ( 'NONE', *, *, #25608, .T. ) ;
#12791 = LINE ( 'NONE', #29848, #8433 ) ;
#12792 = FACE_OUTER_BOUND ( 'NONE', #20434, .T. ) ;
#12793 = B_SPLINE_CURVE_WITH_KNOTS ( 'NONE', 3,
 ( #20930, #12713, #38255, #42533, #24935, #16688 ),
 .UNSPECIFIED., .F., .F.,
 ( 4, 2, 4 ),
 ( 1.406724837889273990E-17, 0.0009531277170912122671, 0.001906255434182410440 ),
 .UNSPECIFIED. ) ;
#12794 = LINE ( 'NONE', #30117, #15507 ) ;
#12795 = EDGE_CURVE ( 'NONE', #38515, #17105, #49245, .T. ) ;
#12796 = CARTESIAN_POINT ( 'NONE',  ( -10.70062775628084495, 0.000000000000000000, 6.045134631712261175 ) ) ;
#12797 = DIRECTION ( 'NONE',  ( 0.5364919789714477361, 0.6444004775717706579, 0.5449076811759711036 ) ) ;
#12798 = ORIENTED_EDGE ( 'NONE', *, *, #14701, .F. ) ;
#12799 = ORIENTED_EDGE ( 'NONE', *, *, #53807, .T. ) ;
#12800 = DIRECTION ( 'NONE',  ( 0.6427681459581294776, -0.7660444431189769032, 0.005002170337467562802 ) ) ;
#12801 = DIRECTION ( 'NONE',  ( 0.005961354470445682716, -0.6427876096865404731, -0.7660212471507180654 ) ) ;
#12802 = ORIENTED_EDGE ( 'NONE', *, *, #26576, .F. ) ;
#12803 = PLANE ( 'NONE',  #32933 ) ;
#12804 = VECTOR ( 'NONE', #52271, 1000.000000000000227 ) ;
#12805 = VECTOR ( 'NONE', #22126, 1000.000000000000227 ) ;
#12806 = ORIENTED_EDGE ( 'NONE', *, *, #6944, .T. ) ;
#12807 = DIRECTION ( 'NONE',  ( -0.7660212471507179544, -0.6427876096865405842, -0.005961354470445141482 ) ) ;
#12808 = ADVANCED_FACE ( 'NONE', ( #27118 ), #22582, .F. ) ;
#12809 = VERTEX_POINT ( 'NONE', #27681 ) ;
#12810 = DIRECTION ( 'NONE',  ( 0.5449076811759707706, 0.6444004775717708799, -0.5364919789714476250 ) ) ;
#12811 = ORIENTED_EDGE ( 'NONE', *, *, #51082, .T. ) ;
#12812 = EDGE_LOOP ( 'NONE', ( #26808, #32387, #55816, #51381 ) ) ;
#12813 = ORIENTED_EDGE ( 'NONE', *, *, #17369, .T. ) ;
#12814 = CARTESIAN_POINT ( 'NONE',  ( -22.40478740399063895, 0.000000000000000000, 5.384712028983816623 ) ) ;
#12815 = DIRECTION ( 'NONE',  ( -0.005961354470445682716, -0.6427876096865404731, 0.7660212471507180654 ) ) ;
#12816 = CARTESIAN_POINT ( 'NONE',  ( -15.50102849149811135, -0.1191753592594197858, 12.95155240711365430 ) ) ;
#12817 = ADVANCED_FACE ( 'NONE', ( #32223 ), #53261, .F. ) ;
#12818 = CARTESIAN_POINT ( 'NONE',  ( -16.11251725036584048, -3.108426967578159061, 8.042038833893970562 ) ) ;
#12819 = ORIENTED_EDGE ( 'NONE', *, *, #34482, .F. ) ;
#12820 = EDGE_LOOP ( 'NONE', ( #45005, #33824, #47047, #41399 ) ) ;
#12821 = EDGE_CURVE ( 'NONE', #39352, #37185, #14607, .T. ) ;
#12822 = EDGE_CURVE ( 'NONE', #28898, #52574, #52949, .T. ) ;
#12823 = VECTOR ( 'NONE', #40353, 999.9999999999998863 ) ;
#12824 = ORIENTED_EDGE ( 'NONE', *, *, #5529, .T. ) ;
#12825 = DIRECTION ( 'NONE',  ( 0.000000000000000000, -0.000000000000000000, -1.000000000000000000 ) ) ;
#12826 = ORIENTED_EDGE ( 'NONE', *, *, #14952, .F. ) ;
#12827 = DIRECTION ( 'NONE',  ( 0.000000000000000000, 0.000000000000000000, 1.000000000000000000 ) ) ;
#12828 = EDGE_CURVE ( 'NONE', #54772, #12635, #2085, .T. ) ;
#12829 = ORIENTED_EDGE ( 'NONE', *, *, #21989, .F. ) ;
#12830 = PLANE ( 'NONE',  #6081 ) ;
#12831 = LINE ( 'NONE', #30153, #19470 ) ;
#12832 = VERTEX_POINT ( 'NONE', #19419 ) ;
#12833 = ADVANCED_FACE ( 'NONE', ( #23426 ), #36207, .F. ) ;
#12834 = DIRECTION ( 'NONE',  ( 0.005961354470445682716, -0.6427876096865404731, -0.7660212471507180654 ) ) ;
#12835 = ORIENTED_EDGE ( 'NONE', *, *, #49629, .F. ) ;
#12836 = EDGE_CURVE ( 'NONE', #25142, #26953, #35635, .T. ) ;
#12837 = DIRECTION ( 'NONE',  ( -0.005961354470445682716, -0.6427876096865404731, 0.7660212471507180654 ) ) ;
#12838 = ORIENTED_EDGE ( 'NONE', *, *, #26190, .F. ) ;
#12839 = DIRECTION ( 'NONE',  ( 0.9999697198139515519, 0.000000000000000000, 0.007781995580013368816 ) ) ;
#12840 = CARTESIAN_POINT ( 'NONE',  ( -17.93139508144814442, 0.000000000000000000, 13.85596890686001537 ) ) ;
#12841 = DIRECTION ( 'NONE',  ( 0.007781995580012663651, 0.000000000000000000, -0.9999697198139515519 ) ) ;
#12842 = VERTEX_POINT ( 'NONE', #10906 ) ;
#12843 = ADVANCED_FACE ( 'NONE', ( #45529 ), #40742, .F. ) ;
#12845 = CARTESIAN_POINT ( 'NONE',  ( -11.89954417724882774, 0.000000000000000000, 1.403813493000912294 ) ) ;
#12844 = VECTOR ( 'NONE', #46439, 1000.000000000000114 ) ;
#12846 = VECTOR ( 'NONE', #53428, 1000.000000000000227 ) ;
#12847 = EDGE_CURVE ( 'NONE', #52707, #27319, #10067, .T. ) ;
#12848 = DIRECTION ( 'NONE',  ( 0.000000000000000000, -0.000000000000000000, -1.000000000000000000 ) ) ;
#12849 = CARTESIAN_POINT ( 'NONE',  ( -18.58795878855817207, 0.000000000000000000, 4.506425318625041143 ) ) ;
#12850 = LINE ( 'NONE', #47490, #28602 ) ;
#12851 = DIRECTION ( 'NONE',  ( 0.007781995580012662783, 0.000000000000000000, -0.9999697198139514409 ) ) ;
#12852 = DIRECTION ( 'NONE',  ( 0.7660212471507180654, -0.6427876096865404731, 0.005961354470445141482 ) ) ;
#12853 = EDGE_CURVE ( 'NONE', #3505, #25279, #971, .T. ) ;
#12854 = CARTESIAN_POINT ( 'NONE',  ( -19.69569380384165669, -0.1191753592594177458, 14.58090286586150697 ) ) ;
#12855 = VECTOR ( 'NONE', #51738, 1000.000000000000114 ) ;
#12856 = ORIENTED_EDGE ( 'NONE', *, *, #9923, .F. ) ;
#12857 = DIRECTION ( 'NONE',  ( -0.000000000000000000, -1.000000000000000000, -0.000000000000000000 ) ) ;
#12858 = DIRECTION ( 'NONE',  ( 0.007781995580012663651, -3.146120232559066537E-19, -0.9999697198139514409 ) ) ;
#12859 = LINE ( 'NONE', #51200, #27770 ) ;
#12860 = EDGE_LOOP ( 'NONE', ( #14671, #10465, #18249 ) ) ;
#12861 = CARTESIAN_POINT ( 'NONE',  ( -20.01569662516219239, -4.403642575758160760, 11.68383572719809216 ) ) ;
#12862 = CARTESIAN_POINT ( 'NONE',  ( -13.62236162558936847, -0.1941918491731548790, 2.292021512081481305 ) ) ;
#12863 = VERTEX_POINT ( 'NONE', #19135 ) ;
#12864 = CARTESIAN_POINT ( 'NONE',  ( -16.33317936670417225, 0.000000000000000000, 13.31440848639340224 ) ) ;
#12865 = CARTESIAN_POINT ( 'NONE',  ( -12.13851405436063047, 0.000000000000000000, 11.68505802764555135 ) ) ;
#12866 = FACE_OUTER_BOUND ( 'NONE', #54438, .T. ) ;
#12867 = VECTOR ( 'NONE', #44143, 1000.000000000000227 ) ;
#12868 = CARTESIAN_POINT ( 'NONE',  ( -69.43683623637159030, 1.999999999998648192, -6.967005367353809042 ) ) ;
#12869 = ORIENTED_EDGE ( 'NONE', *, *, #14509, .T. ) ;
#12870 = VERTEX_POINT ( 'NONE', #14060 ) ;
#12871 = CARTESIAN_POINT ( 'NONE',  ( -16.81345671998191449, 0.000000000000000000, 3.412238694616132495 ) ) ;
#12872 = LINE ( 'NONE', #26220, #5993 ) ;
#12873 = PLANE ( 'NONE',  #33362 ) ;
#12874 = DIRECTION ( 'NONE',  ( 0.000000000000000000, -0.000000000000000000, -1.000000000000000000 ) ) ;
#12875 = LINE ( 'NONE', #8923, #6557 ) ;
#12876 = FACE_OUTER_BOUND ( 'NONE', #40045, .T. ) ;
#12877 = EDGE_CURVE ( 'NONE', #23301, #20373, #40166, .T. ) ;
#12878 = VERTEX_POINT ( 'NONE', #35944 ) ;
#12879 = DIRECTION ( 'NONE',  ( 0.000000000000000000, -0.000000000000000000, -1.000000000000000000 ) ) ;
#12880 = DIRECTION ( 'NONE',  ( -0.005002170337468016433, -0.7660444431189770143, 0.6427681459581293666 ) ) ;
#12881 = EDGE_LOOP ( 'NONE', ( #4567, #54110, #42295, #7108 ) ) ;
#12882 = DIRECTION ( 'NONE',  ( 0.007781995580012663651, 0.000000000000000000, -0.9999697198139515519 ) ) ;
#12883 = DIRECTION ( 'NONE',  ( -0.5449076811759708816, 0.6444004775717707689, 0.5364919789714475140 ) ) ;
#12884 = CARTESIAN_POINT ( 'NONE',  ( -19.60834386242827776, 0.000000000000000000, 4.298478389818581213 ) ) ;
#12885 = EDGE_CURVE ( 'NONE', #54227, #41918, #7021, .T. ) ;
#12886 = EDGE_LOOP ( 'NONE', ( #37417, #3445, #2703, #39308 ) ) ;
#12887 = VECTOR ( 'NONE', #42293, 1000.000000000000227 ) ;
#12888 = VECTOR ( 'NONE', #11662, 999.9999999999998863 ) ;
#12889 = LINE ( 'NONE', #21703, #1263 ) ;
#12890 = ORIENTED_EDGE ( 'NONE', *, *, #31640, .T. ) ;
#12891 = ADVANCED_FACE ( 'NONE', ( #27968 ), #36460, .F. ) ;
#12892 = ORIENTED_EDGE ( 'NONE', *, *, #45533, .F. ) ;
#12893 = ORIENTED_EDGE ( 'NONE', *, *, #32056, .F. ) ;
#12894 = AXIS2_PLACEMENT_3D ( 'NONE', #35768, #18150, #40302 ) ;
#12895 = ORIENTED_EDGE ( 'NONE', *, *, #51380, .F. ) ;
#12896 = CARTESIAN_POINT ( 'NONE',  ( -13.19219159589095192, 0.000000000000000000, 1.963091937920801833 ) ) ;
#12897 = ORIENTED_EDGE ( 'NONE', *, *, #1134, .F. ) ;
#12898 = DIRECTION ( 'NONE',  ( -0.5364919789714478471, 0.6444004775717705469, -0.5449076811759709926 ) ) ;
#12899 = EDGE_LOOP ( 'NONE', ( #37467, #45008, #8228, #10418 ) ) ;
#12900 = FACE_OUTER_BOUND ( 'NONE', #38587, .T. ) ;
#12901 = EDGE_CURVE ( 'NONE', #21477, #12052, #9814, .T. ) ;
#12902 = ORIENTED_EDGE ( 'NONE', *, *, #35255, .T. ) ;
#12904 = VECTOR ( 'NONE', #10756, 1000.000000000000227 ) ;
#12903 = CARTESIAN_POINT ( 'NONE',  ( -69.59775774058348929, -0.6007421665236040154, 7.493101075386322307 ) ) ;
#12905 = VERTEX_POINT ( 'NONE', #18889 ) ;
#12906 = EDGE_CURVE ( 'NONE', #11836, #45158, #45820, .T. ) ;
#12907 = CARTESIAN_POINT ( 'NONE',  ( -9.442067484779661513, -0.1191753592594197858, 10.59804618892231254 ) ) ;
#12908 = LINE ( 'NONE', #4408, #4925 ) ;
#12909 = CARTESIAN_POINT ( 'NONE',  ( -23.33693525117809386, 0.000000000000000000, 5.746789908705562944 ) ) ;
#12910 = PLANE ( 'NONE',  #26004 ) ;
#12911 = FACE_OUTER_BOUND ( 'NONE', #10221, .T. ) ;
#12912 = ORIENTED_EDGE ( 'NONE', *, *, #55113, .F. ) ;
#12913 = EDGE_CURVE ( 'NONE', #23729, #11761, #15433, .T. ) ;
#12914 = ORIENTED_EDGE ( 'NONE', *, *, #44745, .T. ) ;
#12915 = CARTESIAN_POINT ( 'NONE',  ( -14.39892221086183000, 0.000000000000000000, 3.600355174058808672 ) ) ;
#12916 = DIRECTION ( 'NONE',  ( 0.5449076811759707706, 0.6444004775717708799, -0.5364919789714476250 ) ) ;
#12917 = AXIS2_PLACEMENT_3D ( 'NONE', #7213, #10909, #24263 ) ;
#12918 = CARTESIAN_POINT ( 'NONE',  ( -15.03495456790438389, -0.1191753592594197858, 12.77051346725278158 ) ) ;
#12919 = EDGE_CURVE ( 'NONE', #3230, #37945, #20557, .T. ) ;
#12920 = LINE ( 'NONE', #21731, #45736 ) ;
#12921 = DIRECTION ( 'NONE',  ( 0.000000000000000000, -0.000000000000000000, -1.000000000000000000 ) ) ;
#12922 = FACE_OUTER_BOUND ( 'NONE', #11954, .T. ) ;
#12923 = EDGE_LOOP ( 'NONE', ( #52677, #20716, #37591, #27093 ) ) ;
#12925 = CARTESIAN_POINT ( 'NONE',  ( -19.60990026154428278, 0.000000000000000000, 4.498472333781370125 ) ) ;
#12924 = VECTOR ( 'NONE', #17408, 1000.000000000000227 ) ;
#12926 = CARTESIAN_POINT ( 'NONE',  ( -15.81738172854334934, 0.000000000000000000, 6.743979008779684037 ) ) ;
#12927 = EDGE_LOOP ( 'NONE', ( #46191, #49951, #43598, #39911 ) ) ;
#12928 = VECTOR ( 'NONE', #31175, 999.9999999999998863 ) ;
#12929 = VECTOR ( 'NONE', #28410, 1000.000000000000114 ) ;
#12930 = DIRECTION ( 'NONE',  ( -0.7660212471507179544, -0.6427876096865405842, -0.005961354470445141482 ) ) ;
#12931 = PLANE ( 'NONE',  #40551 ) ;
#12932 = LINE ( 'NONE', #51284, #52213 ) ;
#12933 = FACE_OUTER_BOUND ( 'NONE', #39044, .T. ) ;
#12934 = ORIENTED_EDGE ( 'NONE', *, *, #28869, .F. ) ;
#12935 = AXIS2_PLACEMENT_3D ( 'NONE', #26567, #22332, #26865 ) ;
#12936 = AXIS2_PLACEMENT_3D ( 'NONE', #7077, #55053, #28925 ) ;
#12937 = ORIENTED_EDGE ( 'NONE', *, *, #37714, .F. ) ;
#12938 = DIRECTION ( 'NONE',  ( 0.007781995580012663651, -3.146120232559066537E-19, -0.9999697198139514409 ) ) ;
#12939 = DIRECTION ( 'NONE',  ( 0.007781995580012663651, 0.000000000000000000, -0.9999697198139515519 ) ) ;
#12940 = DIRECTION ( 'NONE',  ( 0.000000000000000000, -1.000000000000000000, 0.000000000000000000 ) ) ;
#12941 = DIRECTION ( 'NONE',  ( -0.005002170337468016433, -0.7660444431189770143, 0.6427681459581293666 ) ) ;
#12942 = VECTOR ( 'NONE', #14037, 999.9999999999998863 ) ;
#12943 = CARTESIAN_POINT ( 'NONE',  ( -14.94760462649100496, 0.000000000000000000, 2.488088991209854051 ) ) ;
#12944 = EDGE_CURVE ( 'NONE', #41786, #1716, #6649, .T. ) ;
#12945 = LINE ( 'NONE', #43052, #34606 ) ;
#12946 = PLANE ( 'NONE',  #21145 ) ;
#12947 = ORIENTED_EDGE ( 'NONE', *, *, #32980, .T. ) ;
#12948 = DIRECTION ( 'NONE',  ( 0.9999697198139515519, 0.000000000000000000, 0.007781995580013368816 ) ) ;
#12949 = CARTESIAN_POINT ( 'NONE',  ( -17.67437291679169320, 0.000000000000000000, 6.529521417744858169 ) ) ;
#12950 = EDGE_CURVE ( 'NONE', #29873, #46828, #38135, .T. ) ;
#12951 = EDGE_CURVE ( 'NONE', #34537, #35206, #42418, .T. ) ;
#12952 = ORIENTED_EDGE ( 'NONE', *, *, #5787, .T. ) ;
#12953 = DIRECTION ( 'NONE',  ( 0.5364919789714477361, 0.6444004775717706579, 0.5449076811759711036 ) ) ;
#12954 = ORIENTED_EDGE ( 'NONE', *, *, #34145, .T. ) ;
#12955 = CARTESIAN_POINT ( 'NONE',  ( -17.38641064682997595, 0.000000000000000000, 3.535098764555870243 ) ) ;
#12956 = EDGE_CURVE ( 'NONE', #40957, #33373, #46658, .T. ) ;
#12957 = VECTOR ( 'NONE', #34293, 1000.000000000000227 ) ;
#12958 = EDGE_CURVE ( 'NONE', #41874, #35444, #12318, .T. ) ;
#12959 = ADVANCED_FACE ( 'NONE', ( #11178 ), #37583, .F. ) ;
#12960 = ORIENTED_EDGE ( 'NONE', *, *, #43699, .F. ) ;
#12961 = AXIS2_PLACEMENT_3D ( 'NONE', #34389, #7997, #11684 ) ;
#12962 = ORIENTED_EDGE ( 'NONE', *, *, #33353, .F. ) ;
#12963 = ORIENTED_EDGE ( 'NONE', *, *, #331, .F. ) ;
#12964 = VERTEX_POINT ( 'NONE', #37291 ) ;
#12965 = EDGE_LOOP ( 'NONE', ( #22878, #54116, #33746, #54474, #19413, #6689 ) ) ;
#12966 = ORIENTED_EDGE ( 'NONE', *, *, #38667, .T. ) ;
#12967 = VECTOR ( 'NONE', #21338, 1000.000000000000227 ) ;
#12968 = DIRECTION ( 'NONE',  ( -0.5364919789714478471, 0.6444004775717705469, -0.5449076811759709926 ) ) ;
#12969 = LINE ( 'NONE', #26583, #54679 ) ;
#12970 = DIRECTION ( 'NONE',  ( -0.005961354470445682716, -0.6427876096865404731, 0.7660212471507180654 ) ) ;
#12971 = AXIS2_PLACEMENT_3D ( 'NONE', #9729, #22503, #51736 ) ;
#12972 = VECTOR ( 'NONE', #10718, 1000.000000000000114 ) ;
#12973 = ORIENTED_EDGE ( 'NONE', *, *, #21623, .T. ) ;
#12974 = LINE ( 'NONE', #47317, #16801 ) ;
#12975 = ADVANCED_FACE ( 'NONE', ( #33048 ), #50062, .F. ) ;
#12976 = EDGE_LOOP ( 'NONE', ( #5557, #9875, #18120, #34310 ) ) ;
#12977 = ORIENTED_EDGE ( 'NONE', *, *, #5821, .F. ) ;
#12978 = EDGE_CURVE ( 'NONE', #45114, #18340, #54909, .T. ) ;
#12979 = VECTOR ( 'NONE', #12953, 999.9999999999998863 ) ;
#12980 = AXIS2_PLACEMENT_3D ( 'NONE', #51429, #30112, #17319 ) ;
#12981 = PLANE ( 'NONE',  #44813 ) ;
#12982 = EDGE_CURVE ( 'NONE', #14805, #37070, #55185, .T. ) ;
#12983 = CARTESIAN_POINT ( 'NONE',  ( -23.33693525117809386, 0.000000000000000000, 5.746789908705562944 ) ) ;
#12984 = ORIENTED_EDGE ( 'NONE', *, *, #36623, .T. ) ;
#12985 = DIRECTION ( 'NONE',  ( 0.007781995580012662783, 0.000000000000000000, -0.9999697198139514409 ) ) ;
#12986 = ORIENTED_EDGE ( 'NONE', *, *, #8540, .T. ) ;
#12987 = EDGE_CURVE ( 'NONE', #29855, #15218, #50367, .T. ) ;
#12988 = DIRECTION ( 'NONE',  ( 0.5364919789714477361, 0.6444004775717706579, 0.5449076811759711036 ) ) ;
#12989 = VECTOR ( 'NONE', #44286, 1000.000000000000000 ) ;
#12990 = PLANE ( 'NONE',  #35706 ) ;
#12991 = VECTOR ( 'NONE', #50738, 999.9999999999998863 ) ;
#12992 = DIRECTION ( 'NONE',  ( -0.9999697198139514409, -0.000000000000000000, -0.007781995580013368816 ) ) ;
#12993 = LINE ( 'NONE', #47638, #21350 ) ;
#12994 = LINE ( 'NONE', #47639, #48310 ) ;
#12995 = CARTESIAN_POINT ( 'NONE',  ( -17.85424848621750016, 0.000000000000000000, 3.942797095824502662 ) ) ;
#12996 = CARTESIAN_POINT ( 'NONE',  ( -19.02484223489273063, 0.2864062442990042978, 4.062688683190644134 ) ) ;
#12997 = DIRECTION ( 'NONE',  ( 0.007781995580012662783, 0.000000000000000000, -0.9999697198139514409 ) ) ;
#12998 = VERTEX_POINT ( 'NONE', #54342 ) ;
#12999 = DIRECTION ( 'NONE',  ( 0.5449076811759707706, 0.6444004775717708799, -0.5364919789714476250 ) ) ;
#13000 = VECTOR ( 'NONE', #42089, 999.9999999999998863 ) ;
#13001 = PLANE ( 'NONE',  #15627 ) ;
#13002 = DIRECTION ( 'NONE',  ( -0.005961354470445682716, -0.6427876096865404731, 0.7660212471507180654 ) ) ;
#13003 = CARTESIAN_POINT ( 'NONE',  ( -14.36939978893929570, 0.2864062442990022439, 2.932925422388083181 ) ) ;
#13004 = VECTOR ( 'NONE', #54538, 999.9999999999998863 ) ;
#13005 = CARTESIAN_POINT ( 'NONE',  ( -12.76779144812382327, 0.000000000000000000, 7.137043695297512258 ) ) ;
#13006 = LINE ( 'NONE', #7926, #41308 ) ;
#13007 = LINE ( 'NONE', #26620, #28670 ) ;
#13008 = DIRECTION ( 'NONE',  ( -0.005961354470445682716, -0.6427876096865404731, 0.7660212471507180654 ) ) ;
#13009 = PRODUCT_CONTEXT ( 'NONE', #9746, 'mechanical' ) ;
#13010 = ORIENTED_EDGE ( 'NONE', *, *, #24384, .F. ) ;
#13011 = AXIS2_PLACEMENT_3D ( 'NONE', #42438, #3530, #21118 ) ;
#13012 = PLANE ( 'NONE',  #10306 ) ;
#13013 = DIRECTION ( 'NONE',  ( -0.5364919789714478471, 0.6444004775717705469, -0.5449076811759709926 ) ) ;
#13014 = DIRECTION ( 'NONE',  ( 0.9999697198139515519, 0.000000000000000000, 0.007781995580013368816 ) ) ;
#13015 = VECTOR ( 'NONE', #35916, 1000.000000000000114 ) ;
#13016 = VECTOR ( 'NONE', #11472, 999.9999999999998863 ) ;
#13017 = DIRECTION ( 'NONE',  ( -1.000000000000000000, 0.000000000000000000, 0.000000000000000000 ) ) ;
#13018 = CARTESIAN_POINT ( 'NONE',  ( -14.59759850043533724, 0.000000000000000000, 3.429483015647829092 ) ) ;
#13019 = DIRECTION ( 'NONE',  ( -0.9999697198139514409, -0.000000000000000000, -0.007781995580013368816 ) ) ;
#13020 = LINE ( 'NONE', #39131, #54611 ) ;
#13021 = AXIS2_PLACEMENT_3D ( 'NONE', #868, #35259, #13647 ) ;
#13022 = PLANE ( 'NONE',  #33037 ) ;
#13023 = EDGE_CURVE ( 'NONE', #48933, #9978, #33343, .T. ) ;
#13024 = VECTOR ( 'NONE', #19502, 999.9999999999998863 ) ;
#13025 = CARTESIAN_POINT ( 'NONE',  ( -69.22435732763806016, -9.766609940218463848, 7.235198260161168626 ) ) ;
#13026 = EDGE_LOOP ( 'NONE', ( #6926, #2681, #35342, #28596 ) ) ;
#13027 = DIRECTION ( 'NONE',  ( 0.5364919789714477361, 0.6444004775717706579, 0.5449076811759711036 ) ) ;
#13028 = EDGE_CURVE ( 'NONE', #29379, #32268, #7475, .T. ) ;
#13029 = EDGE_CURVE ( 'NONE', #994, #13853, #28801, .T. ) ;
#13030 = EDGE_CURVE ( 'NONE', #43836, #43824, #7210, .T. ) ;
#13031 = ORIENTED_EDGE ( 'NONE', *, *, #48937, .F. ) ;
#13032 = EDGE_CURVE ( 'NONE', #5134, #12666, #24508, .T. ) ;
#13033 = VERTEX_POINT ( 'NONE', #33595 ) ;
#13034 = ORIENTED_EDGE ( 'NONE', *, *, #24814, .F. ) ;
#13035 = ORIENTED_EDGE ( 'NONE', *, *, #21749, .F. ) ;
#13036 = AXIS2_PLACEMENT_3D ( 'NONE', #55783, #8939, #51784 ) ;
#13037 = EDGE_LOOP ( 'NONE', ( #47260, #1979 ) ) ;
#13038 = LINE ( 'NONE', #804, #19667 ) ;
#13039 = DIRECTION ( 'NONE',  ( -0.5449076811759708816, 0.6444004775717707689, 0.5364919789714475140 ) ) ;
#13040 = VECTOR ( 'NONE', #18989, 1000.000000000000227 ) ;
#13041 = ORIENTED_EDGE ( 'NONE', *, *, #50262, .F. ) ;
#13042 = AXIS2_PLACEMENT_3D ( 'NONE', #43425, #35202, #34916 ) ;
#13043 = EDGE_CURVE ( 'NONE', #55101, #31910, #50906, .T. ) ;
#13044 = DIRECTION ( 'NONE',  ( 0.05705673239519650636, -0.9983709377222390602, -2.351258244848514932E-16 ) ) ;
#13045 = ORIENTED_EDGE ( 'NONE', *, *, #17869, .T. ) ;
#13046 = EDGE_CURVE ( 'NONE', #33948, #1716, #38730, .T. ) ;
#13047 = DIRECTION ( 'NONE',  ( 0.6427681459581294776, -0.7660444431189769032, 0.005002170337467562802 ) ) ;
#13048 = LINE ( 'NONE', #34080, #6854 ) ;
#13049 = ORIENTED_EDGE ( 'NONE', *, *, #25328, .T. ) ;
#13050 = CARTESIAN_POINT ( 'NONE',  ( 2.072287782118878319, 0.000000000000000000, -2.950529333540147015 ) ) ;
#13051 = VECTOR ( 'NONE', #13955, 999.9999999999998863 ) ;
#13052 = ORIENTED_EDGE ( 'NONE', *, *, #7928, .F. ) ;
#13053 = EDGE_CURVE ( 'NONE', #34537, #41034, #38422, .T. ) ;
#13054 = LINE ( 'NONE', #51407, #28245 ) ;
#13055 = EDGE_CURVE ( 'NONE', #34036, #52834, #40315, .T. ) ;
#13056 = VECTOR ( 'NONE', #27415, 1000.000000000000227 ) ;
#13057 = CARTESIAN_POINT ( 'NONE',  ( -16.36775718102074606, -0.6798977022406563764, 4.155552431687926429 ) ) ;
#13058 = VECTOR ( 'NONE', #2468, 999.9999999999998863 ) ;
#13059 = EDGE_LOOP ( 'NONE', ( #10316, #42258, #32563, #31151 ) ) ;
#13060 = FACE_OUTER_BOUND ( 'NONE', #37311, .T. ) ;
#13061 = LINE ( 'NONE', #47406, #10268 ) ;
#13062 = CARTESIAN_POINT ( 'NONE',  ( -11.61840533594187974, 0.000000000000000000, 4.560663995145184835 ) ) ;
#13063 = DIRECTION ( 'NONE',  ( 0.9999697198139515519, 0.000000000000000000, 0.007781995580013368816 ) ) ;
#13064 = ORIENTED_EDGE ( 'NONE', *, *, #23025, .T. ) ;
#13065 = DIRECTION ( 'NONE',  ( 0.7660212471507180654, -0.6427876096865404731, 0.005961354470445141482 ) ) ;
#13066 = PLANE ( 'NONE',  #48668 ) ;
#13067 = DIRECTION ( 'NONE',  ( 0.005961354470445682716, -0.6427876096865404731, -0.7660212471507180654 ) ) ;
#13068 = DIRECTION ( 'NONE',  ( 0.007781995580012663651, 0.000000000000000000, -0.9999697198139515519 ) ) ;
#13069 = LINE ( 'NONE', #8238, #10503 ) ;
#13070 = CARTESIAN_POINT ( 'NONE',  ( -3.033487535867088081, 3.746215373297818729, -2.040063999062676103 ) ) ;
#13071 = DIRECTION ( 'NONE',  ( 0.9999697198139515519, 0.000000000000000000, 0.007781995580013368816 ) ) ;
#13072 = FACE_OUTER_BOUND ( 'NONE', #48907, .T. ) ;
#13073 = LINE ( 'NONE', #4548, #44952 ) ;
#13074 = VECTOR ( 'NONE', #6078, 1000.000000000000227 ) ;
#13075 = ORIENTED_EDGE ( 'NONE', *, *, #28923, .T. ) ;
#13076 = DIRECTION ( 'NONE',  ( 0.9999697198139515519, 0.000000000000000000, 0.007781995580013368816 ) ) ;
#13077 = ORIENTED_EDGE ( 'NONE', *, *, #35316, .T. ) ;
#13078 = CARTESIAN_POINT ( 'NONE',  ( -20.54049170961573267, 0.000000000000000000, 4.660556269540326646 ) ) ;
#13079 = DIRECTION ( 'NONE',  ( 0.5364919789714477361, 0.6444004775717706579, 0.5449076811759711036 ) ) ;
#13080 = VECTOR ( 'NONE', #24494, 1000.000000000000114 ) ;
#13081 = DIRECTION ( 'NONE',  ( 0.9999697198139515519, 0.000000000000000000, 0.007781995580013368816 ) ) ;
#13082 = AXIS2_PLACEMENT_3D ( 'NONE', #31765, #32341, #19244 ) ;
#13083 = CARTESIAN_POINT ( 'NONE',  ( -19.60834386242827776, 0.000000000000000000, 4.298478389818581213 ) ) ;
#13084 = LINE ( 'NONE', #48855, #22037 ) ;
#13085 = ORIENTED_EDGE ( 'NONE', *, *, #15330, .T. ) ;
#13086 = VERTEX_POINT ( 'NONE', #27246 ) ;
#13087 = CARTESIAN_POINT ( 'NONE',  ( -22.40634380310664397, 0.000000000000000000, 5.584705972946605534 ) ) ;
#13088 = VECTOR ( 'NONE', #50739, 1000.000000000000227 ) ;
#13089 = CARTESIAN_POINT ( 'NONE',  ( -17.36532418587302473, -0.1191753592594177458, 13.67570816655714516 ) ) ;
#13090 = EDGE_LOOP ( 'NONE', ( #31639, #22040, #46019, #17162 ) ) ;
#13091 = AXIS2_PLACEMENT_3D ( 'NONE', #4057, #8047, #21079 ) ;
#13092 = FACE_OUTER_BOUND ( 'NONE', #23697, .T. ) ;
#13093 = ADVANCED_FACE ( 'NONE', ( #52796 ), #53107, .F. ) ;
#13094 = ORIENTED_EDGE ( 'NONE', *, *, #15076, .F. ) ;
#13095 = PLANE ( 'NONE',  #44022 ) ;
#13096 = VERTEX_POINT ( 'NONE', #48847 ) ;
#13097 = CARTESIAN_POINT ( 'NONE',  ( -15.86710544311044302, 0.000000000000000000, 13.13336954653252953 ) ) ;
#13098 = EDGE_CURVE ( 'NONE', #51326, #19370, #18756, .T. ) ;
#13099 = EDGE_CURVE ( 'NONE', #44683, #48518, #9368, .T. ) ;
#13100 = VECTOR ( 'NONE', #42208, 999.9999999999998863 ) ;
#13101 = EDGE_LOOP ( 'NONE', ( #38439, #37907, #32058, #46340 ) ) ;
#13102 = VECTOR ( 'NONE', #30060, 1000.000000000000227 ) ;
#13103 = ORIENTED_EDGE ( 'NONE', *, *, #734, .T. ) ;
#13104 = ORIENTED_EDGE ( 'NONE', *, *, #1654, .T. ) ;
#13105 = CARTESIAN_POINT ( 'NONE',  ( -15.07947971830811795, 0.000000000000000000, 5.641725323426407535 ) ) ;
#13106 = DIRECTION ( 'NONE',  ( 0.9999697198139515519, 0.000000000000000000, 0.007781995580013368816 ) ) ;
#13107 = LINE ( 'NONE', #30438, #54735 ) ;
#13108 = DIRECTION ( 'NONE',  ( -0.5364919789714478471, 0.6444004775717705469, -0.5449076811759709926 ) ) ;
#13109 = VERTEX_POINT ( 'NONE', #29915 ) ;
#13110 = ORIENTED_EDGE ( 'NONE', *, *, #27505, .F. ) ;
#13111 = AXIS2_PLACEMENT_3D ( 'NONE', #6282, #32661, #49963 ) ;
#13112 = ORIENTED_EDGE ( 'NONE', *, *, #42814, .F. ) ;
#13113 = CARTESIAN_POINT ( 'NONE',  ( -10.70924991679669169, 0.000000000000000000, 7.153063741485553351 ) ) ;
#13114 = AXIS2_PLACEMENT_3D ( 'NONE', #16823, #34417, #51720 ) ;
#13115 = ORIENTED_EDGE ( 'NONE', *, *, #30895, .F. ) ;
#13116 = DIRECTION ( 'NONE',  ( 0.7660212471507180654, -0.6427876096865404731, 0.005961354470445141482 ) ) ;
#13117 = VERTEX_POINT ( 'NONE', #8060 ) ;
#13118 = VECTOR ( 'NONE', #41741, 1000.000000000000227 ) ;
#13119 = DIRECTION ( 'NONE',  ( 0.000000000000000000, -0.000000000000000000, -1.000000000000000000 ) ) ;
#13120 = DIRECTION ( 'NONE',  ( 0.005002170337468016433, -0.7660444431189770143, -0.6427681459581293666 ) ) ;
#13121 = ORIENTED_EDGE ( 'NONE', *, *, #16828, .T. ) ;
#13122 = CARTESIAN_POINT ( 'NONE',  ( -17.22069023688172607, -3.917936722690662066, 3.445419328183913610 ) ) ;
#13123 = ORIENTED_EDGE ( 'NONE', *, *, #42005, .F. ) ;
#13124 = EDGE_CURVE ( 'NONE', #14373, #7205, #5136, .T. ) ;
#13125 = FACE_OUTER_BOUND ( 'NONE', #22944, .T. ) ;
#13126 = VECTOR ( 'NONE', #26012, 1000.000000000000227 ) ;
#13128 = ADVANCED_FACE ( 'NONE', ( #36082 ), #53384, .F. ) ;
#13127 = EDGE_LOOP ( 'NONE', ( #1183, #41249, #46616, #55562 ) ) ;
#13129 = DIRECTION ( 'NONE',  ( -0.9999697198139514409, -0.000000000000000000, -0.007781995580013368816 ) ) ;
#13130 = DIRECTION ( 'NONE',  ( 0.007781995580012663651, -3.146120232559066537E-19, -0.9999697198139514409 ) ) ;
#13131 = VECTOR ( 'NONE', #35391, 1000.000000000000114 ) ;
#13132 = CARTESIAN_POINT ( 'NONE',  ( -15.48567762416715077, -0.1941918491731566832, 2.890288465539208929 ) ) ;
#13133 = EDGE_CURVE ( 'NONE', #31427, #40934, #8319, .T. ) ;
#13134 = VERTEX_POINT ( 'NONE', #14482 ) ;
#13135 = AXIS2_PLACEMENT_3D ( 'NONE', #44076, #31847, #23347 ) ;
#13136 = LINE ( 'NONE', #9140, #1152 ) ;
#13137 = LINE ( 'NONE', #30472, #5602 ) ;
#13138 = ADVANCED_FACE ( 'NONE', ( #18447 ), #1111, .F. ) ;
#13139 = DIRECTION ( 'NONE',  ( -0.005961354470445682716, -0.6427876096865404731, 0.7660212471507180654 ) ) ;
#13140 = CARTESIAN_POINT ( 'NONE',  ( -11.30636317915456779, -0.1191753592594197858, 11.32220194836580340 ) ) ;
#13141 = DIRECTION ( 'NONE',  ( -0.5449076811759708816, 0.6444004775717707689, 0.5364919789714475140 ) ) ;
#13142 = CARTESIAN_POINT ( 'NONE',  ( -19.60990026154428278, 0.000000000000000000, 4.498472333781370125 ) ) ;
#13143 = VECTOR ( 'NONE', #20830, 999.9999999999998863 ) ;
#13144 = AXIS2_PLACEMENT_3D ( 'NONE', #44161, #35932, #10656 ) ;
#13145 = CARTESIAN_POINT ( 'NONE',  ( -13.12590506641494592, -0.1191753592594172878, 6.295589604590576371 ) ) ;
#13146 = ORIENTED_EDGE ( 'NONE', *, *, #25672, .F. ) ;
#13147 = LINE ( 'NONE', #42664, #38879 ) ;
#13148 = CARTESIAN_POINT ( 'NONE',  ( -14.62346498198288280, 0.000000000000000000, 6.753270344967709171 ) ) ;
#13149 = LINE ( 'NONE', #47801, #6045 ) ;
#13150 = ORIENTED_EDGE ( 'NONE', *, *, #51623, .T. ) ;
#13151 = DIRECTION ( 'NONE',  ( -0.7660212471507179544, -0.6427876096865405842, -0.005961354470445141482 ) ) ;
#13152 = EDGE_LOOP ( 'NONE', ( #4729, #11468, #34501, #53950 ) ) ;
#13153 = CARTESIAN_POINT ( 'NONE',  ( -21.12243245839617956, -5.698858183938163791, 14.23939898133697568 ) ) ;
#13154 = DIRECTION ( 'NONE',  ( 0.5364919789714477361, 0.6444004775717706579, 0.5449076811759711036 ) ) ;
#13155 = FACE_OUTER_BOUND ( 'NONE', #47156, .T. ) ;
#13156 = CARTESIAN_POINT ( 'NONE',  ( -68.04115265051312633, 1.999999999990856203, 4.403654818465982501 ) ) ;
#13157 = AXIS2_PLACEMENT_3D ( 'NONE', #21091, #42965, #40025 ) ;
#13158 = ORIENTED_EDGE ( 'NONE', *, *, #44957, .F. ) ;
#13159 = VERTEX_POINT ( 'NONE', #21400 ) ;
#13160 = CLOSED_SHELL ( 'NONE', ( #43827, #29227, #10303, #44606, #53124, #11479, #44827, #54797, #35461, #17663, #28041, #14786, #3976, #6857, #17209, #55333, #11745, #53873, #10614, #49999, #27367, #4945, #44545, #11435, #47399, #6321, #54230, #41877, #33767, #22103, #3275, #22660, #54366, #49968, #45435, #15902, #44436, #51617, #34084, #56080, #5233, #36232, #18692, #53536, #533, #22020, #21448, #26237, #52711, #21500, #27690, #14677, #18516, #18199, #50674 ) ) ;
#13161 = CARTESIAN_POINT ( 'NONE',  ( -19.60912206198628027, -0.1191753592594197858, 4.398475361799976113 ) ) ;
#13162 = DIRECTION ( 'NONE',  ( 0.5364919789714477361, 0.6444004775717706579, 0.5449076811759711036 ) ) ;
#13163 = LINE ( 'NONE', #35042, #1488 ) ;
#13164 = EDGE_CURVE ( 'NONE', #55170, #55582, #9676, .T. ) ;
#13165 = AXIS2_PLACEMENT_3D ( 'NONE', #10900, #37879, #24505 ) ;
#13166 = LINE ( 'NONE', #43532, #9386 ) ;
#13167 = DIRECTION ( 'NONE',  ( -0.005961354470445682716, -0.6427876096865404731, 0.7660212471507180654 ) ) ;
#13168 = DIRECTION ( 'NONE',  ( 0.6427681459581294776, -0.7660444431189769032, 0.005002170337467562802 ) ) ;
#13169 = AXIS2_PLACEMENT_3D ( 'NONE', #822, #22689, #43989 ) ;
#13170 = ORIENTED_EDGE ( 'NONE', *, *, #21204, .F. ) ;
#13171 = DIRECTION ( 'NONE',  ( 0.007781995580012663651, -3.146120232559066537E-19, -0.9999697198139514409 ) ) ;
#13172 = ADVANCED_FACE ( 'NONE', ( #25371 ), #22711, .F. ) ;
#13173 = DIRECTION ( 'NONE',  ( 0.000000000000000000, -0.000000000000000000, -1.000000000000000000 ) ) ;
#13174 = VECTOR ( 'NONE', #31894, 1000.000000000000227 ) ;
#13175 = ORIENTED_EDGE ( 'NONE', *, *, #29640, .F. ) ;
#13176 = VECTOR ( 'NONE', #55674, 999.9999999999998863 ) ;
#13177 = CARTESIAN_POINT ( 'NONE',  ( -18.67775241435682432, 0.000000000000000000, 4.136394454059623804 ) ) ;
#13178 = DIRECTION ( 'NONE',  ( 0.007781995580012663651, 0.000000000000000000, -0.9999697198139515519 ) ) ;
#13179 = CARTESIAN_POINT ( 'NONE',  ( -14.01545677930355183, 0.000000000000000000, 2.126011111488108174 ) ) ;
#13180 = AXIS2_PLACEMENT_3D ( 'NONE', #49921, #28929, #27830 ) ;
#13181 = EDGE_LOOP ( 'NONE', ( #51915, #23721, #31115, #21886 ) ) ;
#13182 = DIRECTION ( 'NONE',  ( 0.005961354470445682716, -0.6427876096865404731, -0.7660212471507180654 ) ) ;
#13183 = ORIENTED_EDGE ( 'NONE', *, *, #7365, .F. ) ;
#13184 = EDGE_CURVE ( 'NONE', #54636, #49471, #4071, .T. ) ;
#13185 = AXIS2_PLACEMENT_3D ( 'NONE', #32391, #5685, #23009 ) ;
#13186 = ORIENTED_EDGE ( 'NONE', *, *, #48281, .F. ) ;
#13187 = VECTOR ( 'NONE', #45812, 1000.000000000000000 ) ;
#13188 = VERTEX_POINT ( 'NONE', #5669 ) ;
#13189 = ORIENTED_EDGE ( 'NONE', *, *, #2491, .T. ) ;
#13190 = LINE ( 'NONE', #9193, #24824 ) ;
#13191 = ORIENTED_EDGE ( 'NONE', *, *, #41489, .T. ) ;
#13192 = DIRECTION ( 'NONE',  ( 0.007781995580012663651, -3.146120232559066537E-19, -0.9999697198139514409 ) ) ;
#13193 = EDGE_LOOP ( 'NONE', ( #52620, #48064, #37638, #53051 ) ) ;
#13194 = LINE ( 'NONE', #4662, #2321 ) ;
#13195 = EDGE_LOOP ( 'NONE', ( #26833, #11572, #22367, #5311 ) ) ;
#13196 = CARTESIAN_POINT ( 'NONE',  ( -20.24133259733970291, -5.213152330870663320, 13.10002382117402320 ) ) ;
#13197 = ORIENTED_EDGE ( 'NONE', *, *, #9774, .T. ) ;
#13198 = VECTOR ( 'NONE', #25720, 1000.000000000000227 ) ;
#13199 = CARTESIAN_POINT ( 'NONE',  ( -14.06954912762353338, -0.1191753592594177180, 8.134906297343379222 ) ) ;
#13200 = AXIS2_PLACEMENT_3D ( 'NONE', #34654, #12541, #4308 ) ;
#13201 = CARTESIAN_POINT ( 'NONE',  ( -10.47421230394850866, 0.000000000000000000, 10.95934586908605723 ) ) ;
#13202 = DIRECTION ( 'NONE',  ( -0.005002170337468016433, -0.7660444431189770143, 0.6427681459581293666 ) ) ;
#13203 = LINE ( 'NONE', #39313, #28704 ) ;
#13204 = DIRECTION ( 'NONE',  ( 0.5364919789714477361, 0.6444004775717706579, 0.5449076811759711036 ) ) ;
#13205 = VECTOR ( 'NONE', #50132, 1000.000000000000114 ) ;
#13206 = ORIENTED_EDGE ( 'NONE', *, *, #27272, .F. ) ;
#13207 = ORIENTED_EDGE ( 'NONE', *, *, #26735, .T. ) ;
#13208 = LINE ( 'NONE', #38779, #33132 ) ;
#13209 = EDGE_CURVE ( 'NONE', #8976, #5703, #26690, .T. ) ;
#13210 = FACE_OUTER_BOUND ( 'NONE', #53415, .T. ) ;
#13211 = VECTOR ( 'NONE', #23479, 1000.000000000000114 ) ;
#13212 = DIRECTION ( 'NONE',  ( -0.7660212471507179544, -0.6427876096865405842, -0.005961354470445141482 ) ) ;
#13213 = VECTOR ( 'NONE', #8884, 999.9999999999998863 ) ;
#13214 = AXIS2_PLACEMENT_3D ( 'NONE', #16472, #37217, #54521 ) ;
#13215 = LINE ( 'NONE', #962, #21264 ) ;
#13216 = DIRECTION ( 'NONE',  ( 0.000000000000000000, -1.000000000000000000, 0.000000000000000000 ) ) ;
#13217 = LINE ( 'NONE', #35096, #29588 ) ;
#13218 = ORIENTED_EDGE ( 'NONE', *, *, #6742, .T. ) ;
#13219 = LINE ( 'NONE', #29970, #12063 ) ;
#13220 = DIRECTION ( 'NONE',  ( 0.000000000000000000, 0.000000000000000000, 1.000000000000000000 ) ) ;
#13221 = ORIENTED_EDGE ( 'NONE', *, *, #48203, .F. ) ;
#13222 = EDGE_CURVE ( 'NONE', #53048, #50265, #51755, .T. ) ;
#13223 = DIRECTION ( 'NONE',  ( -0.9999697198139514409, -0.000000000000000000, -0.007781995580013368816 ) ) ;
#13224 = DIRECTION ( 'NONE',  ( -0.005961354470445682716, -0.6427876096865404731, 0.7660212471507180654 ) ) ;
#13225 = VECTOR ( 'NONE', #44971, 999.9999999999998863 ) ;
#13226 = VECTOR ( 'NONE', #21104, 999.9999999999998863 ) ;
#13227 = CARTESIAN_POINT ( 'NONE',  ( -17.88586307477561022, 0.000000000000000000, 8.005203831659914115 ) ) ;
#13228 = ADVANCED_FACE ( 'NONE', ( #35783 ), #51505, .F. ) ;
#13229 = EDGE_CURVE ( 'NONE', #13159, #11166, #36332, .T. ) ;
#13230 = CYLINDRICAL_SURFACE ( 'NONE', #10567, 6.000000000000001776 ) ;
#13231 = VECTOR ( 'NONE', #39359, 999.9999999999998863 ) ;
#13232 = PLANE ( 'NONE',  #23808 ) ;
#13233 = ORIENTED_EDGE ( 'NONE', *, *, #40064, .T. ) ;
#13234 = AXIS2_PLACEMENT_3D ( 'NONE', #4763, #30332, #52187 ) ;
#13235 = ORIENTED_EDGE ( 'NONE', *, *, #7038, .T. ) ;
#13236 = LINE ( 'NONE', #30570, #28491 ) ;
#13237 = PLANE ( 'NONE',  #32211 ) ;
#13238 = CARTESIAN_POINT ( 'NONE',  ( -18.49821513591315991, 2.391131607591507446, 7.990910409668134484 ) ) ;
#13239 = EDGE_CURVE ( 'NONE', #2673, #9548, #11326, .T. ) ;
#13240 = CARTESIAN_POINT ( 'NONE',  ( -21.82894433340611684, -4.889348428825662118, 13.18528876708279185 ) ) ;
#13241 = ADVANCED_FACE ( 'NONE', ( #31795 ), #45676, .F. ) ;
#13242 = CARTESIAN_POINT ( 'NONE',  ( -46.02156441860523017, 4.933012701892206309, 5.000000000000000000 ) ) ;
#13243 = FACE_OUTER_BOUND ( 'NONE', #660, .T. ) ;
#13244 = CARTESIAN_POINT ( 'NONE',  ( 2.072287782118878319, 0.000000000000000000, -2.950529333540147015 ) ) ;
#13245 = EDGE_CURVE ( 'NONE', #45223, #5769, #19013, .T. ) ;
#13246 = VERTEX_POINT ( 'NONE', #24381 ) ;
#13247 = AXIS2_PLACEMENT_3D ( 'NONE', #38999, #16869, #5215 ) ;
#13248 = CARTESIAN_POINT ( 'NONE',  ( -23.33693525117809386, 0.000000000000000000, 5.746789908705562944 ) ) ;
#13249 = CARTESIAN_POINT ( 'NONE',  ( -20.70076447251854290, -0.8417996532631553119, 6.104348297203140206 ) ) ;
#13250 = EDGE_LOOP ( 'NONE', ( #7397, #42150, #10016, #8843 ) ) ;
#13251 = PLANE ( 'NONE',  #41017 ) ;
#13252 = ORIENTED_EDGE ( 'NONE', *, *, #23040, .T. ) ;
#13253 = CARTESIAN_POINT ( 'NONE',  ( -12.93745269883482152, 0.000000000000000000, 8.243719561634259563 ) ) ;
#13254 = AXIS2_PLACEMENT_3D ( 'NONE', #25704, #42186, #24864 ) ;
#13255 = CARTESIAN_POINT ( 'NONE',  ( -13.74730076765101217, 2.876837460659009693, 1.930064033053078498 ) ) ;
#13256 = ADVANCED_FACE ( 'NONE', ( #54214 ), #27838, .F. ) ;
#13257 = EDGE_LOOP ( 'NONE', ( #27354, #38298, #21998, #32918 ) ) ;
#13258 = VECTOR ( 'NONE', #20746, 999.9999999999998863 ) ;
#13259 = ORIENTED_EDGE ( 'NONE', *, *, #22066, .F. ) ;
#13260 = EDGE_CURVE ( 'NONE', #485, #2545, #28089, .T. ) ;
#13261 = ORIENTED_EDGE ( 'NONE', *, *, #28161, .F. ) ;
#13262 = AXIS2_PLACEMENT_3D ( 'NONE', #46496, #33195, #33461 ) ;
#13263 = ORIENTED_EDGE ( 'NONE', *, *, #36947, .F. ) ;
#13264 = AXIS2_PLACEMENT_3D ( 'NONE', #15993, #2895, #20223 ) ;
#13265 = EDGE_LOOP ( 'NONE', ( #8614, #18476, #43568, #50333 ) ) ;
#13266 = VERTEX_POINT ( 'NONE', #32623 ) ;
#13267 = DIRECTION ( 'NONE',  ( -0.5449076811759708816, 0.6444004775717707689, 0.5364919789714475140 ) ) ;
#13268 = CARTESIAN_POINT ( 'NONE',  ( -21.47419595591918906, 0.000000000000000000, 5.222628093224860102 ) ) ;
#13269 = CARTESIAN_POINT ( 'NONE',  ( 4.902479726011972794, 0.000000000000000000, -2.247047898273223598 ) ) ;
#13270 = VECTOR ( 'NONE', #46409, 999.9999999999998863 ) ;
#13271 = VECTOR ( 'NONE', #1077, 1000.000000000000227 ) ;
#13272 = VERTEX_POINT ( 'NONE', #23817 ) ;
#13273 = CARTESIAN_POINT ( 'NONE',  ( -17.74482636761137044, -0.1191753592594197858, 3.674319602356483916 ) ) ;
#13274 = ORIENTED_EDGE ( 'NONE', *, *, #30573, .F. ) ;
#13275 = ORIENTED_EDGE ( 'NONE', *, *, #29654, .T. ) ;
#13276 = AXIS2_PLACEMENT_3D ( 'NONE', #11958, #29289, #46608 ) ;
#13277 = VECTOR ( 'NONE', #42673, 999.9999999999998863 ) ;
#13278 = DIRECTION ( 'NONE',  ( 0.000000000000000000, -0.000000000000000000, -1.000000000000000000 ) ) ;
#13279 = PLANE ( 'NONE',  #18539 ) ;
#13280 = DIRECTION ( 'NONE',  ( 0.3535533905932738974, -0.6123724356957929160, 0.7071067811865487940 ) ) ;
#13281 = VERTEX_POINT ( 'NONE', #2776 ) ;
#13282 = FACE_OUTER_BOUND ( 'NONE', #18014, .T. ) ;
#13283 = EDGE_LOOP ( 'NONE', ( #52045, #10523, #31813, #22614, #25904 ) ) ;
#13284 = CARTESIAN_POINT ( 'NONE',  ( -13.89904558389786438, -0.5179957512181551094, 2.930912325616202629 ) ) ;
#13285 = ADVANCED_FACE ( 'NONE', ( #45395 ), #23291, .F. ) ;
#13286 = CARTESIAN_POINT ( 'NONE',  ( -27.99923088623136636, 0.000000000000000000, 7.757173251277078130 ) ) ;
#13287 = AXIS2_PLACEMENT_3D ( 'NONE', #22467, #31244, #14764 ) ;
#13288 = CARTESIAN_POINT ( 'NONE',  ( -50.27554558092695913, 4.209026340267034705, 5.000000000000000000 ) ) ;
#13289 = CARTESIAN_POINT ( 'NONE',  ( -18.79501849392080359, 0.000000000000000000, 5.412804085319542047 ) ) ;
#13290 = DIRECTION ( 'NONE',  ( -0.005961354470445682716, -0.6427876096865404731, 0.7660212471507180654 ) ) ;
#13291 = LINE ( 'NONE', #39106, #9481 ) ;
#13292 = PLANE ( 'NONE',  #18462 ) ;
#13293 = CARTESIAN_POINT ( 'NONE',  ( -16.01162756549557287, 0.000000000000000000, 6.003803203148152967 ) ) ;
#13294 = ORIENTED_EDGE ( 'NONE', *, *, #13425, .F. ) ;
#13295 = DIRECTION ( 'NONE',  ( 0.000000000000000000, -0.000000000000000000, -1.000000000000000000 ) ) ;
#13296 = PRODUCT_DEFINITION_SHAPE ( 'NONE', 'NONE',  #27394 ) ;
#13297 = VECTOR ( 'NONE', #20169, 999.9999999999998863 ) ;
#13298 = EDGE_CURVE ( 'NONE', #34545, #55928, #41148, .T. ) ;
#13299 = EDGE_CURVE ( 'NONE', #24514, #43824, #49927, .T. ) ;
#13300 = PLANE ( 'NONE',  #32865 ) ;
#13301 = DIRECTION ( 'NONE',  ( 0.005002170337468016433, -0.7660444431189770143, -0.6427681459581293666 ) ) ;
#13303 = CARTESIAN_POINT ( 'NONE',  ( -12.09741250030938176, 0.000000000000000000, 6.403596599665996258 ) ) ;
#13302 = AXIS2_PLACEMENT_3D ( 'NONE', #12172, #16160, #20707 ) ;
#13304 = CARTESIAN_POINT ( 'NONE',  ( -37.69457521496538277, 9.163251890963174162, -4.944930165255981613 ) ) ;
#13305 = CARTESIAN_POINT ( 'NONE',  ( -17.26532721389163072, 0.000000000000000000, 13.67648636611514590 ) ) ;
#13306 = ADVANCED_FACE ( 'NONE', ( #41444 ), #37431, .F. ) ;
#13307 = DIRECTION ( 'NONE',  ( -0.8660254037844379305, -0.5000000000000011102, 0.000000000000000000 ) ) ;
#13308 = VECTOR ( 'NONE', #49616, 999.9999999999998863 ) ;
#13309 = CARTESIAN_POINT ( 'NONE',  ( -17.80101456987863173, -0.1191753592594181482, 9.952527519488127083 ) ) ;
#13310 = ORIENTED_EDGE ( 'NONE', *, *, #51462, .T. ) ;
#13311 = DIRECTION ( 'NONE',  ( -0.5364919789714478471, 0.6444004775717705469, -0.5449076811759709926 ) ) ;
#13312 = LINE ( 'NONE', #17852, #27669 ) ;
#13313 = CARTESIAN_POINT ( 'NONE',  ( -25.20123094555300369, 0.000000000000000000, 6.470945668149052032 ) ) ;
#13314 = VECTOR ( 'NONE', #51800, 1000.000000000000227 ) ;
#13315 = CARTESIAN_POINT ( 'NONE',  ( -15.30390940309393599, -4.889348428825662118, 10.65074360903057382 ) ) ;
#13316 = EDGE_CURVE ( 'NONE', #52307, #5827, #28658, .T. ) ;
#13317 = CARTESIAN_POINT ( 'NONE',  ( -11.20636620717317378, 0.000000000000000000, 11.32298014792380414 ) ) ;
#13318 = DIRECTION ( 'NONE',  ( -0.005002170337468016433, -0.7660444431189770143, 0.6427681459581293666 ) ) ;
#13319 = DIRECTION ( 'NONE',  ( 0.000000000000000000, -1.000000000000000000, 0.000000000000000000 ) ) ;
#13320 = AXIS2_PLACEMENT_3D ( 'NONE', #13334, #47956, #52751 ) ;
#13321 = EDGE_CURVE ( 'NONE', #7193, #21470, #14748, .T. ) ;
#13323 = LINE ( 'NONE', #52207, #4060 ) ;
#13322 = VECTOR ( 'NONE', #46044, 999.9999999999998863 ) ;
#13324 = DIRECTION ( 'NONE',  ( -0.6427681459581293666, -0.7660444431189770143, -0.005002170337467561935 ) ) ;
#13325 = VERTEX_POINT ( 'NONE', #15566 ) ;
#13326 = CARTESIAN_POINT ( 'NONE',  ( -14.09440035361675747, -4.079838673713161334, 2.225896648385081278 ) ) ;
#13327 = ADVANCED_FACE ( 'NONE', ( #24115 ), #40613, .F. ) ;
#13328 = ORIENTED_EDGE ( 'NONE', *, *, #33811, .T. ) ;
#13329 = AXIS2_PLACEMENT_3D ( 'NONE', #34157, #4336, #16517 ) ;
#13330 = ORIENTED_EDGE ( 'NONE', *, *, #12919, .F. ) ;
#13331 = VERTEX_POINT ( 'NONE', #45977 ) ;
#13332 = ORIENTED_EDGE ( 'NONE', *, *, #42834, .T. ) ;
#13333 = ORIENTED_EDGE ( 'NONE', *, *, #10407, .F. ) ;
#13334 = CARTESIAN_POINT ( 'NONE',  ( 2.072287782118878319, 0.000000000000000000, -2.950529333540147015 ) ) ;
#13335 = LINE ( 'NONE', #30655, #17626 ) ;
#13336 = ORIENTED_EDGE ( 'NONE', *, *, #20054, .F. ) ;
#13337 = VECTOR ( 'NONE', #40761, 1000.000000000000227 ) ;
#13338 = ORIENTED_EDGE ( 'NONE', *, *, #31131, .T. ) ;
#13339 = VECTOR ( 'NONE', #43036, 1000.000000000000114 ) ;
#13340 = LINE ( 'NONE', #22424, #379 ) ;
#13341 = VERTEX_POINT ( 'NONE', #49395 ) ;
#13342 = DIRECTION ( 'NONE',  ( -0.05705673239519651330, 0.9983709377222391712, 2.351258244848514932E-16 ) ) ;
#13343 = CARTESIAN_POINT ( 'NONE',  ( -14.20280369269832832, 0.000000000000000000, 12.40765738797303719 ) ) ;
#13344 = ORIENTED_EDGE ( 'NONE', *, *, #24733, .T. ) ;
#13345 = FACE_OUTER_BOUND ( 'NONE', #46642, .T. ) ;
#13346 = EDGE_CURVE ( 'NONE', #9458, #6017, #19276, .T. ) ;
#13347 = ORIENTED_EDGE ( 'NONE', *, *, #10381, .F. ) ;
#13348 = AXIS2_PLACEMENT_3D ( 'NONE', #9652, #14459, #31777 ) ;
#13349 = DIRECTION ( 'NONE',  ( 0.005961354470445682716, -0.6427876096865404731, -0.7660212471507180654 ) ) ;
#13350 = EDGE_CURVE ( 'NONE', #55970, #49405, #1946, .T. ) ;
#13351 = CARTESIAN_POINT ( 'NONE',  ( -2.881839257824877265, -5.376589517215482950, -2.098969340251471305 ) ) ;
#13352 = AXIS2_PLACEMENT_3D ( 'NONE', #46296, #54833, #28998 ) ;
#13353 = EDGE_LOOP ( 'NONE', ( #37000, #12480, #18287, #3111, #52691 ) ) ;
#13354 = CARTESIAN_POINT ( 'NONE',  ( -13.47695292330622507, 0.000000000000000000, 4.546200348073146991 ) ) ;
#13355 = DIRECTION ( 'NONE',  ( -0.5449076811759708816, 0.6444004775717707689, 0.5364919789714475140 ) ) ;
#13356 = LINE ( 'NONE', #1387, #25782 ) ;
#13357 = EDGE_CURVE ( 'NONE', #49206, #6706, #49685, .T. ) ;
#13358 = ORIENTED_EDGE ( 'NONE', *, *, #53580, .T. ) ;
#13359 = CARTESIAN_POINT ( 'NONE',  ( -19.15687783499660313, -0.6798977022406558213, 4.300810742247143104 ) ) ;
#13360 = EDGE_LOOP ( 'NONE', ( #6328, #19020, #2247, #40397 ) ) ;
#13361 = EDGE_CURVE ( 'NONE', #55490, #48977, #38275, .T. ) ;
#13362 = EDGE_CURVE ( 'NONE', #26758, #17816, #11869, .T. ) ;
#13363 = EDGE_CURVE ( 'NONE', #55993, #48862, #33735, .T. ) ;
#13364 = CARTESIAN_POINT ( 'NONE',  ( -11.67244013076689946, 0.000000000000000000, 11.50401908778467863 ) ) ;
#13365 = PLANE ( 'NONE',  #18765 ) ;
#13366 = CARTESIAN_POINT ( 'NONE',  ( -50.45472955569960760, 3.742236127018431890, 5.000000000000000000 ) ) ;
#13367 = LINE ( 'NONE', #575, #46811 ) ;
#13368 = DIRECTION ( 'NONE',  ( 0.6427681459581294776, -0.7660444431189769032, 0.005002170337467562802 ) ) ;
#13369 = ADVANCED_FACE ( 'NONE', ( #3920 ), #55598, .F. ) ;
#13370 = FACE_OUTER_BOUND ( 'NONE', #29421, .T. ) ;
#13371 = FACE_OUTER_BOUND ( 'NONE', #33122, .T. ) ;
#13372 = DIRECTION ( 'NONE',  ( 0.000000000000000000, -1.000000000000000000, 0.000000000000000000 ) ) ;
#13373 = DIRECTION ( 'NONE',  ( 0.000000000000000000, 0.000000000000000000, 1.000000000000000000 ) ) ;
#13374 = DIRECTION ( 'NONE',  ( 0.007781995580012662783, 0.000000000000000000, -0.9999697198139514409 ) ) ;
#13375 = ORIENTED_EDGE ( 'NONE', *, *, #44348, .T. ) ;
#13376 = DIRECTION ( 'NONE',  ( 0.005961354470445682716, -0.6427876096865404731, -0.7660212471507180654 ) ) ;
#13377 = DIRECTION ( 'NONE',  ( 0.9999697198139515519, 0.000000000000000000, 0.007781995580013368816 ) ) ;
#13378 = CARTESIAN_POINT ( 'NONE',  ( -22.40478740399063895, 0.000000000000000000, 5.384712028983816623 ) ) ;
#13379 = DIRECTION ( 'NONE',  ( -0.5364919789714478471, 0.6444004775717705469, -0.5449076811759709926 ) ) ;
#13380 = EDGE_CURVE ( 'NONE', #26525, #41032, #12471, .T. ) ;
#13381 = CARTESIAN_POINT ( 'NONE',  ( -29.86352658060627618, 0.000000000000000000, 8.481329010720569883 ) ) ;
#13382 = DIRECTION ( 'NONE',  ( -0.7660212471507179544, -0.6427876096865405842, -0.005961354470445141482 ) ) ;
#13383 = VERTEX_POINT ( 'NONE', #47357 ) ;
#13384 = EDGE_CURVE ( 'NONE', #54774, #18119, #20401, .T. ) ;
#13385 = VECTOR ( 'NONE', #10671, 1000.000000000000227 ) ;
#13386 = ORIENTED_EDGE ( 'NONE', *, *, #4207, .F. ) ;
#13387 = EDGE_CURVE ( 'NONE', #39017, #51326, #29195, .T. ) ;
#13388 = CARTESIAN_POINT ( 'NONE',  ( -22.40634380310664397, 0.000000000000000000, 5.584705972946605534 ) ) ;
#13389 = CARTESIAN_POINT ( 'NONE',  ( -15.87975247367846166, 0.000000000000000000, 2.850166870931599927 ) ) ;
#13391 = VERTEX_POINT ( 'NONE', #38013 ) ;
#13390 = APPLICATION_CONTEXT ( 'automotive_design' ) ;
#13392 = FACE_OUTER_BOUND ( 'NONE', #4396, .T. ) ;
#13393 = EDGE_CURVE ( 'NONE', #10405, #36484, #25500, .T. ) ;
#13394 = VECTOR ( 'NONE', #9505, 1000.000000000000000 ) ;
#13395 = ORIENTED_EDGE ( 'NONE', *, *, #19953, .F. ) ;
#13396 = LINE ( 'NONE', #48576, #28579 ) ;
#13397 = ORIENTED_EDGE ( 'NONE', *, *, #29720, .F. ) ;
#13398 = CARTESIAN_POINT ( 'NONE',  ( -56.75000000000000711, 6.050000000000001599, -2.749999999999994671 ) ) ;
#13399 = EDGE_CURVE ( 'NONE', #28247, #48080, #4234, .T. ) ;
#13400 = ORIENTED_EDGE ( 'NONE', *, *, #39415, .F. ) ;
#13401 = EDGE_LOOP ( 'NONE', ( #50201, #53055, #28967, #44465 ) ) ;
#13402 = ORIENTED_EDGE ( 'NONE', *, *, #36149, .T. ) ;
#13403 = DIRECTION ( 'NONE',  ( 0.005961354470445682716, -0.6427876096865404731, -0.7660212471507180654 ) ) ;
#13404 = FACE_OUTER_BOUND ( 'NONE', #34281, .T. ) ;
#13405 = PLANE ( 'NONE',  #33024 ) ;
#13406 = DIRECTION ( 'NONE',  ( 0.007781995580012663651, 0.000000000000000000, -0.9999697198139515519 ) ) ;
#13407 = ORIENTED_EDGE ( 'NONE', *, *, #52068, .T. ) ;
#13408 = ORIENTED_EDGE ( 'NONE', *, *, #25478, .T. ) ;
#13409 = CARTESIAN_POINT ( 'NONE',  ( -19.23990622075459811, 1.095915999411505526, 4.120399239466145502 ) ) ;
#13410 = ORIENTED_EDGE ( 'NONE', *, *, #31957, .T. ) ;
#13411 = LINE ( 'NONE', #21899, #18456 ) ;
#13412 = ORIENTED_EDGE ( 'NONE', *, *, #33353, .T. ) ;
#13413 = DIRECTION ( 'NONE',  ( 0.005002170337468016433, -0.7660444431189770143, -0.6427681459581293666 ) ) ;
#13414 = CARTESIAN_POINT ( 'NONE',  ( -9.135000016821216207, 6.796527418557151812, 0.3299706567759553844 ) ) ;
#13415 = ORIENTED_EDGE ( 'NONE', *, *, #19761, .T. ) ;
#13416 = CARTESIAN_POINT ( 'NONE',  ( -19.12962290826653700, 0.000000000000000000, 14.40064212555863854 ) ) ;
#13417 = ORIENTED_EDGE ( 'NONE', *, *, #7626, .F. ) ;
#13418 = DIRECTION ( 'NONE',  ( -0.9999697198139514409, -0.000000000000000000, -0.007781995580013368816 ) ) ;
#13419 = ORIENTED_EDGE ( 'NONE', *, *, #30358, .T. ) ;
#13420 = DIRECTION ( 'NONE',  ( 0.7660212471507180654, -0.6427876096865404731, 0.005961354470445141482 ) ) ;
#13421 = PLANE ( 'NONE',  #22979 ) ;
#13422 = CARTESIAN_POINT ( 'NONE',  ( -16.81190032086591302, 0.000000000000000000, 3.212244750653343583 ) ) ;
#13423 = ORIENTED_EDGE ( 'NONE', *, *, #23407, .F. ) ;
#13424 = EDGE_CURVE ( 'NONE', #41178, #34966, #33471, .T. ) ;
#13425 = EDGE_CURVE ( 'NONE', #55458, #25319, #17004, .T. ) ;
#13426 = DIRECTION ( 'NONE',  ( 0.9999697198139515519, 0.000000000000000000, 0.007781995580013368816 ) ) ;
#13427 = VECTOR ( 'NONE', #7987, 1000.000000000000000 ) ;
#13428 = DIRECTION ( 'NONE',  ( 0.000000000000000000, -0.000000000000000000, -1.000000000000000000 ) ) ;
#13429 = LINE ( 'NONE', #47198, #14009 ) ;
#13430 = LINE ( 'NONE', #30746, #6004 ) ;
#13431 = ADVANCED_FACE ( 'NONE', ( #51629 ), #55316, .F. ) ;
#13432 = CARTESIAN_POINT ( 'NONE',  ( -13.06083377814856483, -5.536956232915664522, 10.84229159693478017 ) ) ;
#13433 = DIRECTION ( 'NONE',  ( 0.5000000000000011102, -0.8660254037844380415, 0.000000000000000000 ) ) ;
#13434 = DIRECTION ( 'NONE',  ( 0.007781995580012663651, 0.000000000000000000, -0.9999697198139515519 ) ) ;
#13435 = VERTEX_POINT ( 'NONE', #46505 ) ;
#13436 = FACE_OUTER_BOUND ( 'NONE', #41344, .T. ) ;
#13437 = DIRECTION ( 'NONE',  ( 0.000000000000000000, -0.000000000000000000, -1.000000000000000000 ) ) ;
#13438 = CARTESIAN_POINT ( 'NONE',  ( -15.29625084614291097, 0.2864062442990042978, 2.614377164303661960 ) ) ;
#13439 = VERTEX_POINT ( 'NONE', #16411 ) ;
#13440 = CARTESIAN_POINT ( 'NONE',  ( 2.072287782118878319, 0.000000000000000000, -2.950529333540147015 ) ) ;
#13441 = LINE ( 'NONE', #30758, #15451 ) ;
#13442 = ORIENTED_EDGE ( 'NONE', *, *, #36294, .T. ) ;
#13443 = CARTESIAN_POINT ( 'NONE',  ( -10.84028925556084388, -0.1191753592594197858, 11.14116300850493246 ) ) ;
#13444 = LINE ( 'NONE', #10004, #30290 ) ;
#13445 = CARTESIAN_POINT ( 'NONE',  ( -15.86710544311044302, 0.000000000000000000, 13.13336954653252953 ) ) ;
#13446 = LINE ( 'NONE', #52876, #28307 ) ;
#13447 = VERTEX_POINT ( 'NONE', #3379 ) ;
#13448 = ORIENTED_EDGE ( 'NONE', *, *, #39865, .F. ) ;
#13449 = CARTESIAN_POINT ( 'NONE',  ( -11.59673056228890076, 0.000000000000000000, 1.775502128378044331 ) ) ;
#13450 = DIRECTION ( 'NONE',  ( 0.005961354470445682716, -0.6427876096865404731, -0.7660212471507180654 ) ) ;
#13451 = FACE_OUTER_BOUND ( 'NONE', #29226, .T. ) ;
#13452 = CARTESIAN_POINT ( 'NONE',  ( -11.38054826722768276, 24.93301270189227736, -3.000000000000000000 ) ) ;
#13453 = DIRECTION ( 'NONE',  ( 0.007781995580012663651, 0.000000000000000000, -0.9999697198139515519 ) ) ;
#13454 = CARTESIAN_POINT ( 'NONE',  ( -21.47263955680318404, 0.000000000000000000, 5.022634149262071190 ) ) ;
#13455 = VERTEX_POINT ( 'NONE', #33207 ) ;
#13456 = LINE ( 'NONE', #31617, #17454 ) ;
#13457 = ADVANCED_FACE ( 'NONE', ( #16151 ), #3640, .F. ) ;
#13458 = FACE_OUTER_BOUND ( 'NONE', #53737, .T. ) ;
#13459 = ORIENTED_EDGE ( 'NONE', *, *, #42571, .F. ) ;
#13460 = EDGE_CURVE ( 'NONE', #30608, #37937, #8192, .T. ) ;
#13461 = CARTESIAN_POINT ( 'NONE',  ( -69.66347483736342383, -8.676648739292067702, -7.503912900124009688 ) ) ;
#13462 = LINE ( 'NONE', #39848, #55824 ) ;
#13463 = EDGE_CURVE ( 'NONE', #54313, #19601, #42551, .T. ) ;
#13464 = LINE ( 'NONE', #44651, #4005 ) ;
#13465 = ORIENTED_EDGE ( 'NONE', *, *, #34896, .T. ) ;
#13466 = VECTOR ( 'NONE', #24572, 1000.000000000000114 ) ;
#13467 = PLANE ( 'NONE',  #32275 ) ;
#13468 = EDGE_CURVE ( 'NONE', #9720, #10560, #28935, .T. ) ;
#13469 = ORIENTED_EDGE ( 'NONE', *, *, #42029, .T. ) ;
#13470 = VERTEX_POINT ( 'NONE', #24952 ) ;
#13471 = ORIENTED_EDGE ( 'NONE', *, *, #49514, .F. ) ;
#13472 = ORIENTED_EDGE ( 'NONE', *, *, #34068, .F. ) ;
#13473 = CARTESIAN_POINT ( 'NONE',  ( -18.03805572822844283, -4.889348428825663895, 3.731918723547563932 ) ) ;
#13474 = ORIENTED_EDGE ( 'NONE', *, *, #36107, .F. ) ;
#13475 = FACE_OUTER_BOUND ( 'NONE', #41529, .T. ) ;
#13476 = VERTEX_POINT ( 'NONE', #20699 ) ;
#13477 = CARTESIAN_POINT ( 'NONE',  ( -14.94760462649100496, 0.000000000000000000, 2.488088991209854051 ) ) ;
#13478 = ORIENTED_EDGE ( 'NONE', *, *, #51458, .F. ) ;
#13479 = CARTESIAN_POINT ( 'NONE',  ( -14.01545677930355183, 0.000000000000000000, 2.126011111488108174 ) ) ;
#13480 = EDGE_LOOP ( 'NONE', ( #12952, #51075, #2431, #33302 ) ) ;
#13481 = DIRECTION ( 'NONE',  ( 0.007781995580012663651, 0.000000000000000000, -0.9999697198139515519 ) ) ;
#13482 = PLANE ( 'NONE',  #28654 ) ;
#13483 = DIRECTION ( 'NONE',  ( 0.007781995580012663651, -3.146120232559066537E-19, -0.9999697198139514409 ) ) ;
#13484 = LINE ( 'NONE', #31649, #20558 ) ;
#13485 = FACE_OUTER_BOUND ( 'NONE', #8872, .T. ) ;
#13486 = EDGE_LOOP ( 'NONE', ( #25605, #48872, #318, #29235 ) ) ;
#13487 = EDGE_CURVE ( 'NONE', #17790, #6537, #48791, .T. ) ;
#13488 = ORIENTED_EDGE ( 'NONE', *, *, #8239, .F. ) ;
#13489 = LINE ( 'NONE', #51805, #36734 ) ;
#13490 = DIRECTION ( 'NONE',  ( -0.5449076811759708816, 0.6444004775717707689, 0.5364919789714475140 ) ) ;
#13491 = EDGE_CURVE ( 'NONE', #1421, #394, #35430, .T. ) ;
#13492 = EDGE_CURVE ( 'NONE', #7274, #30542, #40027, .T. ) ;
#13493 = DIRECTION ( 'NONE',  ( -0.005961354470445682716, -0.6427876096865404731, 0.7660212471507180654 ) ) ;
#13494 = DIRECTION ( 'NONE',  ( -0.9999697198139514409, -0.000000000000000000, -0.007781995580013368816 ) ) ;
#13495 = LINE ( 'NONE', #115, #16785 ) ;
#13496 = CARTESIAN_POINT ( 'NONE',  ( -18.16200224167504373, 0.000000000000000000, 9.480383132038964433 ) ) ;
#13497 = ORIENTED_EDGE ( 'NONE', *, *, #22266, .T. ) ;
#13498 = PLANE ( 'NONE',  #48343 ) ;
#13499 = LINE ( 'NONE', #38790, #5912 ) ;
#13500 = ORIENTED_EDGE ( 'NONE', *, *, #48843, .F. ) ;
#13501 = VECTOR ( 'NONE', #47799, 1000.000000000000227 ) ;
#13502 = PLANE ( 'NONE',  #34300 ) ;
#13503 = CARTESIAN_POINT ( 'NONE',  ( -17.74560456716937296, 0.000000000000000000, 3.774316574337878372 ) ) ;
#13504 = FACE_OUTER_BOUND ( 'NONE', #26107, .T. ) ;
#13505 = CARTESIAN_POINT ( 'NONE',  ( -61.10213307005877681, 6.758246409053505488, -3.000000000000007105 ) ) ;
#13506 = EDGE_CURVE ( 'NONE', #42368, #6114, #17550, .T. ) ;
#13507 = LINE ( 'NONE', #52662, #29238 ) ;
#13508 = ORIENTED_EDGE ( 'NONE', *, *, #55272, .F. ) ;
#13509 = VERTEX_POINT ( 'NONE', #22090 ) ;
#13510 = DIRECTION ( 'NONE',  ( -0.6427681459581293666, -0.7660444431189770143, -0.005002170337467561935 ) ) ;
#13511 = CARTESIAN_POINT ( 'NONE',  ( 2.072287782118878319, 0.000000000000000000, -2.950529333540147015 ) ) ;
#13512 = CARTESIAN_POINT ( 'NONE',  ( -16.81345671998191449, 0.000000000000000000, 3.412238694616132495 ) ) ;
#13513 = CARTESIAN_POINT ( 'NONE',  ( 2.072287782118878319, 0.000000000000000000, -2.950529333540147015 ) ) ;
#13514 = LINE ( 'NONE', #9538, #27616 ) ;
#13515 = CARTESIAN_POINT ( 'NONE',  ( -13.57018763683711349, 24.82352436079930769, -3.618365315326378173 ) ) ;
#13516 = DIRECTION ( 'NONE',  ( 0.000000000000000000, -0.000000000000000000, -1.000000000000000000 ) ) ;
#13517 = B_SPLINE_CURVE_WITH_KNOTS ( 'NONE', 3,
 ( #36701, #6887, #49490, #6589 ),
 .UNSPECIFIED., .F., .F.,
 ( 4, 4 ),
 ( 0.000000000000000000, 0.0003539001916872983413 ),
 .UNSPECIFIED. ) ;
#13518 = DIRECTION ( 'NONE',  ( -0.5364919789714478471, 0.6444004775717705469, -0.5449076811759709926 ) ) ;
#13519 = CARTESIAN_POINT ( 'NONE',  ( -15.81295127592206207, 0.000000000000000000, 6.174675361559132547 ) ) ;
#13520 = ORIENTED_EDGE ( 'NONE', *, *, #52466, .T. ) ;
#13521 = DIRECTION ( 'NONE',  ( -0.005961354470445682716, -0.6427876096865404731, 0.7660212471507180654 ) ) ;
#13522 = ORIENTED_EDGE ( 'NONE', *, *, #26190, .T. ) ;
#13523 = DIRECTION ( 'NONE',  ( 0.5449076811759707706, 0.6444004775717708799, -0.5364919789714476250 ) ) ;
#13524 = DIRECTION ( 'NONE',  ( -0.5364919789714478471, 0.6444004775717705469, -0.5449076811759709926 ) ) ;
#13525 = ORIENTED_EDGE ( 'NONE', *, *, #36149, .F. ) ;
#13526 = EDGE_CURVE ( 'NONE', #34394, #55847, #31165, .T. ) ;
#13527 = ORIENTED_EDGE ( 'NONE', *, *, #50191, .T. ) ;
#13528 = ORIENTED_EDGE ( 'NONE', *, *, #53716, .F. ) ;
#13529 = ORIENTED_EDGE ( 'NONE', *, *, #39668, .T. ) ;
#13530 = EDGE_LOOP ( 'NONE', ( #3350, #27718, #15271 ) ) ;
#13531 = VERTEX_POINT ( 'NONE', #48490 ) ;
#13532 = LINE ( 'NONE', #47048, #7745 ) ;
#13533 = FACE_OUTER_BOUND ( 'NONE', #39035, .T. ) ;
#13534 = PLANE ( 'NONE',  #9531 ) ;
#13535 = EDGE_CURVE ( 'NONE', #2679, #49846, #13312, .T. ) ;
#13536 = ORIENTED_EDGE ( 'NONE', *, *, #16953, .T. ) ;
#13537 = FACE_OUTER_BOUND ( 'NONE', #19354, .T. ) ;
#13538 = ORIENTED_EDGE ( 'NONE', *, *, #9170, .F. ) ;
#13539 = ADVANCED_FACE ( 'NONE', ( #52733 ), #30637, .F. ) ;
#13540 = ORIENTED_EDGE ( 'NONE', *, *, #53904, .T. ) ;
#13541 = ADVANCED_FACE ( 'NONE', ( #35719 ), #26094, .F. ) ;
#13542 = DIRECTION ( 'NONE',  ( 0.000000000000000000, -0.000000000000000000, -1.000000000000000000 ) ) ;
#13543 = CARTESIAN_POINT ( 'NONE',  ( -13.08486533123210194, 0.000000000000000000, 1.963927175729152541 ) ) ;
#13544 = LINE ( 'NONE', #26313, #32285 ) ;
#13545 = ADVANCED_FACE ( 'NONE', ( #51896 ), #9035, .F. ) ;
#13546 = ORIENTED_EDGE ( 'NONE', *, *, #38039, .F. ) ;
#13547 = LINE ( 'NONE', #24018, #9251 ) ;
#13548 = EDGE_LOOP ( 'NONE', ( #26724, #5008, #27900, #18767 ) ) ;
#13549 = DIRECTION ( 'NONE',  ( 0.000000000000000000, -0.000000000000000000, -1.000000000000000000 ) ) ;
#13550 = ADVANCED_FACE ( 'NONE', ( #4767 ), #43399, .F. ) ;
#13551 = DIRECTION ( 'NONE',  ( 0.6427681459581294776, -0.7660444431189769032, 0.005002170337467562802 ) ) ;
#13552 = ADVANCED_FACE ( 'NONE', ( #202 ), #26625, .F. ) ;
#13553 = LINE ( 'NONE', #36006, #38731 ) ;
#13554 = DIRECTION ( 'NONE',  ( -0.5449076811759708816, 0.6444004775717707689, 0.5364919789714475140 ) ) ;
#13555 = DIRECTION ( 'NONE',  ( 0.5364919789714477361, 0.6444004775717706579, 0.5449076811759711036 ) ) ;
#13556 = CARTESIAN_POINT ( 'NONE',  ( 5.519498461031219882, -1.055017498708691992, -2.502222228327667608 ) ) ;
#13557 = CARTESIAN_POINT ( 'NONE',  ( -19.96568551101100297, -0.1191753592594195360, 6.242360851625931240 ) ) ;
#13558 = DIRECTION ( 'NONE',  ( 0.007781995580012663651, -3.146120232559066537E-19, -0.9999697198139514409 ) ) ;
#13559 = ORIENTED_EDGE ( 'NONE', *, *, #32626, .T. ) ;
#13560 = PLANE ( 'NONE',  #219 ) ;
#13561 = ADVANCED_FACE ( 'NONE', ( #5067 ), #39711, .F. ) ;
#13562 = CARTESIAN_POINT ( 'NONE',  ( -24.26986129792355129, -0.1191753592594197858, 6.208864760408702388 ) ) ;
#13563 = DIRECTION ( 'NONE',  ( -0.005961354470445682716, -0.6427876096865404731, 0.7660212471507180654 ) ) ;
#13564 = DIRECTION ( 'NONE',  ( 0.6246952433987894571, -0.7422098413412800966, -0.2426528472758541777 ) ) ;
#13565 = CARTESIAN_POINT ( 'NONE',  ( -19.68185725454445034, 19.56289945424903109, -4.315709269779091528 ) ) ;
#13566 = DIRECTION ( 'NONE',  ( 0.005961354470445682716, -0.6427876096865404731, -0.7660212471507180654 ) ) ;
#13567 = DIRECTION ( 'NONE',  ( 0.007781995580012663651, 0.000000000000000000, -0.9999697198139515519 ) ) ;
#13568 = ADVANCED_FACE ( 'NONE', ( #47939 ), #43653, .F. ) ;
#13569 = CARTESIAN_POINT ( 'NONE',  ( -8.373012819454125122, 0.000000000000000000, 5.493910543331755214 ) ) ;
#13570 = VERTEX_POINT ( 'NONE', #27190 ) ;
#13571 = DIRECTION ( 'NONE',  ( 0.005961354470445682716, -0.6427876096865404731, -0.7660212471507180654 ) ) ;
#13572 = DIRECTION ( 'NONE',  ( -0.005961354470445682716, -0.6427876096865404731, 0.7660212471507180654 ) ) ;
#13573 = DIRECTION ( 'NONE',  ( -0.5364919789714478471, 0.6444004775717705469, -0.5449076811759709926 ) ) ;
#13574 = PRODUCT_DEFINITION_FORMATION_WITH_SPECIFIED_SOURCE ( 'ANY', '', #31892, .NOT_KNOWN. ) ;
#13575 = DIRECTION ( 'NONE',  ( 0.000000000000000000, 0.000000000000000000, 1.000000000000000000 ) ) ;
#13576 = CARTESIAN_POINT ( 'NONE',  ( -4.092399949646539525, 6.327196921604587132, -1.628746456733796588 ) ) ;
#13577 = CARTESIAN_POINT ( 'NONE',  ( -11.16239059961664282, 0.000000000000000000, 5.672209016686486471 ) ) ;
#13578 = FACE_OUTER_BOUND ( 'NONE', #18712, .T. ) ;
#13579 = CARTESIAN_POINT ( 'NONE',  ( -68.13541175005632056, -9.641814632260039986, 5.527125342194959323 ) ) ;
#13580 = CARTESIAN_POINT ( 'NONE',  ( 0.1285714285714289751, 0.000000000000000000, 5.998622290806042479 ) ) ;
#13581 = VERTEX_POINT ( 'NONE', #18106 ) ;
#13582 = ADVANCED_FACE ( 'NONE', ( #48191 ), #13839, .F. ) ;
#13583 = ORIENTED_EDGE ( 'NONE', *, *, #43562, .T. ) ;
#13584 = ORIENTED_EDGE ( 'NONE', *, *, #4207, .T. ) ;
#13585 = VERTEX_POINT ( 'NONE', #39964 ) ;
#13586 = ORIENTED_EDGE ( 'NONE', *, *, #13750, .F. ) ;
#13587 = DIRECTION ( 'NONE',  ( -0.005961354470445682716, -0.6427876096865404731, 0.7660212471507180654 ) ) ;
#13588 = CARTESIAN_POINT ( 'NONE',  ( 2.072287782118878319, 0.000000000000000000, -2.950529333540147015 ) ) ;
#13589 = ORIENTED_EDGE ( 'NONE', *, *, #13981, .T. ) ;
#13590 = ORIENTED_EDGE ( 'NONE', *, *, #39887, .T. ) ;
#13591 = ADVANCED_FACE ( 'NONE', ( #28583 ), #14975, .F. ) ;
#13592 = CARTESIAN_POINT ( 'NONE',  ( -13.01075962734913816, 0.000000000000000000, 4.349822315878366652 ) ) ;
#13593 = ORIENTED_EDGE ( 'NONE', *, *, #38818, .F. ) ;
#13594 = CARTESIAN_POINT ( 'NONE',  ( -10.94028622754223967, 0.000000000000000000, 11.14038480894692995 ) ) ;
#13595 = FACE_OUTER_BOUND ( 'NONE', #45166, .T. ) ;
#13596 = ORIENTED_EDGE ( 'NONE', *, *, #44046, .F. ) ;
#13597 = CARTESIAN_POINT ( 'NONE',  ( -13.07066190154808361, 0.000000000000000000, 12.04713590736729678 ) ) ;
#13598 = ORIENTED_EDGE ( 'NONE', *, *, #13909, .F. ) ;
#13599 = CARTESIAN_POINT ( 'NONE',  ( -14.00280974873554030, 0.000000000000000000, 12.40921378708904044 ) ) ;
#13600 = ADVANCED_FACE ( 'NONE', ( #49330 ), #23755, .F. ) ;
#13601 = CARTESIAN_POINT ( 'NONE',  ( -9.908559390481867624, 0.8026771090238171702, 1.484425475346726531 ) ) ;
#13602 = ADVANCED_FACE ( 'NONE', ( #45341 ), #45907, .F. ) ;
#13603 = LINE ( 'NONE', #1383, #48154 ) ;
#13604 = LINE ( 'NONE', #15995, #11520 ) ;
#13605 = EDGE_LOOP ( 'NONE', ( #38883, #26444, #43453, #9739 ) ) ;
#13606 = CARTESIAN_POINT ( 'NONE',  ( -19.59569683186026268, 0.000000000000000000, 14.58168106541950948 ) ) ;
#13607 = CARTESIAN_POINT ( 'NONE',  ( -25.25174164940481347, 18.07917600709017947, 4.578957096563475382 ) ) ;
#13608 = CARTESIAN_POINT ( 'NONE',  ( -24.26986129792355129, -0.1191753592594197858, 6.208864760408702388 ) ) ;
#13609 = EDGE_LOOP ( 'NONE', ( #37087, #15934, #10252, #50325 ) ) ;
#13610 = CARTESIAN_POINT ( 'NONE',  ( -9.808144436391993182, 0.000000000000000000, 10.77986332834118777 ) ) ;
#13611 = ORIENTED_EDGE ( 'NONE', *, *, #34885, .T. ) ;
#13612 = EDGE_CURVE ( 'NONE', #36877, #17353, #41077, .T. ) ;
#13613 = DIRECTION ( 'NONE',  ( 0.9999697198139515519, 0.000000000000000000, 0.007781995580013368816 ) ) ;
#13614 = DIRECTION ( 'NONE',  ( 0.9999697198139515519, 0.000000000000000000, 0.007781995580013368816 ) ) ;
#13615 = CARTESIAN_POINT ( 'NONE',  ( -12.12632416399392277, 0.9340140483890049250, 3.124473410292289977 ) ) ;
#13616 = DIRECTION ( 'NONE',  ( 0.007781995580012662783, 0.000000000000000000, -0.9999697198139514409 ) ) ;
#13617 = LINE ( 'NONE', #5658, #12319 ) ;
#13618 = DIRECTION ( 'NONE',  ( 0.9321478471874541372, 0.000000000000000000, -0.3620778797217453771 ) ) ;
#13619 = DIRECTION ( 'NONE',  ( -0.6427681459581293666, -0.7660444431189770143, -0.005002170337467561935 ) ) ;
#13620 = EDGE_CURVE ( 'NONE', #52907, #21716, #27768, .T. ) ;
#13621 = CARTESIAN_POINT ( 'NONE',  ( -16.71867036141801677, -5.536956232915664522, 3.198762561013173578 ) ) ;
#13622 = LINE ( 'NONE', #26397, #35972 ) ;
#13623 = ORIENTED_EDGE ( 'NONE', *, *, #33996, .F. ) ;
#13624 = DIRECTION ( 'NONE',  ( -0.9999697198139514409, -0.000000000000000000, -0.007781995580013368816 ) ) ;
#13625 = DIRECTION ( 'NONE',  ( 0.007781995580012663651, -3.146120232559066537E-19, -0.9999697198139514409 ) ) ;
#13626 = B_SPLINE_CURVE_WITH_KNOTS ( 'NONE', 3,
 ( #5307, #22618, #14105, #10696 ),
 .UNSPECIFIED., .F., .F.,
 ( 4, 4 ),
 ( 0.000000000000000000, 0.0003539001916874550085 ),
 .UNSPECIFIED. ) ;
#13627 = CARTESIAN_POINT ( 'NONE',  ( -10.37421533196711465, -0.1191753592594197858, 10.96012406864405975 ) ) ;
#13628 = CARTESIAN_POINT ( 'NONE',  ( -23.23471098716119698, 19.24370920290025566, -4.480780584866845828 ) ) ;
#13629 = CARTESIAN_POINT ( 'NONE',  ( 2.072287782118878319, 0.000000000000000000, -2.950529333540147015 ) ) ;
#13630 = FACE_OUTER_BOUND ( 'NONE', #50473, .T. ) ;
#13631 = EDGE_LOOP ( 'NONE', ( #41595, #45974, #702, #39846, #5372 ) ) ;
#13632 = VECTOR ( 'NONE', #32603, 1000.000000000000227 ) ;
#13633 = ORIENTED_EDGE ( 'NONE', *, *, #1326, .T. ) ;
#13634 = DIRECTION ( 'NONE',  ( 0.007781995580012662783, 0.000000000000000000, -0.9999697198139514409 ) ) ;
#13635 = DIRECTION ( 'NONE',  ( 0.005961354470445682716, -0.6427876096865404731, -0.7660212471507180654 ) ) ;
#13636 = EDGE_CURVE ( 'NONE', #29728, #21771, #1340, .T. ) ;
#13637 = ORIENTED_EDGE ( 'NONE', *, *, #45357, .F. ) ;
#13638 = CARTESIAN_POINT ( 'NONE',  ( -13.53673582514181106, 0.000000000000000000, 12.22817484722816772 ) ) ;
#13639 = EDGE_CURVE ( 'NONE', #34394, #36809, #14429, .T. ) ;
#13640 = ORIENTED_EDGE ( 'NONE', *, *, #47235, .T. ) ;
#13641 = DIRECTION ( 'NONE',  ( 0.007781995580012663651, 0.000000000000000000, -0.9999697198139515519 ) ) ;
#13642 = ORIENTED_EDGE ( 'NONE', *, *, #9842, .T. ) ;
#13643 = ORIENTED_EDGE ( 'NONE', *, *, #13650, .F. ) ;
#13644 = ADVANCED_FACE ( 'NONE', ( #27464 ), #37108, .F. ) ;
#13645 = ORIENTED_EDGE ( 'NONE', *, *, #52981, .F. ) ;
#13646 = ADVANCED_FACE ( 'NONE', ( #18962 ), #28294, .F. ) ;
#13647 = DIRECTION ( 'NONE',  ( -0.6427681459581293666, -0.7660444431189770143, -0.005002170337467561935 ) ) ;
#13648 = DIRECTION ( 'NONE',  ( -0.005002170337468016433, -0.7660444431189770143, 0.6427681459581293666 ) ) ;
#13649 = DIRECTION ( 'NONE',  ( -0.000000000000000000, -0.000000000000000000, 1.000000000000000000 ) ) ;
#13650 = EDGE_CURVE ( 'NONE', #26046, #18030, #10730, .T. ) ;
#13651 = ADVANCED_FACE ( 'NONE', ( #23228 ), #19209, .F. ) ;
#13652 = EDGE_CURVE ( 'NONE', #50299, #55191, #36279, .T. ) ;
#13653 = CARTESIAN_POINT ( 'NONE',  ( -1.148821818165424169, 4.447699752827971587, 3.664614983992416697 ) ) ;
#13654 = VERTEX_POINT ( 'NONE', #41378 ) ;
#13655 = ORIENTED_EDGE ( 'NONE', *, *, #46961, .T. ) ;
#13656 = FACE_OUTER_BOUND ( 'NONE', #30693, .T. ) ;
#13657 = ORIENTED_EDGE ( 'NONE', *, *, #48211, .F. ) ;
#13658 = CARTESIAN_POINT ( 'NONE',  ( -15.03495456790438389, -0.1191753592594197858, 12.77051346725278158 ) ) ;
#13659 = ORIENTED_EDGE ( 'NONE', *, *, #2622, .T. ) ;
#13660 = PLANE ( 'NONE',  #5181 ) ;
#13661 = PLANE ( 'NONE',  #38481 ) ;
#13662 = VERTEX_POINT ( 'NONE', #6451 ) ;
#13663 = VECTOR ( 'NONE', #43764, 1000.000000000000000 ) ;
#13664 = LINE ( 'NONE', #30980, #20453 ) ;
#13665 = EDGE_CURVE ( 'NONE', #9855, #50386, #53333, .T. ) ;
#13666 = ORIENTED_EDGE ( 'NONE', *, *, #46538, .T. ) ;
#13667 = VECTOR ( 'NONE', #37508, 1000.000000000000000 ) ;
#13668 = EDGE_CURVE ( 'NONE', #33376, #49938, #14686, .T. ) ;
#13669 = DIRECTION ( 'NONE',  ( 0.5449076811759707706, 0.6444004775717708799, -0.5364919789714476250 ) ) ;
#13670 = ORIENTED_EDGE ( 'NONE', *, *, #54894, .F. ) ;
#13671 = DIRECTION ( 'NONE',  ( -0.5364919789714478471, 0.6444004775717705469, -0.5449076811759709926 ) ) ;
#13672 = LINE ( 'NONE', #39810, #14835 ) ;
#13673 = ADVANCED_FACE ( 'NONE', ( #45612 ), #11258, .F. ) ;
#13674 = LINE ( 'NONE', #30166, #1959 ) ;
#13675 = ORIENTED_EDGE ( 'NONE', *, *, #36843, .T. ) ;
#13676 = DIRECTION ( 'NONE',  ( 0.6246952433987893460, 0.7422098413412802076, -0.2426528472758539279 ) ) ;
#13677 = EDGE_CURVE ( 'NONE', #49612, #38385, #36026, .T. ) ;
#13678 = CARTESIAN_POINT ( 'NONE',  ( -26.13337879274045505, 0.000000000000000000, 6.833023547870798353 ) ) ;
#13679 = CARTESIAN_POINT ( 'NONE',  ( -16.01608722591203104, -3.594132820645663084, 2.987841650007617922 ) ) ;
#13680 = DIRECTION ( 'NONE',  ( -0.005002170337468016433, -0.7660444431189770143, 0.6427681459581293666 ) ) ;
#13681 = CARTESIAN_POINT ( 'NONE',  ( -13.27065584551087163, 0.000000000000000000, 12.04557950825129176 ) ) ;
#13682 = CARTESIAN_POINT ( 'NONE',  ( -23.33771345073609638, -0.1191753592594197858, 5.846786880686956955 ) ) ;
#13683 = FACE_OUTER_BOUND ( 'NONE', #34715, .T. ) ;
#13684 = ORIENTED_EDGE ( 'NONE', *, *, #97, .T. ) ;
#13685 = CARTESIAN_POINT ( 'NONE',  ( -1.086233639165236964, 0.000000000000000000, -2.796443541562362078 ) ) ;
#13686 = FACE_OUTER_BOUND ( 'NONE', #7393, .T. ) ;
#13687 = CARTESIAN_POINT ( 'NONE',  ( -8.378760926464691394, 0.000000000000000000, 6.232529949847283923 ) ) ;
#13688 = ORIENTED_EDGE ( 'NONE', *, *, #19549, .F. ) ;
#13689 = ADVANCED_FACE ( 'NONE', ( #41633 ), #29425, .F. ) ;
#13690 = DIRECTION ( 'NONE',  ( 0.5364919789714477361, 0.6444004775717706579, 0.5449076811759711036 ) ) ;
#13691 = DIRECTION ( 'NONE',  ( 0.7660212471507180654, -0.6427876096865404731, 0.005961354470445141482 ) ) ;
#13692 =( REPRESENTATION_RELATIONSHIP ('NONE','NONE', #51076, #53575 ) REPRESENTATION_RELATIONSHIP_WITH_TRANSFORMATION ( #34034 )SHAPE_REPRESENTATION_RELATIONSHIP( ) );
#13693 = EDGE_LOOP ( 'NONE', ( #45961, #27960, #11273, #39598 ) ) ;
#13694 = CARTESIAN_POINT ( 'NONE',  ( -31.72782227498118601, 0.000000000000000000, 9.205484770164058972 ) ) ;
#13695 = AXIS2_PLACEMENT_3D ( 'NONE', #8847, #44017, #22461 ) ;
#13696 = AXIS2_PLACEMENT_3D ( 'NONE', #41721, #54499, #2812 ) ;
#13697 = CARTESIAN_POINT ( 'NONE',  ( -21.47419595591918906, 0.000000000000000000, 5.222628093224860102 ) ) ;
#13698 = LINE ( 'NONE', #26215, #35054 ) ;
#13699 = CARTESIAN_POINT ( 'NONE',  ( -11.40636015113596180, 0.000000000000000000, 11.32142374880780089 ) ) ;
#13700 = ORIENTED_EDGE ( 'NONE', *, *, #51420, .F. ) ;
#13701 = ORIENTED_EDGE ( 'NONE', *, *, #52407, .F. ) ;
#13702 = LINE ( 'NONE', #10009, #45753 ) ;
#13703 = FACE_OUTER_BOUND ( 'NONE', #8353, .T. ) ;
#13704 = CARTESIAN_POINT ( 'NONE',  ( -67.50702643244157741, 2.000000000000000000, -7.448289400635801805 ) ) ;
#13705 = CARTESIAN_POINT ( 'NONE',  ( -14.84211576094791418, 4.657758921906509642, 10.29067882608070761 ) ) ;
#13706 = CARTESIAN_POINT ( 'NONE',  ( -17.83139810946674686, -0.1191753592594197858, 13.85674710641801788 ) ) ;
#13707 = VECTOR ( 'NONE', #52509, 1000.000000000000227 ) ;
#13708 = FACE_OUTER_BOUND ( 'NONE', #32863, .T. ) ;
#13709 = ORIENTED_EDGE ( 'NONE', *, *, #46692, .F. ) ;
#13710 = LINE ( 'NONE', #9459, #10206 ) ;
#13711 = AXIS2_PLACEMENT_3D ( 'NONE', #1410, #41445, #2526 ) ;
#13712 = CARTESIAN_POINT ( 'NONE',  ( -13.63673279712320507, -0.1191753592594197858, 12.22739664767016521 ) ) ;
#13713 = EDGE_LOOP ( 'NONE', ( #31241, #20141, #13643, #50398 ) ) ;
#13714 = CARTESIAN_POINT ( 'NONE',  ( -15.34124861768113135, 0.000000000000000000, 5.270356107516636968 ) ) ;
#13715 = DIRECTION ( 'NONE',  ( 0.007781995580012662783, 0.000000000000000000, -0.9999697198139514409 ) ) ;
#13716 = DIRECTION ( 'NONE',  ( 0.007781995580012663651, -3.146120232559066537E-19, -0.9999697198139514409 ) ) ;
#13717 = EDGE_CURVE ( 'NONE', #43487, #24159, #54742, .T. ) ;
#13718 = EDGE_CURVE ( 'NONE', #52808, #34831, #25185, .T. ) ;
#13719 = ORIENTED_EDGE ( 'NONE', *, *, #41312, .T. ) ;
#13720 = LINE ( 'NONE', #49197, #29267 ) ;
#13721 = ORIENTED_EDGE ( 'NONE', *, *, #2027, .F. ) ;
#13722 = EDGE_CURVE ( 'NONE', #39978, #308, #38208, .T. ) ;
#13723 = ORIENTED_EDGE ( 'NONE', *, *, #31406, .T. ) ;
#13724 = ORIENTED_EDGE ( 'NONE', *, *, #24417, .T. ) ;
#13725 = ORIENTED_EDGE ( 'NONE', *, *, #39119, .T. ) ;
#13726 = CARTESIAN_POINT ( 'NONE',  ( -14.71120258492120136, -1.489407457353158160, 2.548131899913917309 ) ) ;
#13727 = ORIENTED_EDGE ( 'NONE', *, *, #21238, .T. ) ;
#13728 = DIRECTION ( 'NONE',  ( 0.000000000000000000, -0.000000000000000000, -1.000000000000000000 ) ) ;
#13729 = LINE ( 'NONE', #31050, #32231 ) ;
#13730 = AXIS2_PLACEMENT_3D ( 'NONE', #38927, #26150, #26996 ) ;
#13731 = AXIS2_PLACEMENT_3D ( 'NONE', #7671, #11913, #50260 ) ;
#13732 = ORIENTED_EDGE ( 'NONE', *, *, #39892, .T. ) ;
#13733 = DIRECTION ( 'NONE',  ( 0.9999697198139515519, 0.000000000000000000, 0.007781995580013368816 ) ) ;
#13734 = ORIENTED_EDGE ( 'NONE', *, *, #14316, .F. ) ;
#13735 = LINE ( 'NONE', #39613, #2129 ) ;
#13736 = EDGE_LOOP ( 'NONE', ( #22471, #13386, #31384, #51170 ) ) ;
#13737 = PLANE ( 'NONE',  #21037 ) ;
#13738 = CARTESIAN_POINT ( 'NONE',  ( -23.33771345073609638, -0.1191753592594197858, 5.846786880686956955 ) ) ;
#13739 = VECTOR ( 'NONE', #22861, 1000.000000000000227 ) ;
#13740 = LINE ( 'NONE', #950, #10552 ) ;
#13741 = FACE_OUTER_BOUND ( 'NONE', #52868, .T. ) ;
#13742 = EDGE_CURVE ( 'NONE', #52840, #33489, #37947, .T. ) ;
#13743 = CARTESIAN_POINT ( 'NONE',  ( -15.50102849149811135, -0.1191753592594197858, 12.95155240711365430 ) ) ;
#13744 = CARTESIAN_POINT ( 'NONE',  ( -11.19417631680646963, 0.9340140483890049250, 2.762395530570545432 ) ) ;
#13745 = ORIENTED_EDGE ( 'NONE', *, *, #41169, .F. ) ;
#13747 = EDGE_LOOP ( 'NONE', ( #25210, #8223, #11019, #4049 ) ) ;
#13746 = EDGE_CURVE ( 'NONE', #17943, #41770, #34263, .T. ) ;
#13748 = LINE ( 'NONE', #31067, #24932 ) ;
#13749 = DIRECTION ( 'NONE',  ( 0.6427681459581294776, -0.7660444431189769032, 0.005002170337467562802 ) ) ;
#13750 = EDGE_CURVE ( 'NONE', #49112, #18253, #11810, .T. ) ;
#13751 = AXIS2_PLACEMENT_3D ( 'NONE', #23855, #20140, #37473 ) ;
#13752 = CARTESIAN_POINT ( 'NONE',  ( -15.55405643005433269, 0.000000000000000000, 6.915354280726666580 ) ) ;
#13753 = FACE_OUTER_BOUND ( 'NONE', #5721, .T. ) ;
#13754 = ORIENTED_EDGE ( 'NONE', *, *, #21921, .F. ) ;
#13755 = LINE ( 'NONE', #38482, #17680 ) ;
#13756 = DIRECTION ( 'NONE',  ( -0.6427681459581293666, -0.7660444431189770143, -0.005002170337467561935 ) ) ;
#13757 = EDGE_LOOP ( 'NONE', ( #48526, #31106, #18793, #7022 ) ) ;
#13758 = CARTESIAN_POINT ( 'NONE',  ( -3.335658863730355694, -6.482724466489810489, -1.922690393539094433 ) ) ;
#13759 = DIRECTION ( 'NONE',  ( 0.7660212471507180654, -0.6427876096865404731, 0.005961354470445141482 ) ) ;
#13760 = ORIENTED_EDGE ( 'NONE', *, *, #21688, .F. ) ;
#13761 = DIRECTION ( 'NONE',  ( -0.5364919789714478471, 0.6444004775717705469, -0.5449076811759709926 ) ) ;
#13762 = DIRECTION ( 'NONE',  ( 0.5449076811759707706, 0.6444004775717708799, -0.5364919789714476250 ) ) ;
#13763 = DIRECTION ( 'NONE',  ( 0.007781995580012663651, -3.146120232559066537E-19, -0.9999697198139514409 ) ) ;
#13764 = CARTESIAN_POINT ( 'NONE',  ( -18.80519705355265003, 0.000000000000000000, 6.720727139055624022 ) ) ;
#13765 = CARTESIAN_POINT ( 'NONE',  ( -58.00000000000000711, -9.250000000000000000, 7.102951435054649637E-15 ) ) ;
#13766 = ORIENTED_EDGE ( 'NONE', *, *, #13718, .T. ) ;
#13767 = ORIENTED_EDGE ( 'NONE', *, *, #14949, .T. ) ;
#13768 = DIRECTION ( 'NONE',  ( -0.5364919789714478471, 0.6444004775717705469, -0.5449076811759709926 ) ) ;
#13769 = LINE ( 'NONE', #433, #10487 ) ;
#13770 = DIRECTION ( 'NONE',  ( -0.6427681459581293666, -0.7660444431189770143, -0.005002170337467561935 ) ) ;
#13771 = VECTOR ( 'NONE', #40816, 1000.000000000000227 ) ;
#13772 = VECTOR ( 'NONE', #52577, 1000.000000000000114 ) ;
#13773 = LINE ( 'NONE', #1573, #54528 ) ;
#13774 = CARTESIAN_POINT ( 'NONE',  ( 2.072287782118878319, 0.000000000000000000, -2.950529333540147015 ) ) ;
#13775 = ORIENTED_EDGE ( 'NONE', *, *, #20888, .F. ) ;
#13776 = CARTESIAN_POINT ( 'NONE',  ( -18.26849638870942272, -0.1191753592594162470, 10.31447797378732645 ) ) ;
#13777 = LINE ( 'NONE', #47293, #26585 ) ;
#13778 = LINE ( 'NONE', #22328, #52275 ) ;
#13779 = DIRECTION ( 'NONE',  ( -0.005002170337468016433, -0.7660444431189770143, 0.6427681459581293666 ) ) ;
#13780 = VECTOR ( 'NONE', #30274, 999.9999999999998863 ) ;
#13781 = VERTEX_POINT ( 'NONE', #12669 ) ;
#13782 = FACE_OUTER_BOUND ( 'NONE', #23856, .T. ) ;
#13783 = ORIENTED_EDGE ( 'NONE', *, *, #19698, .F. ) ;
#13784 = DIRECTION ( 'NONE',  ( 0.007781995580012662783, 0.000000000000000000, -0.9999697198139514409 ) ) ;
#13785 = DIRECTION ( 'NONE',  ( 0.005002170337468016433, -0.7660444431189770143, -0.6427681459581293666 ) ) ;
#13786 = ADVANCED_FACE ( 'NONE', ( #54996 ), #47284, .F. ) ;
#13787 = ORIENTED_EDGE ( 'NONE', *, *, #5747, .T. ) ;
#13788 = CARTESIAN_POINT ( 'NONE',  ( -15.87975247367846166, 0.000000000000000000, 2.850166870931599927 ) ) ;
#13789 = VECTOR ( 'NONE', #2143, 999.9999999999998863 ) ;
#13790 = ORIENTED_EDGE ( 'NONE', *, *, #49126, .F. ) ;
#13791 = ADVANCED_FACE ( 'NONE', ( #29129 ), #11555, .F. ) ;
#13792 = ADVANCED_FACE ( 'NONE', ( #24583 ), #16634, .F. ) ;
#13793 = VECTOR ( 'NONE', #36182, 1000.000000000000227 ) ;
#13794 = ORIENTED_EDGE ( 'NONE', *, *, #30562, .F. ) ;
#13795 = ORIENTED_EDGE ( 'NONE', *, *, #49122, .F. ) ;
#13796 = DIRECTION ( 'NONE',  ( 0.7660212471507180654, -0.6427876096865404731, 0.005961354470445141482 ) ) ;
#13797 = ORIENTED_EDGE ( 'NONE', *, *, #30848, .F. ) ;
#13798 = ORIENTED_EDGE ( 'NONE', *, *, #56000, .T. ) ;
#13799 = DIRECTION ( 'NONE',  ( -0.5364919789714478471, 0.6444004775717705469, -0.5449076811759709926 ) ) ;
#13800 = CARTESIAN_POINT ( 'NONE',  ( -19.60495096914714708, 3.686347215771508257, 10.54647366380701712 ) ) ;
#13801 = VERTEX_POINT ( 'NONE', #55254 ) ;
#13802 = ORIENTED_EDGE ( 'NONE', *, *, #40713, .T. ) ;
#13803 = LINE ( 'NONE', #40213, #43069 ) ;
#13804 = ORIENTED_EDGE ( 'NONE', *, *, #41368, .F. ) ;
#13805 = ORIENTED_EDGE ( 'NONE', *, *, #32454, .F. ) ;
#13806 = PLANE ( 'NONE',  #22034 ) ;
#13807 = CARTESIAN_POINT ( 'NONE',  ( -32.10901097986136676, -1.000000000000000000, 16.76339505873265168 ) ) ;
#13808 = DIRECTION ( 'NONE',  ( 0.007781995580012663651, 0.000000000000000000, -0.9999697198139515519 ) ) ;
#13809 = AXIS2_PLACEMENT_3D ( 'NONE', #5965, #36327, #55594 ) ;
#13810 = ORIENTED_EDGE ( 'NONE', *, *, #21630, .T. ) ;
#13811 = CARTESIAN_POINT ( 'NONE',  ( -13.27065584551087163, 0.000000000000000000, 12.04557950825129176 ) ) ;
#13812 = VERTEX_POINT ( 'NONE', #50981 ) ;
#13813 = VECTOR ( 'NONE', #8072, 999.9999999999998863 ) ;
#13814 = VECTOR ( 'NONE', #23801, 1000.000000000000227 ) ;
#13815 = CARTESIAN_POINT ( 'NONE',  ( 0.4518049228021099872, -3.655895688227116747, -5.998622290806042479 ) ) ;
#13816 = ADVANCED_FACE ( 'NONE', ( #29732 ), #46172, .F. ) ;
#13817 = PLANE ( 'NONE',  #46942 ) ;
#13818 = VECTOR ( 'NONE', #54167, 1000.000000000000114 ) ;
#13819 = VECTOR ( 'NONE', #5726, 1000.000000000000227 ) ;
#13820 = LINE ( 'NONE', #26910, #22247 ) ;
#13821 = CARTESIAN_POINT ( 'NONE',  ( -14.85263745873890606, -3.270328918600659218, 7.818367421078713519 ) ) ;
#13822 = EDGE_CURVE ( 'NONE', #46922, #51942, #47029, .T. ) ;
#13823 = FACE_OUTER_BOUND ( 'NONE', #14172, .T. ) ;
#13824 = DIRECTION ( 'NONE',  ( 0.9999697198139515519, 0.000000000000000000, 0.007781995580013368816 ) ) ;
#13825 = DIRECTION ( 'NONE',  ( 0.5449076811759707706, 0.6444004775717708799, -0.5364919789714476250 ) ) ;
#13826 = ORIENTED_EDGE ( 'NONE', *, *, #38926, .T. ) ;
#13827 = PLANE ( 'NONE',  #32903 ) ;
#13828 = CARTESIAN_POINT ( 'NONE',  ( -28.92982233430281980, 0.000000000000000000, 7.919257187036034651 ) ) ;
#13829 = CARTESIAN_POINT ( 'NONE',  ( -27.06552663992790997, 0.000000000000000000, 7.195101427592543786 ) ) ;
#13830 = DIRECTION ( 'NONE',  ( 0.8531650599175527594, 0.4028455766673922356, -0.3313982828793700652 ) ) ;
#13831 = EDGE_CURVE ( 'NONE', #55458, #31864, #20332, .T. ) ;
#13832 = AXIS2_PLACEMENT_3D ( 'NONE', #26522, #4411, #51801 ) ;
#13833 = CARTESIAN_POINT ( 'NONE',  ( -15.40229489717257394, 22.03370593329148264, -3.962133388944282686 ) ) ;
#13834 = CARTESIAN_POINT ( 'NONE',  ( -15.13495153988577968, 0.000000000000000000, 12.76973526769478084 ) ) ;
#13835 = CARTESIAN_POINT ( 'NONE',  ( -24.26908309836554878, 0.000000000000000000, 6.108867788427308376 ) ) ;
#13836 = PLANE ( 'NONE',  #46553 ) ;
#13837 = ORIENTED_EDGE ( 'NONE', *, *, #3032, .T. ) ;
#13838 = PLANE ( 'NONE',  #19369 ) ;
#13839 = PLANE ( 'NONE',  #14939 ) ;
#13840 = CARTESIAN_POINT ( 'NONE',  ( -19.26695989688845501, 0.000000000000000000, 6.347801524029851095 ) ) ;
#13841 = CARTESIAN_POINT ( 'NONE',  ( -16.99924723426068951, 0.000000000000000000, 13.49389102713827171 ) ) ;
#13842 = CARTESIAN_POINT ( 'NONE',  ( -13.07066190154808361, 0.000000000000000000, 12.04713590736729678 ) ) ;
#13843 = AXIS2_PLACEMENT_3D ( 'NONE', #22850, #48715, #9227 ) ;
#13844 = DIRECTION ( 'NONE',  ( 0.005961354470445682716, -0.6427876096865404731, -0.7660212471507180654 ) ) ;
#13845 = EDGE_CURVE ( 'NONE', #37525, #4654, #24880, .T. ) ;
#13846 = LINE ( 'NONE', #43405, #38330 ) ;
#13847 = DIRECTION ( 'NONE',  ( -0.5449076811759708816, 0.6444004775717707689, 0.5364919789714475140 ) ) ;
#13848 = AXIS2_PLACEMENT_3D ( 'NONE', #47228, #16291, #20270 ) ;
#13849 = CARTESIAN_POINT ( 'NONE',  ( -17.27808141480208803, -3.432230869623162928, 3.483208570362961609 ) ) ;
#13850 = EDGE_CURVE ( 'NONE', #28121, #13117, #26554, .T. ) ;
#13851 = AXIS2_PLACEMENT_3D ( 'NONE', #50458, #46753, #38216 ) ;
#13852 = VECTOR ( 'NONE', #31995, 999.9999999999998863 ) ;
#13853 = VERTEX_POINT ( 'NONE', #52120 ) ;
#13854 = ADVANCED_FACE ( 'NONE', ( #21746 ), #17779, .F. ) ;
#13855 = EDGE_CURVE ( 'NONE', #14660, #10075, #26028, .T. ) ;
#13856 = VECTOR ( 'NONE', #12882, 999.9999999999998863 ) ;
#13857 = ORIENTED_EDGE ( 'NONE', *, *, #44373, .F. ) ;
#13858 = ORIENTED_EDGE ( 'NONE', *, *, #18487, .F. ) ;
#13859 = EDGE_LOOP ( 'NONE', ( #23475, #28499, #33601, #31873 ) ) ;
#13860 = VERTEX_POINT ( 'NONE', #48416 ) ;
#13861 = FACE_OUTER_BOUND ( 'NONE', #36055, .T. ) ;
#13862 = PLANE ( 'NONE',  #21267 ) ;
#13863 = ORIENTED_EDGE ( 'NONE', *, *, #33593, .T. ) ;
#13864 = ORIENTED_EDGE ( 'NONE', *, *, #6636, .T. ) ;
#13865 = VECTOR ( 'NONE', #34931, 999.9999999999998863 ) ;
#13866 = VECTOR ( 'NONE', #37972, 1000.000000000000114 ) ;
#13867 = EDGE_CURVE ( 'NONE', #12052, #4182, #17471, .T. ) ;
#13868 = DIRECTION ( 'NONE',  ( -0.6427681459581293666, -0.7660444431189770143, -0.005002170337467561935 ) ) ;
#13869 = EDGE_LOOP ( 'NONE', ( #3205, #15959, #6526, #45416 ) ) ;
#13870 = FACE_OUTER_BOUND ( 'NONE', #53071, .T. ) ;
#13871 = DIRECTION ( 'NONE',  ( 0.5449076811759707706, 0.6444004775717708799, -0.5364919789714476250 ) ) ;
#13872 = EDGE_LOOP ( 'NONE', ( #55138, #3777, #8181, #13478 ) ) ;
#13873 = DIRECTION ( 'NONE',  ( -0.7660212471507179544, -0.6427876096865405842, -0.005961354470445141482 ) ) ;
#13874 = VECTOR ( 'NONE', #21720, 1000.000000000000114 ) ;
#13875 = ORIENTED_EDGE ( 'NONE', *, *, #5092, .F. ) ;
#13876 = CARTESIAN_POINT ( 'NONE',  ( -18.19747506107908563, 0.000000000000000000, 14.03856424583689311 ) ) ;
#13878 = FACE_OUTER_BOUND ( 'NONE', #47947, .T. ) ;
#13877 = VECTOR ( 'NONE', #11405, 1000.000000000000000 ) ;
#13879 = CARTESIAN_POINT ( 'NONE',  ( -14.53367362947859753, -0.1117717739993928788, 8.863745978987285667 ) ) ;
#13880 = LINE ( 'NONE', #31207, #50508 ) ;
#13881 = ORIENTED_EDGE ( 'NONE', *, *, #9039, .T. ) ;
#13882 = CARTESIAN_POINT ( 'NONE',  ( -12.57486326556087697, 0.000000000000000000, 8.046535260224020547 ) ) ;
#13883 = LINE ( 'NONE', #35216, #12989 ) ;
#13884 = CARTESIAN_POINT ( 'NONE',  ( -26.13337879274045505, 0.000000000000000000, 6.833023547870798353 ) ) ;
#13885 = ORIENTED_EDGE ( 'NONE', *, *, #13850, .T. ) ;
#13886 = CARTESIAN_POINT ( 'NONE',  ( -16.01869332689541991, 0.000000000000000000, 6.911738368958656231 ) ) ;
#13887 = ORIENTED_EDGE ( 'NONE', *, *, #17362, .F. ) ;
#13888 = AXIS2_PLACEMENT_3D ( 'NONE', #8136, #25442, #32838 ) ;
#13889 = VECTOR ( 'NONE', #6643, 1000.000000000000000 ) ;
#13890 = CARTESIAN_POINT ( 'NONE',  ( -16.26896601224730432, 0.000000000000000000, 5.063130340017827358 ) ) ;
#13891 = FACE_OUTER_BOUND ( 'NONE', #35329, .T. ) ;
#13892 = CARTESIAN_POINT ( 'NONE',  ( -16.61838873139687678, -3.756034771668162797, 3.216630489095766876 ) ) ;
#13893 = DIRECTION ( 'NONE',  ( 0.000000000000000000, 1.000000000000000000, 0.000000000000000000 ) ) ;
#13894 = ADVANCED_FACE ( 'NONE', ( #52957 ), #13237, .F. ) ;
#13895 = PLANE ( 'NONE',  #36853 ) ;
#13896 = PLANE ( 'NONE',  #42149 ) ;
#13897 = DIRECTION ( 'NONE',  ( 0.9321478471874541372, 0.000000000000000000, -0.3620778797217453771 ) ) ;
#13898 = VECTOR ( 'NONE', #29602, 999.9999999999998863 ) ;
#13899 = CARTESIAN_POINT ( 'NONE',  ( -31.72626587586518099, 0.000000000000000000, 9.005490826201270949 ) ) ;
#13900 = VECTOR ( 'NONE', #42347, 1000.000000000000227 ) ;
#13901 = CARTESIAN_POINT ( 'NONE',  ( -22.10562829171461274, -5.213152330870663320, 13.82417958061751051 ) ) ;
#13902 = ORIENTED_EDGE ( 'NONE', *, *, #8837, .T. ) ;
#13903 = CARTESIAN_POINT ( 'NONE',  ( -15.87975247367846166, 0.000000000000000000, 2.850166870931599927 ) ) ;
#13904 = CARTESIAN_POINT ( 'NONE',  ( -12.65008812213352485, 4.819660872929010687, 9.704929533543706910 ) ) ;
#13905 = DIRECTION ( 'NONE',  ( -0.005002170337468016433, -0.7660444431189770143, 0.6427681459581293666 ) ) ;
#13906 = PLANE ( 'NONE',  #16773 ) ;
#13907 = ADVANCED_FACE ( 'NONE', ( #43589 ), #725, .F. ) ;
#13908 = LINE ( 'NONE', #4834, #21879 ) ;
#13909 = EDGE_CURVE ( 'NONE', #12870, #40212, #21481, .T. ) ;
#13910 = DIRECTION ( 'NONE',  ( 0.005961354470445682716, -0.6427876096865404731, -0.7660212471507180654 ) ) ;
#13911 = EDGE_CURVE ( 'NONE', #35631, #43670, #26854, .T. ) ;
#13912 = DIRECTION ( 'NONE',  ( 0.005002170337468016433, -0.7660444431189770143, -0.6427681459581293666 ) ) ;
#13913 = ORIENTED_EDGE ( 'NONE', *, *, #41797, .F. ) ;
#13914 = EDGE_LOOP ( 'NONE', ( #38235, #3763, #46133 ) ) ;
#13915 = PLANE ( 'NONE',  #40492 ) ;
#13916 = DIRECTION ( 'NONE',  ( -0.02142857142857158143, 0.000000000000000000, -0.9997703818010067467 ) ) ;
#13917 = ADVANCED_FACE ( 'NONE', ( #47876 ), #22320, .F. ) ;
#13918 = AXIS2_PLACEMENT_3D ( 'NONE', #1026, #23205, #18355 ) ;
#13919 = ORIENTED_EDGE ( 'NONE', *, *, #51721, .T. ) ;
#13920 = EDGE_CURVE ( 'NONE', #21318, #25308, #35113, .T. ) ;
#13921 = CARTESIAN_POINT ( 'NONE',  ( -18.19747506107908563, 0.000000000000000000, 14.03856424583689311 ) ) ;
#13922 = VECTOR ( 'NONE', #43803, 999.9999999999998863 ) ;
#13923 = EDGE_LOOP ( 'NONE', ( #11, #25574, #25803, #9903 ) ) ;
#13924 = CARTESIAN_POINT ( 'NONE',  ( -18.62532148412685018, 0.000000000000000000, 9.307451460975977753 ) ) ;
#13925 = EDGE_CURVE ( 'NONE', #55181, #29912, #13769, .T. ) ;
#13926 = ORIENTED_EDGE ( 'NONE', *, *, #43235, .T. ) ;
#13927 = EDGE_LOOP ( 'NONE', ( #37831, #34663, #16727, #52980 ) ) ;
#13928 = EDGE_LOOP ( 'NONE', ( #12312, #691, #19905, #1295 ) ) ;
#13929 = FACE_OUTER_BOUND ( 'NONE', #39780, .T. ) ;
#13930 = VECTOR ( 'NONE', #35661, 1000.000000000000114 ) ;
#13931 = LINE ( 'NONE', #30137, #46829 ) ;
#13932 = CARTESIAN_POINT ( 'NONE',  ( -8.480943993241147894, -0.1191753592594194527, 6.512660236708999406 ) ) ;
#13933 = VECTOR ( 'NONE', #33862, 1000.000000000000227 ) ;
#13934 = EDGE_CURVE ( 'NONE', #44596, #56081, #48128, .T. ) ;
#13935 = VECTOR ( 'NONE', #197, 1000.000000000000114 ) ;
#13936 = LINE ( 'NONE', #5428, #17524 ) ;
#13937 = ORIENTED_EDGE ( 'NONE', *, *, #34493, .F. ) ;
#13938 = ORIENTED_EDGE ( 'NONE', *, *, #47578, .F. ) ;
#13939 = ADVANCED_FACE ( 'NONE', ( #44176 ), #9231, .F. ) ;
#13940 = VECTOR ( 'NONE', #18066, 1000.000000000000227 ) ;
#13941 = VECTOR ( 'NONE', #35487, 1000.000000000000000 ) ;
#13942 = LINE ( 'NONE', #48876, #32736 ) ;
#13943 = ORIENTED_EDGE ( 'NONE', *, *, #3204, .T. ) ;
#13944 = FACE_OUTER_BOUND ( 'NONE', #13713, .T. ) ;
#13945 = ORIENTED_EDGE ( 'NONE', *, *, #49315, .T. ) ;
#13946 = DIRECTION ( 'NONE',  ( -0.005961354470445682716, -0.6427876096865404731, 0.7660212471507180654 ) ) ;
#13947 = PLANE ( 'NONE',  #46666 ) ;
#13948 = ORIENTED_EDGE ( 'NONE', *, *, #31451, .T. ) ;
#13949 = DIRECTION ( 'NONE',  ( -0.7660212471507179544, -0.6427876096865405842, -0.005961354470445141482 ) ) ;
#13950 = ORIENTED_EDGE ( 'NONE', *, *, #18053, .F. ) ;
#13951 = DIRECTION ( 'NONE',  ( -0.005961354470445682716, -0.6427876096865404731, 0.7660212471507180654 ) ) ;
#13952 = AXIS2_PLACEMENT_3D ( 'NONE', #45785, #45491, #28461 ) ;
#13953 = ORIENTED_EDGE ( 'NONE', *, *, #7804, .F. ) ;
#13954 = CARTESIAN_POINT ( 'NONE',  ( -9.808144436391993182, 0.000000000000000000, 10.77986332834118777 ) ) ;
#13955 = DIRECTION ( 'NONE',  ( 0.5364919789714477361, 0.6444004775717706579, 0.5449076811759711036 ) ) ;
#13956 = CARTESIAN_POINT ( 'NONE',  ( -12.44516864510371512, -4.889348428825665671, 1.559451445217089560 ) ) ;
#13957 = B_SPLINE_CURVE_WITH_KNOTS ( 'NONE', 3,
 ( #14483, #19277, #2235, #6250, #22997, #40316, #40868, #27247, #53642, #1689, #14749, #36083 ),
 .UNSPECIFIED., .F., .F.,
 ( 4, 2, 2, 2, 2, 4 ),
 ( 0.07980989636644560126, 0.1159099261691615840, 0.2318198523383231402, 0.4636397046766463914, 0.6954595570149695316, 0.9272794093314227215 ),
 .UNSPECIFIED. ) ;
#13958 = ORIENTED_EDGE ( 'NONE', *, *, #43837, .F. ) ;
#13959 = VECTOR ( 'NONE', #28486, 1000.000000000000227 ) ;
#13960 = CARTESIAN_POINT ( 'NONE',  ( -19.60990026154428278, 0.000000000000000000, 4.498472333781370125 ) ) ;
#13961 = DIRECTION ( 'NONE',  ( -0.6427681459581293666, -0.7660444431189770143, -0.005002170337467561935 ) ) ;
#13962 = CARTESIAN_POINT ( 'NONE',  ( -30.79489622823572859, -0.1191753592594197858, 8.743409918460921304 ) ) ;
#13963 = EDGE_CURVE ( 'NONE', #20216, #32474, #4990, .T. ) ;
#13964 = EDGE_CURVE ( 'NONE', #83, #17803, #35644, .T. ) ;
#13965 = VECTOR ( 'NONE', #48774, 999.9999999999998863 ) ;
#13966 = CARTESIAN_POINT ( 'NONE',  ( -8.024318355659660895, 0.000000000000000000, 6.335291332000425157 ) ) ;
#13967 = CARTESIAN_POINT ( 'NONE',  ( -11.22056963685719211, 0.000000000000000000, 1.239771416285661010 ) ) ;
#13968 = CARTESIAN_POINT ( 'NONE',  ( -22.02718324817240969, 19.65220053346460460, 4.407440554554201917 ) ) ;
#13969 = CARTESIAN_POINT ( 'NONE',  ( -16.99924723426068951, 0.000000000000000000, 13.49389102713827171 ) ) ;
#13970 = ORIENTED_EDGE ( 'NONE', *, *, #33491, .T. ) ;
#13971 = LINE ( 'NONE', #23352, #45273 ) ;
#13972 = CARTESIAN_POINT ( 'NONE',  ( -13.24358169501890714, -0.8417996532631553119, 3.207725259429178077 ) ) ;
#13973 = LINE ( 'NONE', #31304, #43213 ) ;
#13974 = ORIENTED_EDGE ( 'NONE', *, *, #44450, .F. ) ;
#13975 = VECTOR ( 'NONE', #44041, 999.9999999999998863 ) ;
#13976 = FACE_OUTER_BOUND ( 'NONE', #36976, .T. ) ;
#13977 = CARTESIAN_POINT ( 'NONE',  ( 4.912750499197525045, -1.131233082521085231, 2.061810099490657411 ) ) ;
#13978 = ORIENTED_EDGE ( 'NONE', *, *, #47979, .T. ) ;
#13979 = EDGE_CURVE ( 'NONE', #27886, #25181, #4157, .T. ) ;
#13980 = EDGE_CURVE ( 'NONE', #24541, #2142, #55450, .T. ) ;
#13981 = EDGE_CURVE ( 'NONE', #50871, #21762, #30268, .T. ) ;
#13982 = VECTOR ( 'NONE', #1728, 1000.000000000000114 ) ;
#13983 = LINE ( 'NONE', #26767, #45232 ) ;
#13984 = DIRECTION ( 'NONE',  ( 0.000000000000000000, -1.000000000000000000, 0.000000000000000000 ) ) ;
#13985 = LINE ( 'NONE', #9751, #37794 ) ;
#13986 = EDGE_CURVE ( 'NONE', #32747, #48737, #2398, .T. ) ;
#13987 = DIRECTION ( 'NONE',  ( 0.000000000000000000, -0.000000000000000000, -1.000000000000000000 ) ) ;
#13988 = VERTEX_POINT ( 'NONE', #27975 ) ;
#13989 = VECTOR ( 'NONE', #9890, 999.9999999999998863 ) ;
#13990 = VECTOR ( 'NONE', #52412, 1000.000000000000000 ) ;
#13991 = EDGE_LOOP ( 'NONE', ( #51649, #42016, #13412, #43000 ) ) ;
#13992 = CARTESIAN_POINT ( 'NONE',  ( -12.73074006674189995, 1.095915999411505082, 3.624957756920523355 ) ) ;
#13993 = CARTESIAN_POINT ( 'NONE',  ( -20.77710809187043850, -5.375054281893166142, 4.780363120533749566 ) ) ;
#13994 = CARTESIAN_POINT ( 'NONE',  ( -65.38649145641349492, 1.999999999999980016, 1.314563741827306620 ) ) ;
#13995 = DIRECTION ( 'NONE',  ( 0.007781995580012663651, 0.000000000000000000, -0.9999697198139515519 ) ) ;
#13996 = DIRECTION ( 'NONE',  ( -0.9999697198139514409, -0.000000000000000000, -0.007781995580013368816 ) ) ;
#13997 = ADVANCED_FACE ( 'NONE', ( #15441 ), #2095, .F. ) ;
#13998 = CARTESIAN_POINT ( 'NONE',  ( -13.51773605596954120, 4.819660872929013351, 1.778907064336885391 ) ) ;
#13999 = VERTEX_POINT ( 'NONE', #14617 ) ;
#14000 = FACE_OUTER_BOUND ( 'NONE', #31900, .T. ) ;
#14001 = EDGE_CURVE ( 'NONE', #33244, #38668, #31936, .T. ) ;
#14002 = AXIS2_PLACEMENT_3D ( 'NONE', #53830, #14942, #5317 ) ;
#14003 = CARTESIAN_POINT ( 'NONE',  ( -13.08330893211609869, 0.000000000000000000, 1.763933231766363630 ) ) ;
#14004 = ORIENTED_EDGE ( 'NONE', *, *, #29654, .F. ) ;
#14005 = VECTOR ( 'NONE', #880, 999.9999999999998863 ) ;
#14006 = EDGE_CURVE ( 'NONE', #9106, #33688, #19429, .T. ) ;
#14007 = DIRECTION ( 'NONE',  ( 0.9999697198139515519, 0.000000000000000000, 0.007781995580013368816 ) ) ;
#14008 = CARTESIAN_POINT ( 'NONE',  ( -12.33850799832341849, 0.000000000000000000, 11.68350162852954632 ) ) ;
#14009 = VECTOR ( 'NONE', #7761, 999.9999999999998863 ) ;
#14010 = CARTESIAN_POINT ( 'NONE',  ( -19.52298068925090746, 0.000000000000000000, 5.237812901604549154 ) ) ;
#14011 = ORIENTED_EDGE ( 'NONE', *, *, #38548, .T. ) ;
#14012 = EDGE_CURVE ( 'NONE', #51326, #45566, #6386, .T. ) ;
#14013 = FACE_OUTER_BOUND ( 'NONE', #9407, .T. ) ;
#14014 = ORIENTED_EDGE ( 'NONE', *, *, #6847, .T. ) ;
#14015 = ORIENTED_EDGE ( 'NONE', *, *, #447, .T. ) ;
#14016 = ORIENTED_EDGE ( 'NONE', *, *, #30026, .F. ) ;
#14017 = AXIS2_PLACEMENT_3D ( 'NONE', #20024, #19772, #53839 ) ;
#14018 = ORIENTED_EDGE ( 'NONE', *, *, #15907, .T. ) ;
#14019 = VECTOR ( 'NONE', #21270, 1000.000000000000000 ) ;
#14020 = DIRECTION ( 'NONE',  ( -0.7660212471507179544, -0.6427876096865405842, -0.005961354470445141482 ) ) ;
#14021 = EDGE_LOOP ( 'NONE', ( #26351, #14480, #45188 ) ) ;
#14022 = DIRECTION ( 'NONE',  ( 0.007781995580012663651, -3.146120232559066537E-19, -0.9999697198139514409 ) ) ;
#14023 = CARTESIAN_POINT ( 'NONE',  ( -58.00000000000000711, -9.000000000000000000, 7.102951435054649637E-15 ) ) ;
#14024 = VECTOR ( 'NONE', #37995, 999.9999999999998863 ) ;
#14025 = EDGE_LOOP ( 'NONE', ( #13104, #53545, #8198, #15663 ) ) ;
#14026 = FACE_OUTER_BOUND ( 'NONE', #8000, .T. ) ;
#14027 = ORIENTED_EDGE ( 'NONE', *, *, #15032, .T. ) ;
#14028 = LINE ( 'NONE', #48948, #54917 ) ;
#14029 = ORIENTED_EDGE ( 'NONE', *, *, #32844, .F. ) ;
#14030 = VECTOR ( 'NONE', #10853, 999.9999999999998863 ) ;
#14031 = CARTESIAN_POINT ( 'NONE',  ( -18.67619601524082285, 0.000000000000000000, 3.936400510096834893 ) ) ;
#14032 = VECTOR ( 'NONE', #8067, 999.9999999999998863 ) ;
#14033 = DIRECTION ( 'NONE',  ( 0.6427681459581294776, -0.7660444431189769032, 0.005002170337467562802 ) ) ;
#14034 = CARTESIAN_POINT ( 'NONE',  ( -21.47341775636118655, -0.1191753592594197858, 5.122631121243466090 ) ) ;
#14035 = DIRECTION ( 'NONE',  ( 0.007781995580012663651, 0.000000000000000000, -0.9999697198139515519 ) ) ;
#14036 = PLANE ( 'NONE',  #51365 ) ;
#14037 = DIRECTION ( 'NONE',  ( 0.5364919789714477361, 0.6444004775717706579, 0.5449076811759711036 ) ) ;
#14038 = EDGE_LOOP ( 'NONE', ( #15985, #10119, #38131, #49581 ) ) ;
#14039 = ADVANCED_FACE ( 'NONE', ( #19144 ), #32235, .F. ) ;
#14040 = ORIENTED_EDGE ( 'NONE', *, *, #714, .F. ) ;
#14041 = DIRECTION ( 'NONE',  ( 0.000000000000000000, -1.000000000000000000, 0.000000000000000000 ) ) ;
#14042 = PLANE ( 'NONE',  #49351 ) ;
#14043 = ADVANCED_FACE ( 'NONE', ( #23687 ), #31675, .F. ) ;
#14044 = DIRECTION ( 'NONE',  ( 0.9999697198139515519, 0.000000000000000000, 0.007781995580013368816 ) ) ;
#14045 = VECTOR ( 'NONE', #40867, 1000.000000000000227 ) ;
#14046 = LINE ( 'NONE', #1249, #43042 ) ;
#14047 = ORIENTED_EDGE ( 'NONE', *, *, #7076, .F. ) ;
#14048 = AXIS2_PLACEMENT_3D ( 'NONE', #10816, #53677, #32941 ) ;
#14049 = PLANE ( 'NONE',  #9544 ) ;
#14050 = LINE ( 'NONE', #4680, #4172 ) ;
#14051 = VERTEX_POINT ( 'NONE', #9821 ) ;
#14052 = CARTESIAN_POINT ( 'NONE',  ( -10.94028622754223967, 0.000000000000000000, 11.14038480894692995 ) ) ;
#14053 = DIRECTION ( 'NONE',  ( -0.9999697198139514409, -0.000000000000000000, -0.007781995580013368816 ) ) ;
#14054 = VECTOR ( 'NONE', #7851, 999.9999999999998863 ) ;
#14055 = VERTEX_POINT ( 'NONE', #19723 ) ;
#14056 = ADVANCED_FACE ( 'NONE', ( #54349 ), #27126, .F. ) ;
#14057 = ADVANCED_FACE ( 'NONE', ( #18606 ), #45021, .F. ) ;
#14058 = ADVANCED_FACE ( 'NONE', ( #1818 ), #23154, .F. ) ;
#14059 = CARTESIAN_POINT ( 'NONE',  ( -13.96745630169485786, 0.000000000000000000, 7.866371765625014945 ) ) ;
#14060 = CARTESIAN_POINT ( 'NONE',  ( -14.04943075308655587, -0.1191753592594183703, 5.549738374539030517 ) ) ;
#14061 = AXIS2_PLACEMENT_3D ( 'NONE', #3120, #55105, #50817 ) ;
#14062 = CARTESIAN_POINT ( 'NONE',  ( -1.086233639165236964, 0.000000000000000000, -2.796443541562362078 ) ) ;
#14063 = EDGE_CURVE ( 'NONE', #13134, #33308, #15198, .T. ) ;
#14064 = PLANE ( 'NONE',  #6071 ) ;
#14065 = CARTESIAN_POINT ( 'NONE',  ( -16.85737050867004783, -0.1191753592594190225, 8.113210826735326009 ) ) ;
#14066 = VERTEX_POINT ( 'NONE', #40752 ) ;
#14067 = VECTOR ( 'NONE', #54309, 1000.000000000000227 ) ;
#14068 = CIRCLE ( 'NONE', #4091, 3.000000000000001332 ) ;
#14069 = VERTEX_POINT ( 'NONE', #36468 ) ;
#14070 = VECTOR ( 'NONE', #46581, 999.9999999999998863 ) ;
#14071 = VECTOR ( 'NONE', #28763, 1000.000000000000000 ) ;
#14072 = PLANE ( 'NONE',  #47511 ) ;
#14073 = DIRECTION ( 'NONE',  ( -0.005961354470445682716, -0.6427876096865404731, 0.7660212471507180654 ) ) ;
#14074 = CARTESIAN_POINT ( 'NONE',  ( -16.33317936670417225, 0.000000000000000000, 13.31440848639340224 ) ) ;
#14075 = VECTOR ( 'NONE', #12851, 1000.000000000000227 ) ;
#14076 = LINE ( 'NONE', #52962, #28244 ) ;
#14077 = DIRECTION ( 'NONE',  ( -0.9999697198139514409, -0.000000000000000000, -0.007781995580013368816 ) ) ;
#14078 = VERTEX_POINT ( 'NONE', #45537 ) ;
#14079 = DIRECTION ( 'NONE',  ( 0.007781995580012663651, 0.000000000000000000, -0.9999697198139515519 ) ) ;
#14080 = DIRECTION ( 'NONE',  ( 0.9999697198139515519, 0.000000000000000000, 0.007781995580013368816 ) ) ;
#14081 = ADVANCED_FACE ( 'NONE', ( #23970 ), #5538, .F. ) ;
#14082 = AXIS2_PLACEMENT_3D ( 'NONE', #25578, #12807, #55989 ) ;
#14083 = ADVANCED_FACE ( 'NONE', ( #1266 ), #48979, .F. ) ;
#14084 = DIRECTION ( 'NONE',  ( -0.7660212471507179544, -0.6427876096865405842, -0.005961354470445141482 ) ) ;
#14085 = VECTOR ( 'NONE', #50123, 1000.000000000000227 ) ;
#14086 = LINE ( 'NONE', #1276, #3355 ) ;
#14087 = EDGE_CURVE ( 'NONE', #18849, #12775, #2658, .T. ) ;
#14088 = ORIENTED_EDGE ( 'NONE', *, *, #23588, .T. ) ;
#14089 = DIRECTION ( 'NONE',  ( 0.5364919789714477361, 0.6444004775717706579, 0.5449076811759711036 ) ) ;
#14090 = ORIENTED_EDGE ( 'NONE', *, *, #38202, .F. ) ;
#14091 = LINE ( 'NONE', #26867, #13231 ) ;
#14092 = CARTESIAN_POINT ( 'NONE',  ( -25.20123094555300369, 0.000000000000000000, 6.470945668149052032 ) ) ;
#14093 = VERTEX_POINT ( 'NONE', #16283 ) ;
#14094 = EDGE_CURVE ( 'NONE', #22899, #50665, #25377, .T. ) ;
#14095 = LINE ( 'NONE', #31422, #10877 ) ;
#14096 = ORIENTED_EDGE ( 'NONE', *, *, #10290, .T. ) ;
#14097 = EDGE_CURVE ( 'NONE', #22349, #25311, #40600, .T. ) ;
#14098 = AXIS2_PLACEMENT_3D ( 'NONE', #54608, #42129, #7792 ) ;
#14099 = ORIENTED_EDGE ( 'NONE', *, *, #24436, .T. ) ;
#14100 = ORIENTED_EDGE ( 'NONE', *, *, #17134, .T. ) ;
#14101 = PLANE ( 'NONE',  #45671 ) ;
#14102 = ORIENTED_EDGE ( 'NONE', *, *, #9002, .T. ) ;
#14103 = AXIS2_PLACEMENT_3D ( 'NONE', #34288, #51322, #55282 ) ;
#14104 = ORIENTED_EDGE ( 'NONE', *, *, #16120, .T. ) ;
#14105 = CARTESIAN_POINT ( 'NONE',  ( -19.36810218178845489, 21.37987375194732209, -4.244941833920536922 ) ) ;
#14106 = DIRECTION ( 'NONE',  ( -0.5364919789714478471, 0.6444004775717705469, -0.5449076811759709926 ) ) ;
#14107 = VECTOR ( 'NONE', #21396, 999.9999999999998863 ) ;
#14108 = EDGE_LOOP ( 'NONE', ( #1296, #6222, #18080, #32457 ) ) ;
#14109 = ORIENTED_EDGE ( 'NONE', *, *, #276, .F. ) ;
#14110 = DIRECTION ( 'NONE',  ( 0.9999697198139515519, 0.000000000000000000, 0.007781995580013368816 ) ) ;
#14111 = ORIENTED_EDGE ( 'NONE', *, *, #53812, .F. ) ;
#14112 = AXIS2_PLACEMENT_3D ( 'NONE', #18360, #39104, #9590 ) ;
#14113 = VERTEX_POINT ( 'NONE', #21100 ) ;
#14114 = VECTOR ( 'NONE', #11657, 999.9999999999998863 ) ;
#14115 = VECTOR ( 'NONE', #54871, 1000.000000000000000 ) ;
#14116 = DIRECTION ( 'NONE',  ( 0.6427681459581294776, -0.7660444431189769032, 0.005002170337467562802 ) ) ;
#14117 = CARTESIAN_POINT ( 'NONE',  ( -11.14227222507966530, 0.000000000000000000, 3.087041093882136433 ) ) ;
#14118 = DIRECTION ( 'NONE',  ( 0.005002170337468016433, -0.7660444431189770143, -0.6427681459581293666 ) ) ;
#14119 = LINE ( 'NONE', #49018, #51320 ) ;
#14120 = ORIENTED_EDGE ( 'NONE', *, *, #46873, .F. ) ;
#14121 = DIRECTION ( 'NONE',  ( -0.9999697198139514409, -0.000000000000000000, -0.007781995580013368816 ) ) ;
#14122 = ORIENTED_EDGE ( 'NONE', *, *, #27472, .F. ) ;
#14123 = AXIS2_PLACEMENT_3D ( 'NONE', #2227, #45387, #45669 ) ;
#14124 = AXIS2_PLACEMENT_3D ( 'NONE', #49203, #45237, #19380 ) ;
#14125 = DIRECTION ( 'NONE',  ( -0.9999697198139514409, -0.000000000000000000, -0.007781995580013368816 ) ) ;
#14126 = VECTOR ( 'NONE', #46760, 1000.000000000000227 ) ;
#14127 = DIRECTION ( 'NONE',  ( -0.7660212471507179544, -0.6427876096865405842, -0.005961354470445141482 ) ) ;
#14128 = VECTOR ( 'NONE', #51199, 1000.000000000000000 ) ;
#14129 = DIRECTION ( 'NONE',  ( 0.000000000000000000, -0.000000000000000000, -1.000000000000000000 ) ) ;
#14130 = DIRECTION ( 'NONE',  ( 0.6427681459581294776, -0.7660444431189769032, 0.005002170337467562802 ) ) ;
#14131 = DIRECTION ( 'NONE',  ( 0.007781995580012662783, 0.000000000000000000, -0.9999697198139514409 ) ) ;
#14132 = CARTESIAN_POINT ( 'NONE',  ( -28.92982233430281980, 0.000000000000000000, 7.919257187036034651 ) ) ;
#14133 = FACE_OUTER_BOUND ( 'NONE', #51143, .T. ) ;
#14134 = EDGE_LOOP ( 'NONE', ( #46691, #18431, #14720, #15523 ) ) ;
#14135 = DIRECTION ( 'NONE',  ( 0.005002170337468016433, -0.7660444431189770143, -0.6427681459581293666 ) ) ;
#14136 = EDGE_CURVE ( 'NONE', #53080, #56036, #46371, .T. ) ;
#14137 = DIRECTION ( 'NONE',  ( -0.005961354470445682716, -0.6427876096865404731, 0.7660212471507180654 ) ) ;
#14138 = CARTESIAN_POINT ( 'NONE',  ( -15.60102546347950536, 0.000000000000000000, 12.95077420755565356 ) ) ;
#14139 = DIRECTION ( 'NONE',  ( -0.7660212471507179544, -0.6427876096865405842, -0.005961354470445141482 ) ) ;
#14140 = CARTESIAN_POINT ( 'NONE',  ( -20.22851404498383587, 19.24728700913452073, -4.351128180092163511 ) ) ;
#14141 = DIRECTION ( 'NONE',  ( 0.007781995580012662783, 0.000000000000000000, -0.9999697198139514409 ) ) ;
#14142 = EDGE_CURVE ( 'NONE', #12775, #17469, #29356, .T. ) ;
#14143 = ADVANCED_FACE ( 'NONE', ( #33604 ), #41833, .F. ) ;
#14144 = CARTESIAN_POINT ( 'NONE',  ( -11.44573815241757764, 9.034849713672558735, 1.227539821638981010 ) ) ;
#14145 = AXIS2_PLACEMENT_3D ( 'NONE', #19077, #44633, #14550 ) ;
#14146 = DIRECTION ( 'NONE',  ( -0.7660212471507179544, -0.6427876096865405842, -0.005961354470445141482 ) ) ;
#14147 = B_SPLINE_CURVE_WITH_KNOTS ( 'NONE', 3,
 ( #8982, #13242, #18311, #22023 ),
 .UNSPECIFIED., .F., .F.,
 ( 4, 4 ),
 ( 0.000000000000000000, 1.000000000000000000 ),
 .UNSPECIFIED. ) ;
#14148 = AXIS2_PLACEMENT_3D ( 'NONE', #15226, #32541, #16057 ) ;
#14149 = ORIENTED_EDGE ( 'NONE', *, *, #12090, .F. ) ;
#14150 = CARTESIAN_POINT ( 'NONE',  ( -18.60364671047386409, 0.000000000000000000, 6.522289594208837471 ) ) ;
#14151 = DIRECTION ( 'NONE',  ( 0.000000000000000000, -0.000000000000000000, -1.000000000000000000 ) ) ;
#14152 = CARTESIAN_POINT ( 'NONE',  ( 2.072287782118878319, 0.000000000000000000, -2.950529333540147015 ) ) ;
#14153 = AXIS2_PLACEMENT_3D ( 'NONE', #6644, #41565, #37288 ) ;
#14154 = PLANE ( 'NONE',  #19198 ) ;
#14155 = VECTOR ( 'NONE', #44550, 1000.000000000000227 ) ;
#14156 = PLANE ( 'NONE',  #8560 ) ;
#14157 = LINE ( 'NONE', #31744, #17769 ) ;
#14158 = DIRECTION ( 'NONE',  ( 0.000000000000000000, -0.000000000000000000, -1.000000000000000000 ) ) ;
#14159 = VECTOR ( 'NONE', #49919, 1000.000000000000227 ) ;
#14160 = AXIS2_PLACEMENT_3D ( 'NONE', #54051, #14870, #45504 ) ;
#14161 = CARTESIAN_POINT ( 'NONE',  ( -19.92672316015189082, 0.000000000000000000, 6.342667093759775554 ) ) ;
#14162 = AXIS2_PLACEMENT_3D ( 'NONE', #39327, #114, #21995 ) ;
#14163 = CARTESIAN_POINT ( 'NONE',  ( -18.33900375759556667, 0.000000000000000000, 6.524349106860843683 ) ) ;
#14164 = VECTOR ( 'NONE', #43717, 1000.000000000000114 ) ;
#14165 = EDGE_LOOP ( 'NONE', ( #24000, #19887, #49958, #27032 ) ) ;
#14166 = VECTOR ( 'NONE', #15760, 999.9999999999998863 ) ;
#14167 = ADVANCED_FACE ( 'NONE', ( #51214 ), #7483, .F. ) ;
#14168 = VECTOR ( 'NONE', #53957, 999.9999999999998863 ) ;
#14169 = ORIENTED_EDGE ( 'NONE', *, *, #22476, .F. ) ;
#14170 = VECTOR ( 'NONE', #53853, 1000.000000000000227 ) ;
#14171 = ORIENTED_EDGE ( 'NONE', *, *, #12478, .F. ) ;
#14172 = EDGE_LOOP ( 'NONE', ( #2876, #253, #13252 ) ) ;
#14173 = ADVANCED_FACE ( 'NONE', ( #37299 ), #32764, .F. ) ;
#14174 = EDGE_LOOP ( 'NONE', ( #54025, #21840, #21280, #39919 ) ) ;
#14175 = DIRECTION ( 'NONE',  ( 0.9999697198139515519, 0.000000000000000000, 0.007781995580013368816 ) ) ;
#14176 = DIRECTION ( 'NONE',  ( 0.005002170337468016433, -0.7660444431189770143, -0.6427681459581293666 ) ) ;
#14177 = ORIENTED_EDGE ( 'NONE', *, *, #27192, .F. ) ;
#14178 = EDGE_LOOP ( 'NONE', ( #9846, #16605, #49300, #12893 ) ) ;
#14179 = ADVANCED_FACE ( 'NONE', ( #33898 ), #29066, .F. ) ;
#14180 = EDGE_LOOP ( 'NONE', ( #54365, #43742, #14499, #25746 ) ) ;
#14181 = VECTOR ( 'NONE', #35124, 999.9999999999998863 ) ;
#14182 = FACE_OUTER_BOUND ( 'NONE', #30050, .T. ) ;
#14183 = ORIENTED_EDGE ( 'NONE', *, *, #38408, .T. ) ;
#14184 = DIRECTION ( 'NONE',  ( 0.007781995580012663651, 0.000000000000000000, -0.9999697198139515519 ) ) ;
#14185 = DIRECTION ( 'NONE',  ( 0.5449076811759707706, 0.6444004775717708799, -0.5364919789714476250 ) ) ;
#14186 = ORIENTED_EDGE ( 'NONE', *, *, #38633, .F. ) ;
#14187 = VECTOR ( 'NONE', #38415, 999.9999999999998863 ) ;
#14188 = DIRECTION ( 'NONE',  ( 0.9999697198139515519, 0.000000000000000000, 0.007781995580013368816 ) ) ;
#14189 = EDGE_LOOP ( 'NONE', ( #21435, #10901, #325, #14662 ) ) ;
#14190 = PLANE ( 'NONE',  #24586 ) ;
#14191 = AXIS2_PLACEMENT_3D ( 'NONE', #14302, #19078, #53452 ) ;
#14192 = CARTESIAN_POINT ( 'NONE',  ( -13.00656791945457513, 0.000000000000000000, 3.811196853325626854 ) ) ;
#14193 = DIRECTION ( 'NONE',  ( 0.007781995580012662783, 0.000000000000000000, -0.9999697198139514409 ) ) ;
#14194 = CARTESIAN_POINT ( 'NONE',  ( -13.82194518983451736, -3.756034771668161909, 2.130396849930530134 ) ) ;
#14195 = VECTOR ( 'NONE', #36016, 999.9999999999998863 ) ;
#14196 = ORIENTED_EDGE ( 'NONE', *, *, #18140, .F. ) ;
#14197 = LINE ( 'NONE', #18425, #42136 ) ;
#14198 = DIRECTION ( 'NONE',  ( 0.5449076811759707706, 0.6444004775717708799, -0.5364919789714476250 ) ) ;
#14199 = DIRECTION ( 'NONE',  ( 0.9659258262890692004, -0.2588190451025176864, 0.000000000000000000 ) ) ;
#14200 = ORIENTED_EDGE ( 'NONE', *, *, #7060, .T. ) ;
#14201 = DIRECTION ( 'NONE',  ( 0.007781995580012663651, -3.146120232559066537E-19, -0.9999697198139514409 ) ) ;
#14202 = ADVANCED_FACE ( 'NONE', ( #20825 ), #55756, .F. ) ;
#14203 = B_SPLINE_CURVE_WITH_KNOTS ( 'NONE', 3,
 ( #27946, #44982, #49520, #27097 ),
 .UNSPECIFIED., .F., .F.,
 ( 4, 4 ),
 ( 0.7664662348551912752, 1.000000000000000000 ),
 .UNSPECIFIED. ) ;
#14204 = ORIENTED_EDGE ( 'NONE', *, *, #24731, .F. ) ;
#14205 = VECTOR ( 'NONE', #1411, 1000.000000000000227 ) ;
#14206 = EDGE_CURVE ( 'NONE', #19740, #23008, #25118, .T. ) ;
#14207 = VECTOR ( 'NONE', #3488, 1000.000000000000000 ) ;
#14208 = CARTESIAN_POINT ( 'NONE',  ( -13.57131363945838487, -0.6798977022406551551, 3.069318792522690575 ) ) ;
#14209 = CARTESIAN_POINT ( 'NONE',  ( -19.66637125327706670, -0.08393247865673328367, 7.012927507599523658 ) ) ;
#14210 = DIRECTION ( 'NONE',  ( -0.9999697198139514409, -0.000000000000000000, -0.007781995580013368816 ) ) ;
#14211 = LINE ( 'NONE', #10198, #15078 ) ;
#14212 = LINE ( 'NONE', #4822, #48591 ) ;
#14213 = FACE_OUTER_BOUND ( 'NONE', #2959, .T. ) ;
#14214 = ADVANCED_FACE ( 'NONE', ( #3235 ), #28510, .F. ) ;
#14215 = EDGE_CURVE ( 'NONE', #1477, #29979, #42426, .T. ) ;
#14216 = DIRECTION ( 'NONE',  ( 0.6427681459581294776, -0.7660444431189769032, 0.005002170337467562802 ) ) ;
#14217 = VECTOR ( 'NONE', #11277, 999.9999999999998863 ) ;
#14218 = AXIS2_PLACEMENT_3D ( 'NONE', #5532, #49550, #31670 ) ;
#14219 = LINE ( 'NONE', #14743, #23770 ) ;
#14220 = SURFACE_SIDE_STYLE ('',( #31532 ) ) ;
#14221 = DIRECTION ( 'NONE',  ( 0.6427681459581294776, -0.7660444431189769032, 0.005002170337467562802 ) ) ;
#14222 = ORIENTED_EDGE ( 'NONE', *, *, #35132, .T. ) ;
#14223 = DIRECTION ( 'NONE',  ( 0.005002170337468016433, -0.7660444431189770143, -0.6427681459581293666 ) ) ;
#14224 = DIRECTION ( 'NONE',  ( 0.007781995580012663651, 0.000000000000000000, -0.9999697198139515519 ) ) ;
#14225 = CARTESIAN_POINT ( 'NONE',  ( -15.88053067323646417, -0.1191753592594197858, 2.950163842912994383 ) ) ;
#14226 = CARTESIAN_POINT ( 'NONE',  ( -14.06311187215340297, 3.200641362704009119, 7.596709105035338361 ) ) ;
#14227 = DIRECTION ( 'NONE',  ( 0.5364919789714477361, 0.6444004775717706579, 0.5449076811759711036 ) ) ;
#14228 = DIRECTION ( 'NONE',  ( 0.000000000000000000, -1.000000000000000000, 0.000000000000000000 ) ) ;
#14229 = LINE ( 'NONE', #35792, #244 ) ;
#14230 = VECTOR ( 'NONE', #21599, 1000.000000000000114 ) ;
#14231 = EDGE_CURVE ( 'NONE', #6270, #3791, #46966, .T. ) ;
#14232 = EDGE_LOOP ( 'NONE', ( #2558, #2732, #5566, #38370 ) ) ;
#14233 = EDGE_LOOP ( 'NONE', ( #33286, #9349, #33928, #35869, #3401, #47912, #51791 ) ) ;
#14234 = LINE ( 'NONE', #44569, #2357 ) ;
#14235 = CARTESIAN_POINT ( 'NONE',  ( -13.09429047785683942, -0.1191753592594188005, 2.233182868755169803 ) ) ;
#14236 = ORIENTED_EDGE ( 'NONE', *, *, #47960, .F. ) ;
#14237 = FACE_OUTER_BOUND ( 'NONE', #15463, .T. ) ;
#14238 = VECTOR ( 'NONE', #41639, 999.9999999999998863 ) ;
#14239 = EDGE_LOOP ( 'NONE', ( #26228, #30726, #35219, #49169 ) ) ;
#14240 = CARTESIAN_POINT ( 'NONE',  ( -24.26908309836554878, 0.000000000000000000, 6.108867788427308376 ) ) ;
#14241 = VECTOR ( 'NONE', #40999, 1000.000000000000227 ) ;
#14242 = ORIENTED_EDGE ( 'NONE', *, *, #10782, .T. ) ;
#14243 = ORIENTED_EDGE ( 'NONE', *, *, #39865, .T. ) ;
#14244 = EDGE_LOOP ( 'NONE', ( #45509, #22153, #48231, #53266 ) ) ;
#14245 = CARTESIAN_POINT ( 'NONE',  ( -12.43497384774700265, -2.622721114510659035, 5.816430034565780005 ) ) ;
#14246 = FACE_OUTER_BOUND ( 'NONE', #9674, .T. ) ;
#14247 = DIRECTION ( 'NONE',  ( 0.5364919789714477361, 0.6444004775717706579, 0.5449076811759711036 ) ) ;
#14248 = VECTOR ( 'NONE', #35158, 999.9999999999998863 ) ;
#14249 = FACE_OUTER_BOUND ( 'NONE', #10748, .T. ) ;
#14250 = ORIENTED_EDGE ( 'NONE', *, *, #42068, .T. ) ;
#14251 = EDGE_CURVE ( 'NONE', #21588, #22086, #41575, .T. ) ;
#14252 = ORIENTED_EDGE ( 'NONE', *, *, #28368, .F. ) ;
#14253 = VECTOR ( 'NONE', #54004, 1000.000000000000227 ) ;
#14254 = LINE ( 'NONE', #1145, #22778 ) ;
#14255 = EDGE_LOOP ( 'NONE', ( #22914, #3812, #44266, #21872 ) ) ;
#14256 = LINE ( 'NONE', #18792, #25717 ) ;
#14257 = ORIENTED_EDGE ( 'NONE', *, *, #45073, .T. ) ;
#14258 = FACE_OUTER_BOUND ( 'NONE', #52147, .T. ) ;
#14259 = DIRECTION ( 'NONE',  ( -0.6246952433987893460, -0.7422098413412802076, 0.2426528472758542054 ) ) ;
#14260 = EDGE_CURVE ( 'NONE', #38668, #23390, #16560, .T. ) ;
#14261 = ORIENTED_EDGE ( 'NONE', *, *, #2189, .F. ) ;
#14262 = FACE_OUTER_BOUND ( 'NONE', #43436, .T. ) ;
#14263 = VERTEX_POINT ( 'NONE', #4375 ) ;
#14264 = EDGE_CURVE ( 'NONE', #56189, #21908, #51763, .T. ) ;
#14265 = ADVANCED_FACE ( 'NONE', ( #13703 ), #21686, .F. ) ;
#14266 = DIRECTION ( 'NONE',  ( 0.007781995580012663651, 0.000000000000000000, -0.9999697198139515519 ) ) ;
#14267 = EDGE_LOOP ( 'NONE', ( #21704, #48508, #33653, #52133 ) ) ;
#14268 = DIRECTION ( 'NONE',  ( -0.6427681459581293666, -0.7660444431189770143, -0.005002170337467561935 ) ) ;
#14269 = CARTESIAN_POINT ( 'NONE',  ( -19.95699008208018199, 0.2864062442990042978, 4.424766562912388679 ) ) ;
#14270 = CARTESIAN_POINT ( 'NONE',  ( -11.40636015113596180, 0.000000000000000000, 11.32142374880780089 ) ) ;
#14271 = EDGE_CURVE ( 'NONE', #10033, #34166, #34200, .T. ) ;
#14272 = ORIENTED_EDGE ( 'NONE', *, *, #19595, .T. ) ;
#14273 = ADVANCED_FACE ( 'NONE', ( #17699 ), #25645, .F. ) ;
#14274 = FACE_OUTER_BOUND ( 'NONE', #41014, .T. ) ;
#14275 = AXIS2_PLACEMENT_3D ( 'NONE', #4089, #47524, #17409 ) ;
#14276 = FACE_OUTER_BOUND ( 'NONE', #12038, .T. ) ;
#14277 = CARTESIAN_POINT ( 'NONE',  ( -56.75000000000000711, 4.550000000000001599, -2.449489742783172108 ) ) ;
#14278 = FACE_OUTER_BOUND ( 'NONE', #3260, .T. ) ;
#14279 = EDGE_CURVE ( 'NONE', #15160, #21771, #35041, .T. ) ;
#14280 = FACE_OUTER_BOUND ( 'NONE', #10051, .T. ) ;
#14281 = VECTOR ( 'NONE', #54600, 999.9999999999998863 ) ;
#14282 = CARTESIAN_POINT ( 'NONE',  ( -67.07589540981676635, -9.520291518544306442, -2.709928232729476694 ) ) ;
#14283 = VERTEX_POINT ( 'NONE', #26776 ) ;
#14284 = DIRECTION ( 'NONE',  ( -0.2588190451025176864, -0.9659258262890692004, 0.000000000000000000 ) ) ;
#14285 = LINE ( 'NONE', #31303, #31345 ) ;
#14286 = DIRECTION ( 'NONE',  ( 0.9999697198139515519, 0.000000000000000000, 0.007781995580013368816 ) ) ;
#14287 = ORIENTED_EDGE ( 'NONE', *, *, #35606, .F. ) ;
#14288 = CARTESIAN_POINT ( 'NONE',  ( -13.73672976910459909, 0.000000000000000000, 12.22661844811216270 ) ) ;
#14289 = CARTESIAN_POINT ( 'NONE',  ( -26.13493519185646008, 0.000000000000000000, 7.033017491833586377 ) ) ;
#14290 = ORIENTED_EDGE ( 'NONE', *, *, #10852, .F. ) ;
#14291 = EDGE_CURVE ( 'NONE', #46324, #40047, #20253, .T. ) ;
#14292 = CARTESIAN_POINT ( 'NONE',  ( -16.33317936670417225, 0.000000000000000000, 13.31440848639340224 ) ) ;
#14293 = VECTOR ( 'NONE', #5516, 1000.000000000000114 ) ;
#14294 = CARTESIAN_POINT ( 'NONE',  ( -11.12790195755325229, 0.000000000000000000, 1.240492577593313550 ) ) ;
#14295 = LINE ( 'NONE', #22522, #50514 ) ;
#14296 = LINE ( 'NONE', #31013, #47361 ) ;
#14297 = EDGE_CURVE ( 'NONE', #41331, #5666, #52047, .T. ) ;
#14298 = ORIENTED_EDGE ( 'NONE', *, *, #51998, .T. ) ;
#14299 = EDGE_LOOP ( 'NONE', ( #23315, #35898, #40764, #36508 ) ) ;
#14300 = LINE ( 'NONE', #48337, #41224 ) ;
#14301 = FACE_OUTER_BOUND ( 'NONE', #1895, .T. ) ;
#14302 = CARTESIAN_POINT ( 'NONE',  ( -31.72626587586518099, 0.000000000000000000, 9.005490826201270949 ) ) ;
#14303 = DIRECTION ( 'NONE',  ( -0.6427681459581293666, -0.7660444431189770143, -0.005002170337467561935 ) ) ;
#14304 = DIRECTION ( 'NONE',  ( 0.9999697198139515519, 0.000000000000000000, 0.007781995580013368816 ) ) ;
#14305 = ORIENTED_EDGE ( 'NONE', *, *, #24384, .T. ) ;
#14306 = DIRECTION ( 'NONE',  ( 0.5449076811759707706, 0.6444004775717708799, -0.5364919789714476250 ) ) ;
#14307 = VERTEX_POINT ( 'NONE', #48338 ) ;
#14308 = CARTESIAN_POINT ( 'NONE',  ( -9.483718581678113324, 0.000000000000000000, 3.099948341838171029 ) ) ;
#14309 = CARTESIAN_POINT ( 'NONE',  ( -58.00000000000000711, -9.000000000000000000, -2.749999999999994671 ) ) ;
#14310 = VERTEX_POINT ( 'NONE', #22240 ) ;
#14311 = DIRECTION ( 'NONE',  ( 0.000000000000000000, -0.000000000000000000, -1.000000000000000000 ) ) ;
#14312 = CARTESIAN_POINT ( 'NONE',  ( -17.39286377064282618, -2.460819163488160655, 3.558787054721057608 ) ) ;
#14313 = FACE_OUTER_BOUND ( 'NONE', #42703, .T. ) ;
#14314 = ORIENTED_EDGE ( 'NONE', *, *, #32674, .F. ) ;
#14315 = DIRECTION ( 'NONE',  ( 0.7660212471507180654, -0.6427876096865404731, 0.005961354470445141482 ) ) ;
#14316 = EDGE_CURVE ( 'NONE', #52765, #19601, #12872, .T. ) ;
#14317 = ORIENTED_EDGE ( 'NONE', *, *, #21708, .F. ) ;
#14318 = ORIENTED_EDGE ( 'NONE', *, *, #40133, .T. ) ;
#14319 = AXIS2_PLACEMENT_3D ( 'NONE', #9534, #47877, #13770 ) ;
#14320 = ORIENTED_EDGE ( 'NONE', *, *, #46120, .T. ) ;
#14321 = ORIENTED_EDGE ( 'NONE', *, *, #30611, .F. ) ;
#14322 = PLANE ( 'NONE',  #12127 ) ;
#14323 = ORIENTED_EDGE ( 'NONE', *, *, #19241, .T. ) ;
#14324 = FACE_OUTER_BOUND ( 'NONE', #49652, .T. ) ;
#14325 = CARTESIAN_POINT ( 'NONE',  ( 2.072287782118878319, 0.000000000000000000, -2.950529333540147015 ) ) ;
#14326 = VECTOR ( 'NONE', #38718, 999.9999999999998863 ) ;
#14327 = ORIENTED_EDGE ( 'NONE', *, *, #40443, .F. ) ;
#14328 = ORIENTED_EDGE ( 'NONE', *, *, #39049, .T. ) ;
#14329 = DIRECTION ( 'NONE',  ( 0.005002170337468016433, -0.7660444431189770143, -0.6427681459581293666 ) ) ;
#14330 = ORIENTED_EDGE ( 'NONE', *, *, #29223, .T. ) ;
#14331 = ADVANCED_FACE ( 'NONE', ( #39271 ), #52352, .F. ) ;
#14332 = PLANE ( 'NONE',  #48228 ) ;
#14333 = DIRECTION ( 'NONE',  ( 0.000000000000000000, 0.000000000000000000, -1.000000000000000000 ) ) ;
#14334 = LINE ( 'NONE', #31647, #54961 ) ;
#14335 = DIRECTION ( 'NONE',  ( 0.9999697198139515519, 0.000000000000000000, 0.007781995580013368816 ) ) ;
#14336 = CARTESIAN_POINT ( 'NONE',  ( -27.99767448711536133, 0.000000000000000000, 7.557179307314289218 ) ) ;
#14337 = DIRECTION ( 'NONE',  ( 0.9999697198139515519, 0.000000000000000000, 0.007781995580013368816 ) ) ;
#14338 = EDGE_LOOP ( 'NONE', ( #33561, #26955, #50024, #48742 ) ) ;
#14339 = ORIENTED_EDGE ( 'NONE', *, *, #7271, .F. ) ;
#14340 = ADVANCED_FACE ( 'NONE', ( #52606 ), #42975, .F. ) ;
#14341 = DIRECTION ( 'NONE',  ( 0.7660212471507180654, -0.6427876096865404731, 0.005961354470445141482 ) ) ;
#14342 = CARTESIAN_POINT ( 'NONE',  ( -10.87188116519080694, 0.000000000000000000, 2.350481200018612160 ) ) ;
#14343 = ADVANCED_FACE ( 'NONE', ( #43527 ), #51511, .F. ) ;
#14344 = CARTESIAN_POINT ( 'NONE',  ( -16.93227919866189879, 0.000000000000000000, 4.888642269838840093 ) ) ;
#14345 = PLANE ( 'NONE',  #15874 ) ;
#14346 = EDGE_LOOP ( 'NONE', ( #51862, #26308, #33275, #27783 ) ) ;
#14347 = CARTESIAN_POINT ( 'NONE',  ( -22.36868959911851462, 19.74370688441071309, -4.657437592157546824 ) ) ;
#14348 = DIRECTION ( 'NONE',  ( -0.9999697198139514409, -0.000000000000000000, -0.007781995580013368816 ) ) ;
#14349 = ORIENTED_EDGE ( 'NONE', *, *, #11909, .T. ) ;
#14350 = DIRECTION ( 'NONE',  ( 0.7660212471507180654, -0.6427876096865404731, 0.005961354470445141482 ) ) ;
#14351 = CARTESIAN_POINT ( 'NONE',  ( -25.20278734466900517, 0.000000000000000000, 6.670939612111840944 ) ) ;
#14352 = VERTEX_POINT ( 'NONE', #21411 ) ;
#14353 = ADVANCED_FACE ( 'NONE', ( #47514 ), #4079, .F. ) ;
#14354 = CARTESIAN_POINT ( 'NONE',  ( -67.32216720457572023, -8.809864171621468287, 4.273291358077422331 ) ) ;
#14355 = DIRECTION ( 'NONE',  ( 0.5364919789714477361, 0.6444004775717706579, 0.5449076811759711036 ) ) ;
#14356 = CARTESIAN_POINT ( 'NONE',  ( -20.21494452004282394, 3.362543313726509719, 4.426819948926248749 ) ) ;
#14357 = PLANE ( 'NONE',  #30510 ) ;
#14358 = LINE ( 'NONE', #31086, #35573 ) ;
#14359 = EDGE_CURVE ( 'NONE', #31186, #51745, #47814, .T. ) ;
#14360 = ORIENTED_EDGE ( 'NONE', *, *, #22632, .T. ) ;
#14361 = VERTEX_POINT ( 'NONE', #39575 ) ;
#14362 = CARTESIAN_POINT ( 'NONE',  ( -11.25873531853475384, -0.1191753592594179401, 5.202124141889320263 ) ) ;
#14363 = CARTESIAN_POINT ( 'NONE',  ( -18.86354292863559579, 0.000000000000000000, 14.21804678658176080 ) ) ;
#14364 = LINE ( 'NONE', #18607, #36970 ) ;
#14365 = AXIS2_PLACEMENT_3D ( 'NONE', #31926, #36206, #5818 ) ;
#14366 = CARTESIAN_POINT ( 'NONE',  ( -9.746805135440405721, 0.000000000000000000, 2.897894885223375461 ) ) ;
#14367 = DIRECTION ( 'NONE',  ( 0.9999697198139515519, 0.000000000000000000, 0.007781995580013368816 ) ) ;
#14368 = VERTEX_POINT ( 'NONE', #17142 ) ;
#14369 = CARTESIAN_POINT ( 'NONE',  ( -13.93117922710646539, 24.61510576898210445, -3.677906343404563572 ) ) ;
#14370 = DIRECTION ( 'NONE',  ( 0.5449076811759707706, 0.6444004775717708799, -0.5364919789714476250 ) ) ;
#14371 = DIRECTION ( 'NONE',  ( -0.6427681459581293666, -0.7660444431189770143, -0.005002170337467561935 ) ) ;
#14372 = DIRECTION ( 'NONE',  ( 0.005961354470445682716, -0.6427876096865404731, -0.7660212471507180654 ) ) ;
#14373 = VERTEX_POINT ( 'NONE', #8626 ) ;
#14374 = LINE ( 'NONE', #27988, #25659 ) ;
#14375 = ORIENTED_EDGE ( 'NONE', *, *, #56069, .F. ) ;
#14376 = PLANE ( 'NONE',  #6862 ) ;
#14377 = EDGE_CURVE ( 'NONE', #41210, #16962, #17985, .T. ) ;
#14378 = DIRECTION ( 'NONE',  ( 0.6427681459581294776, -0.7660444431189769032, 0.005002170337467562802 ) ) ;
#14379 = ORIENTED_EDGE ( 'NONE', *, *, #30791, .F. ) ;
#14380 = FACE_OUTER_BOUND ( 'NONE', #47605, .T. ) ;
#14381 = EDGE_CURVE ( 'NONE', #22565, #38766, #8920, .T. ) ;
#14382 = ORIENTED_EDGE ( 'NONE', *, *, #15105, .F. ) ;
#14383 = VERTEX_POINT ( 'NONE', #53195 ) ;
#14384 = ORIENTED_EDGE ( 'NONE', *, *, #30299, .T. ) ;
#14385 = CARTESIAN_POINT ( 'NONE',  ( -27.99202758151029613, 16.49707118653253346, 4.690121163682637651 ) ) ;
#14386 = ORIENTED_EDGE ( 'NONE', *, *, #51082, .F. ) ;
#14387 = EDGE_CURVE ( 'NONE', #8966, #28311, #4164, .T. ) ;
#14388 = VERTEX_POINT ( 'NONE', #48916 ) ;
#14389 = FACE_OUTER_BOUND ( 'NONE', #43151, .T. ) ;
#14390 = DIRECTION ( 'NONE',  ( 0.007781995580012663651, 0.000000000000000000, -0.9999697198139515519 ) ) ;
#14392 = ADVANCED_FACE ( 'NONE', ( #48648 ), #22786, .F. ) ;
#14391 = VERTEX_POINT ( 'NONE', #5472 ) ;
#14393 = EDGE_CURVE ( 'NONE', #44862, #18734, #49179, .T. ) ;
#14394 = ADVANCED_FACE ( 'NONE', ( #1496 ), #27619, .F. ) ;
#14395 = ORIENTED_EDGE ( 'NONE', *, *, #55203, .F. ) ;
#14396 = CARTESIAN_POINT ( 'NONE',  ( -3.360905869600907092, 1.712176620043476140E-14, -4.599999999999999645 ) ) ;
#14397 = ORIENTED_EDGE ( 'NONE', *, *, #19755, .F. ) ;
#14398 = ORIENTED_EDGE ( 'NONE', *, *, #25470, .F. ) ;
#14399 = LINE ( 'NONE', #31711, #51038 ) ;
#14400 = CARTESIAN_POINT ( 'NONE',  ( -15.60102546347950536, 0.000000000000000000, 12.95077420755565356 ) ) ;
#14401 = CARTESIAN_POINT ( 'NONE',  ( -12.75342118059741026, 0.000000000000000000, 5.290495179008689597 ) ) ;
#14402 = CARTESIAN_POINT ( 'NONE',  ( -16.36686713028141682, -0.1191753592594189115, 4.793039409183453614 ) ) ;
#14403 = VERTEX_POINT ( 'NONE', #27913 ) ;
#14404 = LINE ( 'NONE', #6998, #44671 ) ;
#14405 = ORIENTED_EDGE ( 'NONE', *, *, #5787, .F. ) ;
#14406 = AXIS2_PLACEMENT_3D ( 'NONE', #27053, #44362, #655 ) ;
#14407 = EDGE_CURVE ( 'NONE', #28407, #35510, #27322, .T. ) ;
#14408 = DIRECTION ( 'NONE',  ( 0.6427681459581294776, -0.7660444431189769032, 0.005002170337467562802 ) ) ;
#14409 = EDGE_CURVE ( 'NONE', #27150, #45223, #44939, .T. ) ;
#14410 = DIRECTION ( 'NONE',  ( -0.9999697198139514409, -0.000000000000000000, -0.007781995580013368816 ) ) ;
#14411 = DIRECTION ( 'NONE',  ( 0.9999697198139515519, 0.000000000000000000, 0.007781995580013368816 ) ) ;
#14412 = DIRECTION ( 'NONE',  ( 0.007781995580012663651, 0.000000000000000000, -0.9999697198139515519 ) ) ;
#14413 = EDGE_CURVE ( 'NONE', #2309, #18910, #10598, .T. ) ;
#14414 = CARTESIAN_POINT ( 'NONE',  ( -13.69131713479542967, 0.000000000000000000, 6.391192465245965515 ) ) ;
#14415 = CARTESIAN_POINT ( 'NONE',  ( -27.99923088623136636, 0.000000000000000000, 7.757173251277078130 ) ) ;
#14416 = VERTEX_POINT ( 'NONE', #2020 ) ;
#14417 = CARTESIAN_POINT ( 'NONE',  ( -19.60834386242827776, 0.000000000000000000, 4.298478389818581213 ) ) ;
#14418 = ORIENTED_EDGE ( 'NONE', *, *, #8216, .T. ) ;
#14419 = ADVANCED_FACE ( 'NONE', ( #31865 ), #6058, .F. ) ;
#14420 = CARTESIAN_POINT ( 'NONE',  ( -15.90510428694561718, -0.1191753592594205907, 5.165965024209228318 ) ) ;
#14421 = LINE ( 'NONE', #53570, #18730 ) ;
#14422 = CARTESIAN_POINT ( 'NONE',  ( -19.32568712495613639, 5.629170628041515023, 4.009084898942861130 ) ) ;
#14423 = FACE_OUTER_BOUND ( 'NONE', #48996, .T. ) ;
#14424 = ADVANCED_FACE ( 'NONE', ( #36402 ), #45471, .F. ) ;
#14425 = CARTESIAN_POINT ( 'NONE',  ( -9.075990533167328067, 0.000000000000000000, 10.41622904950343909 ) ) ;
#14426 = CARTESIAN_POINT ( 'NONE',  ( -66.31760998578604926, 3.414724497084775940E-15, -0.1846293804859178989 ) ) ;
#14427 = ORIENTED_EDGE ( 'NONE', *, *, #246, .F. ) ;
#14428 = CARTESIAN_POINT ( 'NONE',  ( -28.19207438693690904, 14.64952330200006259, 4.723338118696758237 ) ) ;
#14429 = LINE ( 'NONE', #6193, #12208 ) ;
#14430 = DIRECTION ( 'NONE',  ( 0.6427681459581294776, -0.7660444431189769032, 0.005002170337467562802 ) ) ;
#14431 = CARTESIAN_POINT ( 'NONE',  ( -29.86352658060627618, 0.000000000000000000, 8.481329010720569883 ) ) ;
#14432 = DIRECTION ( 'NONE',  ( 0.9999697198139515519, 0.000000000000000000, 0.007781995580013368816 ) ) ;
#14433 = CARTESIAN_POINT ( 'NONE',  ( -10.94028622754223967, 0.000000000000000000, 11.14038480894692995 ) ) ;
#14434 = LINE ( 'NONE', #14981, #3835 ) ;
#14435 = CARTESIAN_POINT ( 'NONE',  ( -17.18579816256228554, 0.000000000000000000, 3.457174062837659712 ) ) ;
#14436 = CARTESIAN_POINT ( 'NONE',  ( 2.072287782118878319, 0.000000000000000000, -2.950529333540147015 ) ) ;
#14437 = ORIENTED_EDGE ( 'NONE', *, *, #15621, .F. ) ;
#14438 = VERTEX_POINT ( 'NONE', #1757 ) ;
#14439 = ORIENTED_EDGE ( 'NONE', *, *, #55422, .F. ) ;
#14440 = ORIENTED_EDGE ( 'NONE', *, *, #19188, .T. ) ;
#14441 = ORIENTED_EDGE ( 'NONE', *, *, #52843, .F. ) ;
#14442 = LINE ( 'NONE', #6469, #9670 ) ;
#14443 = CARTESIAN_POINT ( 'NONE',  ( -8.575880816922197170, 0.000000000000000000, 5.861663847473516320 ) ) ;
#14444 = ADVANCED_FACE ( 'NONE', ( #14301 ), #23621, .F. ) ;
#14445 = EDGE_CURVE ( 'NONE', #5292, #36795, #49753, .T. ) ;
#14446 = EDGE_LOOP ( 'NONE', ( #7319, #1070, #45576, #37626 ) ) ;
#14447 = ORIENTED_EDGE ( 'NONE', *, *, #1863, .T. ) ;
#14448 = EDGE_LOOP ( 'NONE', ( #43822, #14513, #29833, #51984, #56125 ) ) ;
#14449 = EDGE_CURVE ( 'NONE', #43897, #12199, #40936, .T. ) ;
#14450 = FACE_OUTER_BOUND ( 'NONE', #10162, .T. ) ;
#14451 = LINE ( 'NONE', #27494, #21895 ) ;
#14452 = PLANE ( 'NONE',  #22310 ) ;
#14453 = VERTEX_POINT ( 'NONE', #6582 ) ;
#14454 = DIRECTION ( 'NONE',  ( 0.005961354470445682716, -0.6427876096865404731, -0.7660212471507180654 ) ) ;
#14455 = ORIENTED_EDGE ( 'NONE', *, *, #25709, .F. ) ;
#14456 = DIRECTION ( 'NONE',  ( 0.5364919789714477361, 0.6444004775717706579, 0.5449076811759711036 ) ) ;
#14457 = CARTESIAN_POINT ( 'NONE',  ( -27.06552663992790997, 0.000000000000000000, 7.195101427592543786 ) ) ;
#14458 = CARTESIAN_POINT ( 'NONE',  ( -9.110551994824897193, 0.000000000000000000, 3.538847790438064411 ) ) ;
#14459 = DIRECTION ( 'NONE',  ( -0.7660212471507179544, -0.6427876096865405842, -0.005961354470445141482 ) ) ;
#14460 = CARTESIAN_POINT ( 'NONE',  ( -20.76273478851211607, 4.495856970884009485, 12.32473963750469359 ) ) ;
#14461 = CARTESIAN_POINT ( 'NONE',  ( -18.16733880988877914, -1.165603555308156514, 3.900943620346350116 ) ) ;
#14462 = DIRECTION ( 'NONE',  ( -0.5364919789714478471, 0.6444004775717705469, -0.5449076811759709926 ) ) ;
#14463 = ORIENTED_EDGE ( 'NONE', *, *, #18114, .T. ) ;
#14464 = LINE ( 'NONE', #36316, #7441 ) ;
#14465 = ORIENTED_EDGE ( 'NONE', *, *, #34594, .F. ) ;
#14466 = EDGE_LOOP ( 'NONE', ( #49061, #37905, #27081, #21159 ) ) ;
#14467 = EDGE_CURVE ( 'NONE', #41178, #5706, #23898, .T. ) ;
#14468 = DIRECTION ( 'NONE',  ( 0.7660212471507180654, -0.6427876096865404731, 0.005961354470445141482 ) ) ;
#14469 = PLANE ( 'NONE',  #561 ) ;
#14470 = DIRECTION ( 'NONE',  ( 0.5449076811759707706, 0.6444004775717708799, -0.5364919789714476250 ) ) ;
#14471 = PLANE ( 'NONE',  #38622 ) ;
#14472 = CARTESIAN_POINT ( 'NONE',  ( -20.91752765554880966, 5.305366725996514710, 4.637740859931800408 ) ) ;
#14473 = EDGE_CURVE ( 'NONE', #51439, #9864, #52881, .T. ) ;
#14474 = CARTESIAN_POINT ( 'NONE',  ( -23.33849165029409889, 0.000000000000000000, 5.946783852668351855 ) ) ;
#14475 = DIRECTION ( 'NONE',  ( -0.5000000000000015543, 0.8660254037844378194, 0.000000000000000000 ) ) ;
#14476 = FACE_OUTER_BOUND ( 'NONE', #9528, .T. ) ;
#14478 = ADVANCED_FACE ( 'NONE', ( #44369 ), #1193, .F. ) ;
#14477 =( NAMED_UNIT ( * ) SI_UNIT ( $, .STERADIAN. ) SOLID_ANGLE_UNIT ( ) );
#14479 = LINE ( 'NONE', #19844, #46846 ) ;
#14480 = ORIENTED_EDGE ( 'NONE', *, *, #7427, .T. ) ;
#14481 = CARTESIAN_POINT ( 'NONE',  ( -15.03495456790438389, -0.1191753592594197858, 12.77051346725278158 ) ) ;
#14482 = CARTESIAN_POINT ( 'NONE',  ( 5.057731014323089802, -1.114607557371862567, -2.289010529401726224 ) ) ;
#14484 = EDGE_CURVE ( 'NONE', #6551, #8206, #32983, .T. ) ;
#14483 = CARTESIAN_POINT ( 'NONE',  ( -70.10219403106212610, -1.000000000000000666, -7.503912900124007912 ) ) ;
#14485 = DIRECTION ( 'NONE',  ( 0.007781995580012663651, -3.146120232559066537E-19, -0.9999697198139514409 ) ) ;
#14486 = EDGE_CURVE ( 'NONE', #31864, #46689, #16220, .T. ) ;
#14487 = CARTESIAN_POINT ( 'NONE',  ( -20.28887480193589354, 0.000000000000000000, 4.662514410496616968 ) ) ;
#14488 = CARTESIAN_POINT ( 'NONE',  ( 2.072287782118878319, 0.000000000000000000, -2.950529333540147015 ) ) ;
#14489 = DIRECTION ( 'NONE',  ( -0.5449076811759708816, 0.6444004775717707689, 0.5364919789714475140 ) ) ;
#14490 = ORIENTED_EDGE ( 'NONE', *, *, #41667, .F. ) ;
#14491 = ORIENTED_EDGE ( 'NONE', *, *, #26090, .T. ) ;
#14492 = PLANE ( 'NONE',  #10581 ) ;
#14493 = DIRECTION ( 'NONE',  ( -0.6427681459581293666, -0.7660444431189770143, -0.005002170337467561935 ) ) ;
#14494 = ORIENTED_EDGE ( 'NONE', *, *, #17975, .F. ) ;
#14495 = PLANE ( 'NONE',  #24976 ) ;
#14496 = EDGE_LOOP ( 'NONE', ( #8817, #38861, #19699, #40208 ) ) ;
#14497 = DIRECTION ( 'NONE',  ( 0.5449076811759707706, 0.6444004775717708799, -0.5364919789714476250 ) ) ;
#14498 = ORIENTED_EDGE ( 'NONE', *, *, #13468, .T. ) ;
#14499 = ORIENTED_EDGE ( 'NONE', *, *, #27808, .T. ) ;
#14500 = ORIENTED_EDGE ( 'NONE', *, *, #18748, .F. ) ;
#14501 = LINE ( 'NONE', #14245, #14798 ) ;
#14502 = DIRECTION ( 'NONE',  ( 0.007781995580012663651, -3.146120232559066537E-19, -0.9999697198139514409 ) ) ;
#14503 = CARTESIAN_POINT ( 'NONE',  ( -16.33317936670417225, 0.000000000000000000, 13.31440848639340224 ) ) ;
#14504 = EDGE_CURVE ( 'NONE', #883, #37296, #55390, .T. ) ;
#14505 = CARTESIAN_POINT ( 'NONE',  ( -10.68050938174386566, 0.000000000000000000, 3.459966708907908473 ) ) ;
#14506 = ORIENTED_EDGE ( 'NONE', *, *, #49719, .T. ) ;
#14507 = ORIENTED_EDGE ( 'NONE', *, *, #33185, .F. ) ;
#14508 = EDGE_CURVE ( 'NONE', #44205, #29912, #50004, .T. ) ;
#14509 = EDGE_CURVE ( 'NONE', #48572, #21088, #46899, .T. ) ;
#14510 = DIRECTION ( 'NONE',  ( -0.9999697198139514409, -0.000000000000000000, -0.007781995580013368816 ) ) ;
#14511 = ORIENTED_EDGE ( 'NONE', *, *, #19422, .T. ) ;
#14512 = PLANE ( 'NONE',  #23723 ) ;
#14513 = ORIENTED_EDGE ( 'NONE', *, *, #20725, .T. ) ;
#14514 = CARTESIAN_POINT ( 'NONE',  ( 5.618093942130458096, -1.050357310661657939, 2.260478214906367800 ) ) ;
#14515 = FACE_OUTER_BOUND ( 'NONE', #49183, .T. ) ;
#14516 = ORIENTED_EDGE ( 'NONE', *, *, #20459, .T. ) ;
#14517 = CARTESIAN_POINT ( 'NONE',  ( -50.45472955569960760, 3.742236127018431890, -5.000000000000000000 ) ) ;
#14518 = ORIENTED_EDGE ( 'NONE', *, *, #22764, .T. ) ;
#14519 = EDGE_CURVE ( 'NONE', #45407, #39622, #51133, .T. ) ;
#14520 = CARTESIAN_POINT ( 'NONE',  ( -61.70068505767310540, 8.059153983834628221, -5.000000000000000000 ) ) ;
#14521 = ORIENTED_EDGE ( 'NONE', *, *, #15449, .F. ) ;
#14522 = CARTESIAN_POINT ( 'NONE',  ( -18.39746900504187010, 0.000000000000000000, 14.03700784672088808 ) ) ;
#14523 = PLANE ( 'NONE',  #32064 ) ;
#14524 = CARTESIAN_POINT ( 'NONE',  ( -13.99298162533602152, -5.536956232915663634, 11.20436947665652561 ) ) ;
#14525 = ORIENTED_EDGE ( 'NONE', *, *, #21246, .T. ) ;
#14526 = CARTESIAN_POINT ( 'NONE',  ( -14.53418602446461705, -0.1191753592594185784, 8.131290385575372426 ) ) ;
#14527 = LINE ( 'NONE', #10266, #46839 ) ;
#14528 = DIRECTION ( 'NONE',  ( -0.9999697198139514409, -0.000000000000000000, -0.007781995580013368816 ) ) ;
#14529 = CARTESIAN_POINT ( 'NONE',  ( -56.75000000000000711, 4.436543092327784876, -2.449489742783172996 ) ) ;
#14530 = EDGE_CURVE ( 'NONE', #31964, #16497, #3447, .T. ) ;
#14531 = DIRECTION ( 'NONE',  ( 0.005002170337468016433, -0.7660444431189770143, -0.6427681459581293666 ) ) ;
#14532 = LINE ( 'NONE', #49159, #30656 ) ;
#14533 = VECTOR ( 'NONE', #13830, 999.9999999999998863 ) ;
#14534 = CARTESIAN_POINT ( 'NONE',  ( -66.74269294525370810, -11.36137123595008269, -2.738438791722735743 ) ) ;
#14535 = VERTEX_POINT ( 'NONE', #16489 ) ;
#14537 = ADVANCED_FACE ( 'NONE', ( #41226 ), #29272, .F. ) ;
#14536 = DIRECTION ( 'NONE',  ( 0.007781995580012662783, 0.000000000000000000, -0.9999697198139514409 ) ) ;
#14538 = LINE ( 'NONE', #22770, #18665 ) ;
#14539 = CARTESIAN_POINT ( 'NONE',  ( -66.50839368374572302, 1.729872094282792178E-11, -1.425848428484772112 ) ) ;
#14540 = ORIENTED_EDGE ( 'NONE', *, *, #46673, .F. ) ;
#14541 = LINE ( 'NONE', #22773, #10257 ) ;
#14542 = DIRECTION ( 'NONE',  ( 0.005961354470445682716, -0.6427876096865404731, -0.7660212471507180654 ) ) ;
#14543 = ORIENTED_EDGE ( 'NONE', *, *, #44578, .F. ) ;
#14544 = EDGE_CURVE ( 'NONE', #98, #23644, #36987, .T. ) ;
#14545 = DIRECTION ( 'NONE',  ( -0.8531650599175527594, 0.4028455766673922356, 0.3313982828793700652 ) ) ;
#14546 = DIRECTION ( 'NONE',  ( 0.9999697198139515519, 0.000000000000000000, 0.007781995580013368816 ) ) ;
#14547 = DIRECTION ( 'NONE',  ( 0.000000000000000000, 0.000000000000000000, 1.000000000000000000 ) ) ;
#14548 = ORIENTED_EDGE ( 'NONE', *, *, #4648, .T. ) ;
#14549 = ORIENTED_EDGE ( 'NONE', *, *, #28827, .T. ) ;
#14550 = DIRECTION ( 'NONE',  ( 0.000000000000000000, -0.000000000000000000, -1.000000000000000000 ) ) ;
#14551 = LINE ( 'NONE', #35306, #23265 ) ;
#14552 = EDGE_CURVE ( 'NONE', #53976, #19985, #24884, .T. ) ;
#14553 = CARTESIAN_POINT ( 'NONE',  ( -13.35659999714346391, 4.010151117816509903, 8.650819319289523079 ) ) ;
#14554 = CARTESIAN_POINT ( 'NONE',  ( -27.06552663992790997, 0.000000000000000000, 7.195101427592543786 ) ) ;
#14555 = ORIENTED_EDGE ( 'NONE', *, *, #45635, .F. ) ;
#14556 = CARTESIAN_POINT ( 'NONE',  ( -14.10280672071693431, -0.1191753592594197858, 12.40843558753103792 ) ) ;
#14558 = ADVANCED_FACE ( 'NONE', ( #50848 ), #42050, .F. ) ;
#14557 = VERTEX_POINT ( 'NONE', #15643 ) ;
#14559 = DIRECTION ( 'NONE',  ( 0.7091055728196409280, -0.7051023234936394379, 0.000000000000000000 ) ) ;
#14560 = ADVANCED_FACE ( 'NONE', ( #41759 ), #28434, .F. ) ;
#14561 = CARTESIAN_POINT ( 'NONE',  ( -61.21055533376208047, 7.871010810323351592, 5.000000000000012434 ) ) ;
#14562 = ORIENTED_EDGE ( 'NONE', *, *, #33488, .T. ) ;
#14563 = DIRECTION ( 'NONE',  ( 0.9999697198139515519, 0.000000000000000000, 0.007781995580013368816 ) ) ;
#14564 = EDGE_CURVE ( 'NONE', #35585, #50536, #46589, .T. ) ;
#14565 = CARTESIAN_POINT ( 'NONE',  ( -12.16214263066938628, -0.1191753592594194527, 1.871104989033428145 ) ) ;
#14566 = DIRECTION ( 'NONE',  ( 0.005002170337468016433, -0.7660444431189770143, -0.6427681459581293666 ) ) ;
#14567 = EDGE_LOOP ( 'NONE', ( #17519, #15163, #8552, #40935 ) ) ;
#14568 = PLANE ( 'NONE',  #23044 ) ;
#14569 = EDGE_CURVE ( 'NONE', #15522, #4593, #25039, .T. ) ;
#14570 = VERTEX_POINT ( 'NONE', #7408 ) ;
#14571 = ADVANCED_FACE ( 'NONE', ( #54537 ), #46301, .F. ) ;
#14572 = VECTOR ( 'NONE', #36978, 1000.000000000000000 ) ;
#14573 = VERTEX_POINT ( 'NONE', #55132 ) ;
#14574 = EDGE_LOOP ( 'NONE', ( #31349, #18424, #23126, #15081 ) ) ;
#14575 = CARTESIAN_POINT ( 'NONE',  ( -13.79019121975177953, 5.143464774974014553, 1.874406862791435868 ) ) ;
#14576 = ORIENTED_EDGE ( 'NONE', *, *, #41013, .F. ) ;
#14577 = CARTESIAN_POINT ( 'NONE',  ( 2.072287782118878319, 0.000000000000000000, -2.950529333540147015 ) ) ;
#14578 = ORIENTED_EDGE ( 'NONE', *, *, #31657, .T. ) ;
#14579 = PLANE ( 'NONE',  #22204 ) ;
#14580 = FACE_OUTER_BOUND ( 'NONE', #739, .T. ) ;
#14581 = ADVANCED_FACE ( 'NONE', ( #7155 ), #15948, .F. ) ;
#14582 = VERTEX_POINT ( 'NONE', #8549 ) ;
#14583 = PLANE ( 'NONE',  #5920 ) ;
#14584 = ORIENTED_EDGE ( 'NONE', *, *, #39050, .F. ) ;
#14585 = ADVANCED_FACE ( 'NONE', ( #26155 ), #51440, .F. ) ;
#14586 = FACE_OUTER_BOUND ( 'NONE', #45585, .T. ) ;
#14587 = LINE ( 'NONE', #949, #21129 ) ;
#14588 = DIRECTION ( 'NONE',  ( -0.9999697198139514409, -0.000000000000000000, -0.007781995580013368816 ) ) ;
#14589 = CARTESIAN_POINT ( 'NONE',  ( -12.80458192191714595, 0.000000000000000000, 11.86454056839041726 ) ) ;
#14590 = CARTESIAN_POINT ( 'NONE',  ( 4.912750499197525045, -1.131233082521085231, 2.061810099490657411 ) ) ;
#14591 = DIRECTION ( 'NONE',  ( 0.000000000000000000, -1.000000000000000000, 0.000000000000000000 ) ) ;
#14592 = EDGE_LOOP ( 'NONE', ( #40508, #17564, #50492, #16722, #47042 ) ) ;
#14593 = ORIENTED_EDGE ( 'NONE', *, *, #6603, .F. ) ;
#14594 = VECTOR ( 'NONE', #8021, 1000.000000000000227 ) ;
#14595 = LINE ( 'NONE', #10343, #35509 ) ;
#14596 = PLANE ( 'NONE',  #23051 ) ;
#14597 = CARTESIAN_POINT ( 'NONE',  ( -8.563136055001720592, -0.006715909454105468447, 4.948137389168624445 ) ) ;
#14598 = FACE_OUTER_BOUND ( 'NONE', #3552, .T. ) ;
#14599 = ORIENTED_EDGE ( 'NONE', *, *, #22202, .T. ) ;
#14600 = LINE ( 'NONE', #6115, #34018 ) ;
#14601 = CARTESIAN_POINT ( 'NONE',  ( -8.700467249853277352, 8.479997087537753941, 6.597930524618322856 ) ) ;
#14602 = ORIENTED_EDGE ( 'NONE', *, *, #47322, .T. ) ;
#14603 = DIRECTION ( 'NONE',  ( -0.5364919789714478471, 0.6444004775717705469, -0.5449076811759709926 ) ) ;
#14604 = DIRECTION ( 'NONE',  ( 0.9999697198139515519, 0.000000000000000000, 0.007781995580013368816 ) ) ;
#14605 = ORIENTED_EDGE ( 'NONE', *, *, #22656, .T. ) ;
#14606 = CARTESIAN_POINT ( 'NONE',  ( -18.95295033115275984, 3.524445264749009876, 3.931453028570905062 ) ) ;
#14607 = LINE ( 'NONE', #14894, #645 ) ;
#14608 = AXIS2_PLACEMENT_3D ( 'NONE', #49445, #1986, #27290 ) ;
#14609 = ADVANCED_FACE ( 'NONE', ( #47744 ), #25882, .F. ) ;
#14610 = CARTESIAN_POINT ( 'NONE',  ( -20.72220850017212612, -3.594132820645660420, 10.62972551294390655 ) ) ;
#14611 = DIRECTION ( 'NONE',  ( -0.5364919789714478471, 0.6444004775717705469, -0.5449076811759709926 ) ) ;
#14612 = VECTOR ( 'NONE', #6194, 1000.000000000000227 ) ;
#14613 = LINE ( 'NONE', #721, #10199 ) ;
#14614 = ORIENTED_EDGE ( 'NONE', *, *, #10082, .F. ) ;
#14615 = ORIENTED_EDGE ( 'NONE', *, *, #38186, .T. ) ;
#14616 = DIRECTION ( 'NONE',  ( 0.007781995580012663651, 0.000000000000000000, -0.9999697198139515519 ) ) ;
#14617 = CARTESIAN_POINT ( 'NONE',  ( -14.61903452936159553, 0.000000000000000000, 6.183966697747157681 ) ) ;
#14618 = CARTESIAN_POINT ( 'NONE',  ( -16.93359685305117779, 0.000000000000000000, 5.057958029133816424 ) ) ;
#14619 = ADVANCED_FACE ( 'NONE', ( #43210 ), #47152, .F. ) ;
#14620 = DIRECTION ( 'NONE',  ( -0.5364919789714478471, 0.6444004775717705469, -0.5449076811759709926 ) ) ;
#14621 = FACE_BOUND ( 'NONE', #13037, .T. ) ;
#14623 = ADVANCED_FACE ( 'NONE', ( #3707 ), #16787, .F. ) ;
#14622 = ORIENTED_EDGE ( 'NONE', *, *, #15972, .F. ) ;
#14624 = LINE ( 'NONE', #41839, #28351 ) ;
#14625 = CARTESIAN_POINT ( 'NONE',  ( -14.01701317841955508, 0.000000000000000000, 2.326005055450897085 ) ) ;
#14626 = ADVANCED_FACE ( 'NONE', ( #21874 ), #9100, .F. ) ;
#14627 = DIRECTION ( 'NONE',  ( -0.9999697198139514409, -0.000000000000000000, -0.007781995580013368816 ) ) ;
#14628 = FACE_OUTER_BOUND ( 'NONE', #12299, .T. ) ;
#14629 = ORIENTED_EDGE ( 'NONE', *, *, #5408, .T. ) ;
#14630 = DIRECTION ( 'NONE',  ( -0.6427681459581293666, -0.7660444431189770143, -0.005002170337467561935 ) ) ;
#14631 = EDGE_LOOP ( 'NONE', ( #22682, #30445, #37276, #54148 ) ) ;
#14632 = PLANE ( 'NONE',  #38594 ) ;
#14633 = DIRECTION ( 'NONE',  ( 0.005961354470445682716, -0.6427876096865404731, -0.7660212471507180654 ) ) ;
#14634 = ORIENTED_EDGE ( 'NONE', *, *, #10222, .T. ) ;
#14635 = VECTOR ( 'NONE', #13575, 1000.000000000000000 ) ;
#14636 = VECTOR ( 'NONE', #37404, 999.9999999999998863 ) ;
#14637 = DIRECTION ( 'NONE',  ( -0.5449076811759708816, 0.6444004775717707689, 0.5364919789714475140 ) ) ;
#14638 = EDGE_CURVE ( 'NONE', #52700, #7363, #4004, .T. ) ;
#14639 = ORIENTED_EDGE ( 'NONE', *, *, #4568, .F. ) ;
#14640 = EDGE_CURVE ( 'NONE', #36151, #47897, #36794, .T. ) ;
#14641 = EDGE_LOOP ( 'NONE', ( #7295, #23252, #34923, #13459 ) ) ;
#14642 = ORIENTED_EDGE ( 'NONE', *, *, #9911, .F. ) ;
#14643 = CARTESIAN_POINT ( 'NONE',  ( -15.87975247367846166, 0.000000000000000000, 2.850166870931599927 ) ) ;
#14644 = ORIENTED_EDGE ( 'NONE', *, *, #26199, .F. ) ;
#14645 = ORIENTED_EDGE ( 'NONE', *, *, #45225, .F. ) ;
#14646 = DIRECTION ( 'NONE',  ( 0.9999697198139515519, 0.000000000000000000, 0.007781995580013368816 ) ) ;
#14647 = LINE ( 'NONE', #7176, #16776 ) ;
#14648 = EDGE_LOOP ( 'NONE', ( #18775, #4101, #5259, #4853 ) ) ;
#14649 = EDGE_CURVE ( 'NONE', #4593, #33120, #4842, .T. ) ;
#14650 = ORIENTED_EDGE ( 'NONE', *, *, #25851, .F. ) ;
#14651 = DIRECTION ( 'NONE',  ( 0.5364919789714477361, 0.6444004775717706579, 0.5449076811759711036 ) ) ;
#14652 = VERTEX_POINT ( 'NONE', #17076 ) ;
#14653 = ORIENTED_EDGE ( 'NONE', *, *, #51519, .T. ) ;
#14654 = VECTOR ( 'NONE', #26118, 1000.000000000000000 ) ;
#14655 = ADVANCED_FACE ( 'NONE', ( #30704 ), #30123, .F. ) ;
#14656 = CARTESIAN_POINT ( 'NONE',  ( -46.52156441860571334, 5.799038105676371124, -5.000000000000000000 ) ) ;
#14657 = DIRECTION ( 'NONE',  ( -0.9999697198139514409, -0.000000000000000000, -0.007781995580013368816 ) ) ;
#14658 = LINE ( 'NONE', #6421, #50464 ) ;
#14659 = CARTESIAN_POINT ( 'NONE',  ( -15.50102849149811135, -0.1191753592594197858, 12.95155240711365430 ) ) ;
#14660 = VERTEX_POINT ( 'NONE', #48001 ) ;
#14661 = LINE ( 'NONE', #6424, #23790 ) ;
#14662 = ORIENTED_EDGE ( 'NONE', *, *, #447, .F. ) ;
#14663 = LINE ( 'NONE', #31452, #52913 ) ;
#14664 = CARTESIAN_POINT ( 'NONE',  ( -14.17164195355221246, 0.000000000000000000, 8.403440829061754158 ) ) ;
#14665 = LINE ( 'NONE', #33331, #24063 ) ;
#14666 = CARTESIAN_POINT ( 'NONE',  ( -11.80247261326225505, 0.000000000000000000, 2.512565135777569569 ) ) ;
#14667 = DIRECTION ( 'NONE',  ( 0.5364919789714477361, 0.6444004775717706579, 0.5449076811759711036 ) ) ;
#14668 = LINE ( 'NONE', #5888, #16858 ) ;
#14669 = ORIENTED_EDGE ( 'NONE', *, *, #8092, .F. ) ;
#14670 = CARTESIAN_POINT ( 'NONE',  ( -17.74404816805336793, 0.000000000000000000, 3.574322630375089460 ) ) ;
#14671 = ORIENTED_EDGE ( 'NONE', *, *, #12209, .F. ) ;
#14672 = VECTOR ( 'NONE', #41635, 1000.000000000000114 ) ;
#14673 = AXIS2_PLACEMENT_3D ( 'NONE', #7756, #24238, #37560 ) ;
#14674 = DIRECTION ( 'NONE',  ( -0.6427681459581293666, -0.7660444431189770143, -0.005002170337467561935 ) ) ;
#14675 = CARTESIAN_POINT ( 'NONE',  ( -11.52752152373586192, -2.137015261443160341, 1.290819977936035423 ) ) ;
#14676 = CARTESIAN_POINT ( 'NONE',  ( -14.20280369269832832, 0.000000000000000000, 12.40765738797303719 ) ) ;
#14677 = ADVANCED_FACE ( 'NONE', ( #29856 ), #39502, .T. ) ;
#14678 = CARTESIAN_POINT ( 'NONE',  ( -22.40478740399063895, 0.000000000000000000, 5.384712028983816623 ) ) ;
#14679 = CARTESIAN_POINT ( 'NONE',  ( -9.110551994824897193, 0.000000000000000000, 3.538847790438064411 ) ) ;
#14680 = CARTESIAN_POINT ( 'NONE',  ( -69.45075675106602375, 5.509042946743876566E-16, 8.251517284182453338 ) ) ;
#14681 = EDGE_CURVE ( 'NONE', #14310, #27973, #42896, .T. ) ;
#14682 = AXIS2_PLACEMENT_3D ( 'NONE', #48389, #6362, #44153 ) ;
#14683 = ORIENTED_EDGE ( 'NONE', *, *, #36430, .F. ) ;
#14684 = ADVANCED_FACE ( 'NONE', ( #34653 ), #38657, .F. ) ;
#14685 = CARTESIAN_POINT ( 'NONE',  ( -24.27063949748155380, 0.000000000000000000, 6.308861732390097288 ) ) ;
#14686 = LINE ( 'NONE', #32008, #15896 ) ;
#14687 = CARTESIAN_POINT ( 'NONE',  ( -10.42868029727597801, 0.000000000000000000, 5.108580793885948879 ) ) ;
#14688 = EDGE_CURVE ( 'NONE', #41032, #7012, #8853, .T. ) ;
#14689 = EDGE_CURVE ( 'NONE', #39029, #12809, #4563, .T. ) ;
#14690 = EDGE_CURVE ( 'NONE', #15779, #31243, #30950, .T. ) ;
#14691 = LINE ( 'NONE', #54162, #13771 ) ;
#14692 = VECTOR ( 'NONE', #40585, 1000.000000000000227 ) ;
#14693 = CARTESIAN_POINT ( 'NONE',  ( -24.26908309836554878, 0.000000000000000000, 6.108867788427308376 ) ) ;
#14694 = CARTESIAN_POINT ( 'NONE',  ( -8.609916609573598834, 0.000000000000000000, 10.23519010964256637 ) ) ;
#14695 = VECTOR ( 'NONE', #21066, 999.9999999999998863 ) ;
#14696 = DIRECTION ( 'NONE',  ( -0.5364919789714478471, 0.6444004775717705469, -0.5449076811759709926 ) ) ;
#14697 = DIRECTION ( 'NONE',  ( 0.007781995580012663651, 0.000000000000000000, -0.9999697198139515519 ) ) ;
#14698 = ORIENTED_EDGE ( 'NONE', *, *, #2406, .F. ) ;
#14699 = ORIENTED_EDGE ( 'NONE', *, *, #3711, .F. ) ;
#14700 = EDGE_CURVE ( 'NONE', #24619, #24312, #53122, .T. ) ;
#14701 = EDGE_CURVE ( 'NONE', #5503, #12315, #27543, .T. ) ;
#14702 = ORIENTED_EDGE ( 'NONE', *, *, #51993, .T. ) ;
#14703 = VERTEX_POINT ( 'NONE', #23303 ) ;
#14704 = ORIENTED_EDGE ( 'NONE', *, *, #528, .T. ) ;
#14705 = EDGE_CURVE ( 'NONE', #21025, #41679, #53940, .T. ) ;
#14706 = ORIENTED_EDGE ( 'NONE', *, *, #12248, .T. ) ;
#14707 = LINE ( 'NONE', #53348, #42323 ) ;
#14708 = DIRECTION ( 'NONE',  ( 0.005002170337468016433, -0.7660444431189770143, -0.6427681459581293666 ) ) ;
#14709 = VECTOR ( 'NONE', #3938, 999.9999999999998863 ) ;
#14710 = EDGE_CURVE ( 'NONE', #11058, #47950, #18768, .T. ) ;
#14711 = VECTOR ( 'NONE', #31782, 1000.000000000000227 ) ;
#14712 = ORIENTED_EDGE ( 'NONE', *, *, #10020, .T. ) ;
#14713 = ORIENTED_EDGE ( 'NONE', *, *, #39584, .T. ) ;
#14714 = ORIENTED_EDGE ( 'NONE', *, *, #18085, .F. ) ;
#14715 = VECTOR ( 'NONE', #43355, 999.9999999999998863 ) ;
#14716 = AXIS2_PLACEMENT_3D ( 'NONE', #19001, #14468, #52783 ) ;
#14717 = FACE_OUTER_BOUND ( 'NONE', #18628, .T. ) ;
#14718 = PLANE ( 'NONE',  #112 ) ;
#14719 = CARTESIAN_POINT ( 'NONE',  ( -9.442067484779661513, -0.1191753592594197858, 10.59804618892231254 ) ) ;
#14720 = ORIENTED_EDGE ( 'NONE', *, *, #10895, .T. ) ;
#14721 = DIRECTION ( 'NONE',  ( -0.005961354470445682716, -0.6427876096865404731, 0.7660212471507180654 ) ) ;
#14722 = ORIENTED_EDGE ( 'NONE', *, *, #16608, .F. ) ;
#14723 = DIRECTION ( 'NONE',  ( 0.9999697198139515519, 0.000000000000000000, 0.007781995580013368816 ) ) ;
#14724 = AXIS2_PLACEMENT_3D ( 'NONE', #18020, #38775, #52930 ) ;
#14725 = CARTESIAN_POINT ( 'NONE',  ( -13.53673582514181106, 0.000000000000000000, 12.22817484722816772 ) ) ;
#14726 = LINE ( 'NONE', #32050, #23678 ) ;
#14727 = LINE ( 'NONE', #49082, #43276 ) ;
#14728 = FACE_OUTER_BOUND ( 'NONE', #8017, .T. ) ;
#14729 = DIRECTION ( 'NONE',  ( -0.5364919789714478471, 0.6444004775717705469, -0.5449076811759709926 ) ) ;
#14730 = FACE_OUTER_BOUND ( 'NONE', #23081, .T. ) ;
#14731 = ORIENTED_EDGE ( 'NONE', *, *, #48013, .F. ) ;
#14732 = PLANE ( 'NONE',  #41888 ) ;
#14733 = ORIENTED_EDGE ( 'NONE', *, *, #26406, .T. ) ;
#14734 = CARTESIAN_POINT ( 'NONE',  ( -16.21389796751076773, 3.038739411681508518, 2.883008631584717207 ) ) ;
#14735 = DIRECTION ( 'NONE',  ( -0.5449076811759708816, 0.6444004775717707689, 0.5364919789714475140 ) ) ;
#14736 = DIRECTION ( 'NONE',  ( 0.9999697198139515519, 0.000000000000000000, 0.007781995580013368816 ) ) ;
#14737 = DIRECTION ( 'NONE',  ( -0.5364919789714478471, 0.6444004775717705469, -0.5449076811759709926 ) ) ;
#14738 = EDGE_CURVE ( 'NONE', #3988, #46922, #1956, .T. ) ;
#14739 = AXIS2_PLACEMENT_3D ( 'NONE', #10777, #49392, #10511 ) ;
#14740 = LINE ( 'NONE', #32070, #42266 ) ;
#14741 = PLANE ( 'NONE',  #40373 ) ;
#14742 = CARTESIAN_POINT ( 'NONE',  ( -13.66964236114244891, 0.000000000000000000, 3.606030598478824789 ) ) ;
#14743 = CARTESIAN_POINT ( 'NONE',  ( -10.47421230394850866, 0.000000000000000000, 10.95934586908605723 ) ) ;
#14744 = LINE ( 'NONE', #54212, #39605 ) ;
#14745 = ORIENTED_EDGE ( 'NONE', *, *, #26199, .T. ) ;
#14746 = VECTOR ( 'NONE', #2938, 999.9999999999998863 ) ;
#14747 = DIRECTION ( 'NONE',  ( 0.007781995580012663651, 0.000000000000000000, -0.9999697198139515519 ) ) ;
#14748 = LINE ( 'NONE', #44853, #37630 ) ;
#14749 = CARTESIAN_POINT ( 'NONE',  ( -69.18604761972393646, -0.9999999999995238253, 6.394134653913046584 ) ) ;
#14750 = EDGE_CURVE ( 'NONE', #48012, #50620, #31547, .T. ) ;
#14751 = DIRECTION ( 'NONE',  ( 0.000000000000000000, -1.000000000000000000, 0.000000000000000000 ) ) ;
#14752 = ADVANCED_FACE ( 'NONE', ( #44863 ), #14492, .F. ) ;
#14753 = ADVANCED_FACE ( 'NONE', ( #1698 ), #13915, .F. ) ;
#14754 = VECTOR ( 'NONE', #44795, 1000.000000000000114 ) ;
#14755 = CIRCLE ( 'NONE', #43758, 2.750000000000001776 ) ;
#14756 = LINE ( 'NONE', #1415, #28200 ) ;
#14757 = EDGE_CURVE ( 'NONE', #7759, #3022, #44026, .T. ) ;
#14758 = DIRECTION ( 'NONE',  ( -0.005961354470445682716, -0.6427876096865404731, 0.7660212471507180654 ) ) ;
#14759 = LINE ( 'NONE', #19853, #5701 ) ;
#14760 = ORIENTED_EDGE ( 'NONE', *, *, #13362, .F. ) ;
#14761 = VECTOR ( 'NONE', #46977, 999.9999999999998863 ) ;
#14762 = AXIS2_PLACEMENT_3D ( 'NONE', #41369, #6442, #32564 ) ;
#14763 = ORIENTED_EDGE ( 'NONE', *, *, #7252, .T. ) ;
#14764 = DIRECTION ( 'NONE',  ( -0.3583679495452925523, -0.9335804264972047406, 0.000000000000000000 ) ) ;
#14765 = LINE ( 'NONE', #45160, #48498 ) ;
#14766 = VERTEX_POINT ( 'NONE', #36092 ) ;
#14767 = DIRECTION ( 'NONE',  ( 0.7660212471507180654, -0.6427876096865404731, 0.005961354470445141482 ) ) ;
#14768 = VECTOR ( 'NONE', #3971, 1000.000000000000000 ) ;
#14769 = EDGE_LOOP ( 'NONE', ( #32335, #32394, #39109, #29441 ) ) ;
#14770 = CARTESIAN_POINT ( 'NONE',  ( -18.15140093078727901, -4.403642575758160760, 10.95967996775459952 ) ) ;
#14771 = VECTOR ( 'NONE', #15147, 1000.000000000000227 ) ;
#14772 = EDGE_CURVE ( 'NONE', #13654, #16888, #53395, .T. ) ;
#14773 = ORIENTED_EDGE ( 'NONE', *, *, #11707, .T. ) ;
#14774 = EDGE_LOOP ( 'NONE', ( #48799, #19345, #51333, #11459 ) ) ;
#14775 = ORIENTED_EDGE ( 'NONE', *, *, #20794, .T. ) ;
#14776 =( BOUNDED_CURVE ( )  B_SPLINE_CURVE ( 3, ( #20669, #17231, #51864, #38541 ),
 .UNSPECIFIED., .F., .F. ) 
 B_SPLINE_CURVE_WITH_KNOTS ( ( 4, 4 ),
 ( 5.898329122556067894, 6.668041491803113452 ),
 .UNSPECIFIED. ) 
 CURVE ( )  GEOMETRIC_REPRESENTATION_ITEM ( )  RATIONAL_B_SPLINE_CURVE ( ( 1.000000000000000000, 0.9512349561781446861, 0.9512349561781446861, 1.000000000000000000 ) ) 
 REPRESENTATION_ITEM ( '' )  );
#14777 = EDGE_CURVE ( 'NONE', #42084, #20292, #48573, .T. ) ;
#14778 = PLANE ( 'NONE',  #28404 ) ;
#14779 = LINE ( 'NONE', #44880, #8743 ) ;
#14780 = CARTESIAN_POINT ( 'NONE',  ( -69.59775774058348929, -0.6007421665236040154, 7.493101075386322307 ) ) ;
#14781 = VECTOR ( 'NONE', #52761, 999.9999999999998863 ) ;
#14782 = EDGE_CURVE ( 'NONE', #8988, #28441, #53649, .T. ) ;
#14783 = VERTEX_POINT ( 'NONE', #9687 ) ;
#14784 = ORIENTED_EDGE ( 'NONE', *, *, #45841, .F. ) ;
#14785 = VECTOR ( 'NONE', #7703, 1000.000000000000227 ) ;
#14786 = ADVANCED_FACE ( 'NONE', ( #1123 ), #40326, .T. ) ;
#14787 = CARTESIAN_POINT ( 'NONE',  ( -19.60834386242827776, 0.000000000000000000, 4.298478389818581213 ) ) ;
#14788 = ORIENTED_EDGE ( 'NONE', *, *, #20035, .T. ) ;
#14789 = VECTOR ( 'NONE', #26293, 999.9999999999998863 ) ;
#14790 = CARTESIAN_POINT ( 'NONE',  ( -13.07066190154808361, 0.000000000000000000, 12.04713590736729678 ) ) ;
#14791 = EDGE_LOOP ( 'NONE', ( #23787, #45872, #34345, #13064 ) ) ;
#14792 = DIRECTION ( 'NONE',  ( 0.005961354470445682716, -0.6427876096865404731, -0.7660212471507180654 ) ) ;
#14793 = LINE ( 'NONE', #40647, #40311 ) ;
#14794 = VECTOR ( 'NONE', #53905, 1000.000000000000227 ) ;
#14795 = VECTOR ( 'NONE', #47273, 1000.000000000000114 ) ;
#14796 = ORIENTED_EDGE ( 'NONE', *, *, #6740, .F. ) ;
#14797 = DIRECTION ( 'NONE',  ( 0.000000000000000000, -1.000000000000000000, 0.000000000000000000 ) ) ;
#14798 = VECTOR ( 'NONE', #39514, 1000.000000000000114 ) ;
#14799 = LINE ( 'NONE', #18492, #25462 ) ;
#14800 = VECTOR ( 'NONE', #9090, 999.9999999999998863 ) ;
#14801 = ORIENTED_EDGE ( 'NONE', *, *, #30217, .T. ) ;
#14802 = PLANE ( 'NONE',  #44097 ) ;
#14803 = FACE_OUTER_BOUND ( 'NONE', #304, .T. ) ;
#14804 = DIRECTION ( 'NONE',  ( -0.9999697198139514409, -0.000000000000000000, -0.007781995580013368816 ) ) ;
#14805 = VERTEX_POINT ( 'NONE', #45159 ) ;
#14806 = CARTESIAN_POINT ( 'NONE',  ( -9.075990533167328067, 0.000000000000000000, 10.41622904950343909 ) ) ;
#14807 = LINE ( 'NONE', #20157, #11498 ) ;
#14808 = DIRECTION ( 'NONE',  ( 0.005961354470445682716, -0.6427876096865404731, -0.7660212471507180654 ) ) ;
#14809 = VECTOR ( 'NONE', #31199, 1000.000000000000114 ) ;
#14810 = DIRECTION ( 'NONE',  ( 0.007781995580012663651, 0.000000000000000000, -0.9999697198139515519 ) ) ;
#14811 = VECTOR ( 'NONE', #752, 1000.000000000000227 ) ;
#14812 = CARTESIAN_POINT ( 'NONE',  ( -11.51026827947273112, 0.7721120973665037690, 1.128276403237633563 ) ) ;
#14813 = DIRECTION ( 'NONE',  ( 0.2426528472758542054, 0.7422098413412800966, 0.6246952433987894571 ) ) ;
#14814 = CARTESIAN_POINT ( 'NONE',  ( -65.69817947455537421, -11.24159248525151078, 5.466724623770281788 ) ) ;
#14815 = EDGE_LOOP ( 'NONE', ( #40149, #53222, #6120, #56061, #14122 ) ) ;
#14816 = CARTESIAN_POINT ( 'NONE',  ( 2.072287782118878319, 0.000000000000000000, -2.950529333540147015 ) ) ;
#14817 = CARTESIAN_POINT ( 'NONE',  ( -13.66257659974260186, 0.000000000000000000, 2.698095432668320637 ) ) ;
#14818 = CARTESIAN_POINT ( 'NONE',  ( -65.72289477776887168, -3.035766082959412415E-14, 1.903866651545371269 ) ) ;
#14819 = VERTEX_POINT ( 'NONE', #32093 ) ;
#14820 = DIRECTION ( 'NONE',  ( -0.7660212471507179544, -0.6427876096865405842, -0.005961354470445141482 ) ) ;
#14821 = CARTESIAN_POINT ( 'NONE',  ( -12.55055318312933643, 0.000000000000000000, 4.922741874866930267 ) ) ;
#14822 = AXIS2_PLACEMENT_3D ( 'NONE', #23937, #37017, #32483 ) ;
#14823 = EDGE_CURVE ( 'NONE', #21642, #13331, #49408, .T. ) ;
#14824 = CARTESIAN_POINT ( 'NONE',  ( -14.62205743691809801, 3.362543313726510164, 2.254352670595775265 ) ) ;
#14825 = VECTOR ( 'NONE', #24200, 999.9999999999998863 ) ;
#14826 = EDGE_CURVE ( 'NONE', #15779, #30378, #22723, .T. ) ;
#14827 = EDGE_CURVE ( 'NONE', #44163, #5769, #14234, .T. ) ;
#14828 = DIRECTION ( 'NONE',  ( -0.6427681459581293666, -0.7660444431189770143, -0.005002170337467561935 ) ) ;
#14829 = CARTESIAN_POINT ( 'NONE',  ( -56.40853634832227925, 6.684187361877747868, 2.244562702769390405 ) ) ;
#14830 = ORIENTED_EDGE ( 'NONE', *, *, #1072, .F. ) ;
#14831 = EDGE_LOOP ( 'NONE', ( #35627, #4113, #47204, #18258 ) ) ;
#14832 = CARTESIAN_POINT ( 'NONE',  ( 0.000000000000000000, 2.000000000000000000, -2.125000000000000000 ) ) ;
#14833 = AXIS2_PLACEMENT_3D ( 'NONE', #17488, #33753, #16169 ) ;
#14834 = PLANE ( 'NONE',  #45913 ) ;
#14835 = VECTOR ( 'NONE', #1164, 999.9999999999998863 ) ;
#14836 = PLANE ( 'NONE',  #50154 ) ;
#14837 = VECTOR ( 'NONE', #39706, 1000.000000000000227 ) ;
#14838 = ORIENTED_EDGE ( 'NONE', *, *, #41988, .T. ) ;
#14839 = DIRECTION ( 'NONE',  ( 0.5449076811759707706, 0.6444004775717708799, -0.5364919789714476250 ) ) ;
#14840 = ORIENTED_EDGE ( 'NONE', *, *, #30580, .F. ) ;
#14841 = FACE_OUTER_BOUND ( 'NONE', #33369, .T. ) ;
#14842 = AXIS2_PLACEMENT_3D ( 'NONE', #40048, #27012, #10236 ) ;
#14843 = VECTOR ( 'NONE', #37672, 999.9999999999998863 ) ;
#14844 = ORIENTED_EDGE ( 'NONE', *, *, #22781, .T. ) ;
#14845 = PLANE ( 'NONE',  #2043 ) ;
#14846 = PLANE ( 'NONE',  #45889 ) ;
#14847 = FACE_OUTER_BOUND ( 'NONE', #43495, .T. ) ;
#14848 = ORIENTED_EDGE ( 'NONE', *, *, #9650, .F. ) ;
#14849 = DIRECTION ( 'NONE',  ( 0.005961354470445682716, -0.6427876096865404731, -0.7660212471507180654 ) ) ;
#14850 = EDGE_LOOP ( 'NONE', ( #23495, #9926, #32115, #9968 ) ) ;
#14851 = EDGE_CURVE ( 'NONE', #51400, #20591, #5682, .T. ) ;
#14852 = ORIENTED_EDGE ( 'NONE', *, *, #544, .T. ) ;
#14853 = ORIENTED_EDGE ( 'NONE', *, *, #6691, .F. ) ;
#14854 = CARTESIAN_POINT ( 'NONE',  ( -25.20123094555300369, 0.000000000000000000, 6.470945668149052032 ) ) ;
#14855 = VECTOR ( 'NONE', #22550, 1000.000000000000114 ) ;
#14856 = ADVANCED_FACE ( 'NONE', ( #32388 ), #33975, .F. ) ;
#14857 = ORIENTED_EDGE ( 'NONE', *, *, #52194, .F. ) ;
#14858 = PLANE ( 'NONE',  #8492 ) ;
#14859 = EDGE_LOOP ( 'NONE', ( #20763, #21521, #39292, #31255 ) ) ;
#14860 = AXIS2_PLACEMENT_3D ( 'NONE', #49080, #18419, #54192 ) ;
#14861 = CARTESIAN_POINT ( 'NONE',  ( -16.99924723426068951, 0.000000000000000000, 13.49389102713827171 ) ) ;
#14862 = LINE ( 'NONE', #27940, #14993 ) ;
#14863 = ORIENTED_EDGE ( 'NONE', *, *, #8349, .T. ) ;
#14864 = ADVANCED_FACE ( 'NONE', ( #8137 ), #21183, .F. ) ;
#14865 = DIRECTION ( 'NONE',  ( 0.6427681459581294776, -0.7660444431189769032, 0.005002170337467562802 ) ) ;
#14866 = VECTOR ( 'NONE', #14956, 1000.000000000000227 ) ;
#14867 = EDGE_LOOP ( 'NONE', ( #28677, #36190, #50935, #24287 ) ) ;
#14868 = DIRECTION ( 'NONE',  ( 0.005961354470445682716, -0.6427876096865404731, -0.7660212471507180654 ) ) ;
#14869 = LINE ( 'NONE', #36438, #40193 ) ;
#14870 = DIRECTION ( 'NONE',  ( -0.7660212471507179544, -0.6427876096865405842, -0.005961354470445141482 ) ) ;
#14871 = CARTESIAN_POINT ( 'NONE',  ( -10.74029228357944987, 0.000000000000000000, 11.14194120806293320 ) ) ;
#14872 = CARTESIAN_POINT ( 'NONE',  ( -9.743931081935125249, 0.000000000000000000, 2.528585181965609774 ) ) ;
#14873 = VECTOR ( 'NONE', #20506, 1000.000000000000114 ) ;
#14874 = DIRECTION ( 'NONE',  ( 0.7660212471507180654, -0.6427876096865404731, 0.005961354470445141482 ) ) ;
#14875 = CARTESIAN_POINT ( 'NONE',  ( -57.52614991588065152, -8.291364278369165675, -2.999999999999996003 ) ) ;
#14876 = ORIENTED_EDGE ( 'NONE', *, *, #40168, .T. ) ;
#14877 = AXIS2_PLACEMENT_3D ( 'NONE', #17298, #16459, #56211 ) ;
#14878 = ORIENTED_EDGE ( 'NONE', *, *, #49399, .T. ) ;
#14879 = DIRECTION ( 'NONE',  ( -0.7660212471507179544, -0.6427876096865405842, -0.005961354470445141482 ) ) ;
#14880 = FACE_OUTER_BOUND ( 'NONE', #7405, .T. ) ;
#14881 = CARTESIAN_POINT ( 'NONE',  ( -14.40467031787239449, 0.000000000000000000, 4.338974580574337381 ) ) ;
#14882 = VECTOR ( 'NONE', #38599, 999.9999999999998863 ) ;
#14883 = AXIS2_PLACEMENT_3D ( 'NONE', #16344, #51825, #50980 ) ;
#14884 = CARTESIAN_POINT ( 'NONE',  ( -45.77156441860525149, 4.499999999999981348, -5.000000000000000000 ) ) ;
#14885 = VERTEX_POINT ( 'NONE', #33680 ) ;
#14886 = DIRECTION ( 'NONE',  ( -0.7660212471507179544, -0.6427876096865405842, -0.005961354470445141482 ) ) ;
#14887 = DIRECTION ( 'NONE',  ( 0.000000000000000000, -1.000000000000000000, 0.000000000000000000 ) ) ;
#14888 = EDGE_LOOP ( 'NONE', ( #22548, #37622, #16752, #48402 ) ) ;
#14889 = LINE ( 'NONE', #6372, #2976 ) ;
#14890 = EDGE_CURVE ( 'NONE', #17736, #6150, #42212, .T. ) ;
#14891 = LINE ( 'NONE', #26838, #38525 ) ;
#14892 = EDGE_LOOP ( 'NONE', ( #43845, #2482, #53668, #7960 ) ) ;
#14893 = CARTESIAN_POINT ( 'NONE',  ( -14.71857576103236198, 2.876837460659007473, 7.319896171222362469 ) ) ;
#14894 = CARTESIAN_POINT ( 'NONE',  ( -15.29900336458644894, -4.403642575758165201, 2.683474326561374745 ) ) ;
#14895 = CARTESIAN_POINT ( 'NONE',  ( -33.59211796935609584, 0.000000000000000000, 9.929640529607549837 ) ) ;
#14896 = ADVANCED_FACE ( 'NONE', ( #17207 ), #2252, .F. ) ;
#14897 = PLANE ( 'NONE',  #21463 ) ;
#14898 = LINE ( 'NONE', #45825, #45575 ) ;
#14899 = AXIS2_PLACEMENT_3D ( 'NONE', #48759, #27738, #10703 ) ;
#14900 = ORIENTED_EDGE ( 'NONE', *, *, #393, .T. ) ;
#14901 = VECTOR ( 'NONE', #6001, 999.9999999999998863 ) ;
#14902 = ORIENTED_EDGE ( 'NONE', *, *, #41119, .F. ) ;
#14903 = DIRECTION ( 'NONE',  ( -0.7660212471507179544, -0.6427876096865405842, -0.005961354470445141482 ) ) ;
#14904 = CARTESIAN_POINT ( 'NONE',  ( -26.13493519185646008, 0.000000000000000000, 7.033017491833586377 ) ) ;
#14905 = DIRECTION ( 'NONE',  ( 0.007781995580012663651, -3.146120232559066537E-19, -0.9999697198139514409 ) ) ;
#14906 = AXIS2_PLACEMENT_3D ( 'NONE', #24561, #2979, #2445 ) ;
#14907 = LINE ( 'NONE', #53273, #17371 ) ;
#14908 = CARTESIAN_POINT ( 'NONE',  ( -18.67697421479882181, -0.1191753592594197858, 4.036397482078229793 ) ) ;
#14909 = VECTOR ( 'NONE', #11778, 999.9999999999998863 ) ;
#14910 = VERTEX_POINT ( 'NONE', #36926 ) ;
#14911 = PLANE ( 'NONE',  #21999 ) ;
#14912 = EDGE_CURVE ( 'NONE', #34828, #35980, #50988, .T. ) ;
#14913 = FACE_OUTER_BOUND ( 'NONE', #46185, .T. ) ;
#14914 = CARTESIAN_POINT ( 'NONE',  ( -25.20200914511100265, -0.1191753592594197858, 6.570942640130446932 ) ) ;
#14915 = ORIENTED_EDGE ( 'NONE', *, *, #51726, .F. ) ;
#14916 = VECTOR ( 'NONE', #3101, 999.9999999999998863 ) ;
#14917 = DIRECTION ( 'NONE',  ( 0.000000000000000000, -0.000000000000000000, -1.000000000000000000 ) ) ;
#14918 = ORIENTED_EDGE ( 'NONE', *, *, #43946, .F. ) ;
#14919 = LINE ( 'NONE', #41845, #50388 ) ;
#14920 = DIRECTION ( 'NONE',  ( 0.5449076811759707706, 0.6444004775717708799, -0.5364919789714476250 ) ) ;
#14921 = VECTOR ( 'NONE', #9021, 1000.000000000000000 ) ;
#14922 = ORIENTED_EDGE ( 'NONE', *, *, #2260, .F. ) ;
#14923 = DIRECTION ( 'NONE',  ( 0.7660212471507180654, -0.6427876096865404731, 0.005961354470445141482 ) ) ;
#14924 = VERTEX_POINT ( 'NONE', #49942 ) ;
#14925 = VECTOR ( 'NONE', #34268, 1000.000000000000114 ) ;
#14926 = ORIENTED_EDGE ( 'NONE', *, *, #39444, .F. ) ;
#14927 = ORIENTED_EDGE ( 'NONE', *, *, #10751, .F. ) ;
#14928 = DIRECTION ( 'NONE',  ( 0.005961354470445682716, -0.6427876096865404731, -0.7660212471507180654 ) ) ;
#14929 = VECTOR ( 'NONE', #56048, 1000.000000000000227 ) ;
#14930 = VERTEX_POINT ( 'NONE', #12414 ) ;
#14931 = ORIENTED_EDGE ( 'NONE', *, *, #50994, .T. ) ;
#14932 = CARTESIAN_POINT ( 'NONE',  ( -26.13337879274045505, 0.000000000000000000, 6.833023547870798353 ) ) ;
#14933 = ORIENTED_EDGE ( 'NONE', *, *, #27520, .T. ) ;
#14934 = ORIENTED_EDGE ( 'NONE', *, *, #18167, .T. ) ;
#14935 = CARTESIAN_POINT ( 'NONE',  ( -15.09844010454417429, -0.8417996532631562001, 2.719210182726563119 ) ) ;
#14936 = EDGE_CURVE ( 'NONE', #1131, #33580, #25733, .T. ) ;
#14937 = EDGE_LOOP ( 'NONE', ( #27847, #2891, #9570, #15299 ) ) ;
#14938 = ORIENTED_EDGE ( 'NONE', *, *, #7360, .F. ) ;
#14939 = AXIS2_PLACEMENT_3D ( 'NONE', #26932, #5346, #22653 ) ;
#14940 = LINE ( 'NONE', #36250, #36545 ) ;
#14941 = VECTOR ( 'NONE', #2282, 1000.000000000000227 ) ;
#14942 = DIRECTION ( 'NONE',  ( 0.000000000000000000, -1.000000000000000000, 0.000000000000000000 ) ) ;
#14943 = CARTESIAN_POINT ( 'NONE',  ( -20.54204810873173415, 0.000000000000000000, 4.860550213503115558 ) ) ;
#14944 = DIRECTION ( 'NONE',  ( 0.007781995580012663651, -3.146120232559066537E-19, -0.9999697198139514409 ) ) ;
#14945 = ORIENTED_EDGE ( 'NONE', *, *, #23281, .F. ) ;
#14946 = FACE_OUTER_BOUND ( 'NONE', #41411, .T. ) ;
#14947 = VECTOR ( 'NONE', #15925, 999.9999999999998863 ) ;
#14948 = ORIENTED_EDGE ( 'NONE', *, *, #42402, .T. ) ;
#14949 = EDGE_CURVE ( 'NONE', #52494, #33064, #42495, .T. ) ;
#14950 = CARTESIAN_POINT ( 'NONE',  ( -13.36712169493445579, -2.622721114510659035, 6.178507914287525438 ) ) ;
#14951 = AXIS2_PLACEMENT_3D ( 'NONE', #6848, #27883, #36374 ) ;
#14952 = EDGE_CURVE ( 'NONE', #8247, #18922, #55838, .T. ) ;
#14953 = EDGE_CURVE ( 'NONE', #40596, #6333, #20644, .T. ) ;
#14954 = DIRECTION ( 'NONE',  ( -0.005002170337468016433, -0.7660444431189770143, 0.6427681459581293666 ) ) ;
#14955 = CARTESIAN_POINT ( 'NONE',  ( 3.004435629306332345, 0.000000000000000000, -3.312607213261892003 ) ) ;
#14956 = DIRECTION ( 'NONE',  ( -0.9999697198139514409, -0.000000000000000000, -0.007781995580013368816 ) ) ;
#14957 = VECTOR ( 'NONE', #21357, 1000.000000000000000 ) ;
#14958 = CARTESIAN_POINT ( 'NONE',  ( -18.82594708035263764, 2.229229656569007290, 7.852503942761646982 ) ) ;
#14959 = ORIENTED_EDGE ( 'NONE', *, *, #8881, .F. ) ;
#14960 = CARTESIAN_POINT ( 'NONE',  ( -19.71200609458190911, -1.984075165378300865, 6.895443337863062183 ) ) ;
#14961 = ADVANCED_FACE ( 'NONE', ( #28101 ), #6519, .F. ) ;
#14962 = ORIENTED_EDGE ( 'NONE', *, *, #35003, .F. ) ;
#14963 = VECTOR ( 'NONE', #25555, 1000.000000000000114 ) ;
#14964 = CARTESIAN_POINT ( 'NONE',  ( -27.06708303904391144, 0.000000000000000000, 7.395095371555332697 ) ) ;
#14965 = DIRECTION ( 'NONE',  ( -0.9999697198139514409, -0.000000000000000000, -0.007781995580013368816 ) ) ;
#14966 = EDGE_CURVE ( 'NONE', #52332, #45792, #21490, .T. ) ;
#14967 = CARTESIAN_POINT ( 'NONE',  ( -25.20200914511100265, -0.1191753592594197858, 6.570942640130446932 ) ) ;
#14968 = FACE_OUTER_BOUND ( 'NONE', #27788, .T. ) ;
#14969 = ADVANCED_FACE ( 'NONE', ( #12678 ), #15324, .F. ) ;
#14970 = CARTESIAN_POINT ( 'NONE',  ( -9.542064456761055524, 0.000000000000000000, 10.59726798936431180 ) ) ;
#14971 = AXIS2_PLACEMENT_3D ( 'NONE', #12024, #51219, #3521 ) ;
#14972 = VECTOR ( 'NONE', #8377, 1000.000000000000227 ) ;
#14973 = ORIENTED_EDGE ( 'NONE', *, *, #26735, .F. ) ;
#14974 = LINE ( 'NONE', #19787, #7619 ) ;
#14975 = PLANE ( 'NONE',  #46663 ) ;
#14976 = DIRECTION ( 'NONE',  ( -0.005961354470445682716, -0.6427876096865404731, 0.7660212471507180654 ) ) ;
#14977 = EDGE_CURVE ( 'NONE', #24834, #25732, #29989, .T. ) ;
#14978 = LINE ( 'NONE', #33137, #24621 ) ;
#14979 = FACE_OUTER_BOUND ( 'NONE', #14831, .T. ) ;
#14980 = CARTESIAN_POINT ( 'NONE',  ( -13.66545065324788411, 0.000000000000000000, 3.067405135926084103 ) ) ;
#14981 = CARTESIAN_POINT ( 'NONE',  ( -18.92804305261459774, 1.257817950434005461, 6.297909381879228441 ) ) ;
#14982 = VECTOR ( 'NONE', #54921, 999.9999999999998863 ) ;
#14983 = EDGE_CURVE ( 'NONE', #10480, #18734, #32637, .T. ) ;
#14984 = CARTESIAN_POINT ( 'NONE',  ( -23.27598484286411562, 19.08968574485540515, 4.485782763162093900 ) ) ;
#14985 = AXIS2_PLACEMENT_3D ( 'NONE', #50741, #15280, #24078 ) ;
#14986 = LINE ( 'NONE', #5911, #27442 ) ;
#14987 = VECTOR ( 'NONE', #14210, 1000.000000000000227 ) ;
#14988 = VERTEX_POINT ( 'NONE', #3321 ) ;
#14989 = VECTOR ( 'NONE', #50195, 999.9999999999998863 ) ;
#14990 = ORIENTED_EDGE ( 'NONE', *, *, #17536, .T. ) ;
#14991 = ORIENTED_EDGE ( 'NONE', *, *, #20753, .F. ) ;
#14992 = AXIS2_PLACEMENT_3D ( 'NONE', #48784, #34872, #26333 ) ;
#14993 = VECTOR ( 'NONE', #29029, 1000.000000000000114 ) ;
#14994 = ORIENTED_EDGE ( 'NONE', *, *, #1927, .T. ) ;
#14995 = VECTOR ( 'NONE', #50841, 999.9999999999998863 ) ;
#14996 = ORIENTED_EDGE ( 'NONE', *, *, #35473, .F. ) ;
#14997 = DIRECTION ( 'NONE',  ( -0.005961354470445682716, -0.6427876096865404731, 0.7660212471507180654 ) ) ;
#14998 = CARTESIAN_POINT ( 'NONE',  ( -27.06708303904391144, 0.000000000000000000, 7.395095371555332697 ) ) ;
#14999 = AXIS2_PLACEMENT_3D ( 'NONE', #49036, #47933, #5059 ) ;
#15000 = VECTOR ( 'NONE', #24219, 999.9999999999998863 ) ;
#15001 = ORIENTED_EDGE ( 'NONE', *, *, #48184, .T. ) ;
#15002 = CARTESIAN_POINT ( 'NONE',  ( -10.79984652870423822, -0.1191753592594181482, 5.944359460172861098 ) ) ;
#15003 = EDGE_CURVE ( 'NONE', #32474, #29764, #55263, .T. ) ;
#15004 = ORIENTED_EDGE ( 'NONE', *, *, #12364, .F. ) ;
#15005 = VECTOR ( 'NONE', #38084, 1000.000000000000227 ) ;
#15006 = VECTOR ( 'NONE', #48902, 1000.000000000000227 ) ;
#15007 = CARTESIAN_POINT ( 'NONE',  ( -20.59866850025657925, -1.813211359398156919, 7.658942858085559635 ) ) ;
#15008 = DIRECTION ( 'NONE',  ( 0.5364919789714477361, 0.6444004775717706579, 0.5449076811759711036 ) ) ;
#15009 = DIRECTION ( 'NONE',  ( 0.007781995580012663651, -3.146120232559066537E-19, -0.9999697198139514409 ) ) ;
#15010 = ORIENTED_EDGE ( 'NONE', *, *, #4512, .F. ) ;
#15011 = DIRECTION ( 'NONE',  ( -0.005961354470445682716, -0.6427876096865404731, 0.7660212471507180654 ) ) ;
#15012 = EDGE_CURVE ( 'NONE', #54304, #9862, #20894, .T. ) ;
#15013 = EDGE_CURVE ( 'NONE', #37067, #39800, #42753, .T. ) ;
#15014 = PLANE ( 'NONE',  #51790 ) ;
#15015 = CARTESIAN_POINT ( 'NONE',  ( -14.98445265377928770, -0.1191753592594174960, 6.281125957518538527 ) ) ;
#15016 = ADVANCED_FACE ( 'NONE', ( #48426 ), #5290, .F. ) ;
#15017 = VECTOR ( 'NONE', #28739, 1000.000000000000000 ) ;
#15018 = DIRECTION ( 'NONE',  ( -0.005961354470445682716, -0.6427876096865404731, 0.7660212471507180654 ) ) ;
#15019 = FACE_OUTER_BOUND ( 'NONE', #15323, .T. ) ;
#15020 = CARTESIAN_POINT ( 'NONE',  ( -11.36804826722768347, 24.91136206679770382, 5.000000000000000888 ) ) ;
#15021 = DIRECTION ( 'NONE',  ( 0.6427681459581294776, -0.7660444431189769032, 0.005002170337467562802 ) ) ;
#15023 = VECTOR ( 'NONE', #11774, 999.9999999999998863 ) ;
#15022 = CARTESIAN_POINT ( 'NONE',  ( -11.87243407472968926, 0.000000000000000000, 11.50246268866867361 ) ) ;
#15024 = DIRECTION ( 'NONE',  ( -0.005961354470445682716, -0.6427876096865404731, 0.7660212471507180654 ) ) ;
#15025 = ORIENTED_EDGE ( 'NONE', *, *, #3679, .T. ) ;
#15026 = DIRECTION ( 'NONE',  ( 0.000000000000000000, -0.000000000000000000, -1.000000000000000000 ) ) ;
#15027 = ORIENTED_EDGE ( 'NONE', *, *, #29720, .T. ) ;
#15028 = VECTOR ( 'NONE', #16857, 999.9999999999998863 ) ;
#15029 = PLANE ( 'NONE',  #49204 ) ;
#15030 = CARTESIAN_POINT ( 'NONE',  ( -13.20368780991208268, 0.000000000000000000, 3.440330750951857031 ) ) ;
#15031 = CARTESIAN_POINT ( 'NONE',  ( -11.30636317915456779, -0.1191753592594197858, 11.32220194836580340 ) ) ;
#15032 = EDGE_CURVE ( 'NONE', #42375, #39726, #17788, .T. ) ;
#15033 = CARTESIAN_POINT ( 'NONE',  ( -50.02554558092695913, 3.776013638374817294, 5.000000000000000000 ) ) ;
#15034 = VECTOR ( 'NONE', #42873, 1000.000000000000114 ) ;
#15035 = DIRECTION ( 'NONE',  ( 0.005961354470445682716, -0.6427876096865404731, -0.7660212471507180654 ) ) ;
#15036 = PLANE ( 'NONE',  #40420 ) ;
#15037 = DIRECTION ( 'NONE',  ( 0.000000000000000000, -1.000000000000000000, 0.000000000000000000 ) ) ;
#15038 = ADVANCED_FACE ( 'NONE', ( #443 ), #5546, .F. ) ;
#15040 = AXIS2_PLACEMENT_3D ( 'NONE', #15676, #3191, #15987 ) ;
#15039 = DIRECTION ( 'NONE',  ( 0.007781995580012662783, 0.000000000000000000, -0.9999697198139514409 ) ) ;
#15041 = VECTOR ( 'NONE', #24535, 1000.000000000000227 ) ;
#15042 = DIRECTION ( 'NONE',  ( 0.005002170337468016433, -0.7660444431189770143, -0.6427681459581293666 ) ) ;
#15043 = PLANE ( 'NONE',  #12112 ) ;
#15044 = DIRECTION ( 'NONE',  ( 0.9999697198139515519, 0.000000000000000000, 0.007781995580013368816 ) ) ;
#15045 = CARTESIAN_POINT ( 'NONE',  ( -14.46333583037745107, 5.305366725996512045, 11.20638257342840660 ) ) ;
#15047 = VECTOR ( 'NONE', #11743, 999.9999999999998863 ) ;
#15046 = PLANE ( 'NONE',  #5119 ) ;
#15048 = EDGE_CURVE ( 'NONE', #10989, #6706, #735, .T. ) ;
#15049 = VECTOR ( 'NONE', #37084, 1000.000000000000227 ) ;
#15050 = DIRECTION ( 'NONE',  ( 0.007781995580012663651, 0.000000000000000000, -0.9999697198139515519 ) ) ;
#15051 = VECTOR ( 'NONE', #17556, 1000.000000000000227 ) ;
#15052 = DIRECTION ( 'NONE',  ( -0.6246952433987894571, 0.7422098413412802076, 0.2426528472758539834 ) ) ;
#15053 = FACE_OUTER_BOUND ( 'NONE', #2536, .T. ) ;
#15054 = LINE ( 'NONE', #19585, #40120 ) ;
#15055 = ORIENTED_EDGE ( 'NONE', *, *, #12412, .T. ) ;
#15056 = VECTOR ( 'NONE', #13784, 1000.000000000000227 ) ;
#15057 = VECTOR ( 'NONE', #1881, 999.9999999999998863 ) ;
#15058 = VERTEX_POINT ( 'NONE', #9543 ) ;
#15059 = DIRECTION ( 'NONE',  ( 0.9999697198139515519, 0.000000000000000000, 0.007781995580013368816 ) ) ;
#15060 = DIRECTION ( 'NONE',  ( 0.5449076811759707706, 0.6444004775717708799, -0.5364919789714476250 ) ) ;
#15061 = ORIENTED_EDGE ( 'NONE', *, *, #42046, .T. ) ;
#15062 = PLANE ( 'NONE',  #13185 ) ;
#15063 = ORIENTED_EDGE ( 'NONE', *, *, #9170, .T. ) ;
#15064 = CARTESIAN_POINT ( 'NONE',  ( -18.68645613183151610, -0.07073876987044309950, 9.535660383697532438 ) ) ;
#15065 = VECTOR ( 'NONE', #25194, 1000.000000000000227 ) ;
#15066 = ORIENTED_EDGE ( 'NONE', *, *, #29239, .T. ) ;
#15067 = VERTEX_POINT ( 'NONE', #22864 ) ;
#15068 = ORIENTED_EDGE ( 'NONE', *, *, #47064, .T. ) ;
#15069 = LINE ( 'NONE', #15891, #22990 ) ;
#15070 = DIRECTION ( 'NONE',  ( -0.7660212471507179544, -0.6427876096865405842, -0.005961354470445141482 ) ) ;
#15071 = VECTOR ( 'NONE', #14348, 1000.000000000000227 ) ;
#15072 = CARTESIAN_POINT ( 'NONE',  ( -50.99228148001754590, 2.341865487272627000, 5.000000000000000000 ) ) ;
#15073 = EDGE_CURVE ( 'NONE', #30649, #12259, #39070, .T. ) ;
#15074 = ORIENTED_EDGE ( 'NONE', *, *, #44815, .F. ) ;
#15075 = VECTOR ( 'NONE', #41684, 999.9999999999998863 ) ;
#15077 = ORIENTED_EDGE ( 'NONE', *, *, #54244, .T. ) ;
#15076 = EDGE_CURVE ( 'NONE', #7467, #24071, #35374, .T. ) ;
#15078 = VECTOR ( 'NONE', #14737, 1000.000000000000000 ) ;
#15079 = VECTOR ( 'NONE', #35338, 1000.000000000000000 ) ;
#15080 = CARTESIAN_POINT ( 'NONE',  ( -18.66354898467281132, 0.000000000000000000, 14.21960318569776582 ) ) ;
#15082 = EDGE_CURVE ( 'NONE', #24541, #7274, #13778, .T. ) ;
#15081 = ORIENTED_EDGE ( 'NONE', *, *, #5466, .T. ) ;
#15083 = CARTESIAN_POINT ( 'NONE',  ( -11.87243407472968926, 0.000000000000000000, 11.50246268866867361 ) ) ;
#15084 = EDGE_LOOP ( 'NONE', ( #21560, #39163, #22190, #26461 ) ) ;
#15085 = CARTESIAN_POINT ( 'NONE',  ( -9.042720045137619067, -2.794052915596232367, 3.713477088201619924 ) ) ;
#15086 = LINE ( 'NONE', #28700, #27630 ) ;
#15087 = EDGE_CURVE ( 'NONE', #6080, #15150, #30833, .T. ) ;
#15088 = AXIS2_PLACEMENT_3D ( 'NONE', #10516, #14751, #40616 ) ;
#15089 = EDGE_CURVE ( 'NONE', #32268, #54774, #26862, .T. ) ;
#15090 = ADVANCED_FACE ( 'NONE', ( #26036 ), #8716, .F. ) ;
#15091 = ORIENTED_EDGE ( 'NONE', *, *, #7464, .F. ) ;
#15092 = VECTOR ( 'NONE', #31906, 1000.000000000000000 ) ;
#15093 = LINE ( 'NONE', #49721, #6844 ) ;
#15094 = AXIS2_PLACEMENT_3D ( 'NONE', #52822, #4577, #8566 ) ;
#15095 = PLANE ( 'NONE',  #16369 ) ;
#15096 = AXIS2_PLACEMENT_3D ( 'NONE', #39641, #30263, #52113 ) ;
#15097 = EDGE_LOOP ( 'NONE', ( #27404, #11061, #14857, #34718 ) ) ;
#15098 = PLANE ( 'NONE',  #55762 ) ;
#15099 = SURFACE_STYLE_USAGE ( .BOTH. , #45722 ) ;
#15100 = CARTESIAN_POINT ( 'NONE',  ( -21.47341775636118655, -0.1191753592594197858, 5.122631121243466090 ) ) ;
#15101 = EDGE_LOOP ( 'NONE', ( #43830, #33587, #29277, #16895 ) ) ;
#15102 = CARTESIAN_POINT ( 'NONE',  ( 2.072287782118878319, 0.000000000000000000, -2.950529333540147015 ) ) ;
#15103 = DIRECTION ( 'NONE',  ( 0.005961354470445682716, -0.6427876096865404731, -0.7660212471507180654 ) ) ;
#15104 = CARTESIAN_POINT ( 'NONE',  ( -17.73140113748535285, 0.000000000000000000, 13.85752530597602039 ) ) ;
#15105 = EDGE_CURVE ( 'NONE', #15287, #10033, #34526, .T. ) ;
#15106 = CARTESIAN_POINT ( 'NONE',  ( -13.23305999722791171, 2.229229656569007290, 5.680036664431174387 ) ) ;
#15107 = CARTESIAN_POINT ( 'NONE',  ( -22.40478740399063895, 0.000000000000000000, 5.384712028983816623 ) ) ;
#15108 = PLANE ( 'NONE',  #39733 ) ;
#15109 = AXIS2_PLACEMENT_3D ( 'NONE', #7805, #11759, #33905 ) ;
#15110 = ADVANCED_FACE ( 'NONE', ( #44185 ), #9242, .F. ) ;
#15111 = CARTESIAN_POINT ( 'NONE',  ( -66.84206714067370569, -9.493454880241955607, -1.367029069777546457 ) ) ;
#15112 = EDGE_LOOP ( 'NONE', ( #38817, #22425, #46980, #53512 ) ) ;
#15113 = FACE_OUTER_BOUND ( 'NONE', #55845, .T. ) ;
#15114 = FACE_OUTER_BOUND ( 'NONE', #39213, .T. ) ;
#15115 = ADVANCED_FACE ( 'NONE', ( #39353 ), #26563, .F. ) ;
#15116 = CARTESIAN_POINT ( 'NONE',  ( -69.65753061157268178, -0.6010127178502197021, -7.568661514997570450 ) ) ;
#15117 = EDGE_LOOP ( 'NONE', ( #22273, #42675, #43370, #31762 ) ) ;
#15118 = CARTESIAN_POINT ( 'NONE',  ( 0.09621548157177391147, -1.683565401097097070, -3.964956190634383340E-16 ) ) ;
#15119 = CARTESIAN_POINT ( 'NONE',  ( -25.20200914511100265, -0.1191753592594197858, 6.570942640130446932 ) ) ;
#15120 = VECTOR ( 'NONE', #9941, 1000.000000000000227 ) ;
#15121 = EDGE_CURVE ( 'NONE', #29959, #41646, #39655, .T. ) ;
#15122 = VECTOR ( 'NONE', #23622, 1000.000000000000227 ) ;
#15123 = LINE ( 'NONE', #42043, #19525 ) ;
#15124 = FACE_OUTER_BOUND ( 'NONE', #20907, .T. ) ;
#15125 = EDGE_CURVE ( 'NONE', #47950, #41108, #52130, .T. ) ;
#15126 = DIRECTION ( 'NONE',  ( -0.5449076811759708816, 0.6444004775717707689, 0.5364919789714475140 ) ) ;
#15127 = ORIENTED_EDGE ( 'NONE', *, *, #32947, .T. ) ;
#15128 = VECTOR ( 'NONE', #5894, 1000.000000000000114 ) ;
#15129 = ORIENTED_EDGE ( 'NONE', *, *, #23717, .T. ) ;
#15130 =( BOUNDED_SURFACE ( )  B_SPLINE_SURFACE ( 3, 2, ( 
 ( #40921, #9994, #2304 ),
 ( #18506, #19640, #23350 ),
 ( #53698, #36385, #6303 ),
 ( #54270, #40669, #35851 ),
 ( #31593, #10833, #49985 ),
 ( #19063, #27044, #14814 ),
 ( #23606, #22767, #32679 ),
 ( #36136, #10582, #49465 ),
 ( #44353, #27894, #45201 ),
 ( #2003, #36971, #5453 ),
 ( #40381, #32141, #45453 ),
 ( #18815, #19340, #53995 ),
 ( #15111, #53174, #32435 ),
 ( #14282, #14534, #53437 ),
 ( #48899, #6567, #23879 ),
 ( #27301, #44615, #5734 ),
 ( #23059, #31849, #49160 ),
 ( #10274, #27598, #44923 ),
 ( #6037, #45735, #34107 ),
 ( #3135, #20164, #15933 ),
 ( #16207, #51118, #25298 ),
 ( #12226, #24438, #11671 ),
 ( #33525, #20750, #50833 ),
 ( #6864, #37499, #7140 ) ),
 .UNSPECIFIED., .F., .F., .F. ) 
 B_SPLINE_SURFACE_WITH_KNOTS ( ( 4, 2, 2, 2, 2, 2, 2, 2, 2, 2, 2, 4 ),
 ( 3, 3 ),
 ( 0.008994972463978564287, 0.01138926720843922921, 0.01258641458066956167, 0.01378356195289989587, 0.01617785669736056253, 0.01857215144182122746, 0.02096644618628189238, 0.02336074093074255731, 0.02575503567520322223, 0.02695218304743355470, 0.02755075673354872440, 0.02814933041966389063 ),
 ( 0.000000000000000000, 1.000000000000000000 ),
 .UNSPECIFIED. ) 
 GEOMETRIC_REPRESENTATION_ITEM ( )  RATIONAL_B_SPLINE_SURFACE ( (
 ( 1.000000000000000000, 0.7302382283600511448, 1.000000000000000000),
 ( 1.000000000000000000, 0.7302057701444357729, 1.000000000000000000),
 ( 1.000000000000000000, 0.7302261543188973691, 1.000000000000000000),
 ( 1.000000000000000000, 0.7302340627759303926, 1.000000000000000000),
 ( 1.000000000000000000, 0.7302358193541355069, 1.000000000000000000),
 ( 1.000000000000000000, 0.7302356584975112641, 1.000000000000000000),
 ( 1.000000000000000000, 0.7302336981016072093, 1.000000000000000000),
 ( 1.000000000000000000, 0.7302244465200464774, 1.000000000000000000),
 ( 1.000000000000000000, 0.7302382397014047788, 1.000000000000000000),
 ( 1.000000000000000000, 0.7302438375889021005, 1.000000000000000000),
 ( 1.000000000000000000, 0.7302379409284335265, 1.000000000000000000),
 ( 1.000000000000000000, 0.7302249128382346521, 1.000000000000000000),
 ( 1.000000000000000000, 0.7302266904902104949, 1.000000000000000000),
 ( 1.000000000000000000, 0.7302305284537528030, 1.000000000000000000),
 ( 1.000000000000000000, 0.7302278475275691960, 1.000000000000000000),
 ( 1.000000000000000000, 0.7302208473896385499, 1.000000000000000000),
 ( 1.000000000000000000, 0.7302205818819856864, 1.000000000000000000),
 ( 1.000000000000000000, 0.7302413824365678874, 1.000000000000000000),
 ( 1.000000000000000000, 0.7302489349981282629, 1.000000000000000000),
 ( 1.000000000000000000, 0.7302381596259744923, 1.000000000000000000),
 ( 1.000000000000000000, 0.7302138215212032879, 1.000000000000000000),
 ( 1.000000000000000000, 0.7302588551347022339, 1.000000000000000000),
 ( 1.000000000000000000, 0.7302821861409102278, 1.000000000000000000),
 ( 1.000000000000000000, 0.7303030204721967511, 1.000000000000000000) ) ) 
 REPRESENTATION_ITEM ( '' )  SURFACE ( )  );
#15131 = CARTESIAN_POINT ( 'NONE',  ( -17.93139508144814442, 0.000000000000000000, 13.85596890686001537 ) ) ;
#15132 = B_SPLINE_CURVE_WITH_KNOTS ( 'NONE', 3,
 ( #31658, #28208, #32212, #19707 ),
 .UNSPECIFIED., .F., .F.,
 ( 4, 4 ),
 ( 0.000000000000000000, 0.0001521986025861482247 ),
 .UNSPECIFIED. ) ;
#15133 = CARTESIAN_POINT ( 'NONE',  ( -13.53673582514181106, 0.000000000000000000, 12.22817484722816772 ) ) ;
#15134 = VECTOR ( 'NONE', #8756, 1000.000000000000000 ) ;
#15135 = EDGE_LOOP ( 'NONE', ( #10463, #1704, #1310, #16242 ) ) ;
#15136 = FACE_OUTER_BOUND ( 'NONE', #24912, .T. ) ;
#15137 = ORIENTED_EDGE ( 'NONE', *, *, #24928, .T. ) ;
#15138 = LINE ( 'NONE', #50010, #39218 ) ;
#15139 = VECTOR ( 'NONE', #37695, 999.9999999999998863 ) ;
#15140 = AXIS2_PLACEMENT_3D ( 'NONE', #28361, #15573, #20108 ) ;
#15141 = ORIENTED_EDGE ( 'NONE', *, *, #11568, .T. ) ;
#15142 = EDGE_LOOP ( 'NONE', ( #20855, #38822, #24971, #23511 ) ) ;
#15143 = CARTESIAN_POINT ( 'NONE',  ( -16.45614608779968080, 0.000000000000000000, 3.415019368575790804 ) ) ;
#15144 = DIRECTION ( 'NONE',  ( 0.005002170337468016433, -0.7660444431189770143, -0.6427681459581293666 ) ) ;
#15145 = DIRECTION ( 'NONE',  ( -0.9999697198139514409, -0.000000000000000000, -0.007781995580013368816 ) ) ;
#15146 = ORIENTED_EDGE ( 'NONE', *, *, #52752, .F. ) ;
#15147 = DIRECTION ( 'NONE',  ( -0.9999697198139514409, -0.000000000000000000, -0.007781995580013368816 ) ) ;
#15148 = ORIENTED_EDGE ( 'NONE', *, *, #53108, .T. ) ;
#15149 = VECTOR ( 'NONE', #39801, 999.9999999999998863 ) ;
#15150 = VERTEX_POINT ( 'NONE', #44443 ) ;
#15151 = ORIENTED_EDGE ( 'NONE', *, *, #27912, .T. ) ;
#15152 = CARTESIAN_POINT ( 'NONE',  ( -19.43036298310061483, 2.391131607591507446, 8.352988289389880805 ) ) ;
#15153 = ORIENTED_EDGE ( 'NONE', *, *, #13229, .F. ) ;
#15154 = DIRECTION ( 'NONE',  ( -0.5449076811759708816, 0.6444004775717707689, 0.5364919789714475140 ) ) ;
#15155 = ORIENTED_EDGE ( 'NONE', *, *, #7068, .F. ) ;
#15156 = LINE ( 'NONE', #23929, #28563 ) ;
#15157 = DIRECTION ( 'NONE',  ( 0.005002170337468016433, -0.7660444431189770143, -0.6427681459581293666 ) ) ;
#15158 = EDGE_CURVE ( 'NONE', #1353, #40267, #40187, .T. ) ;
#15159 = EDGE_CURVE ( 'NONE', #50596, #33190, #8986, .T. ) ;
#15160 = VERTEX_POINT ( 'NONE', #45029 ) ;
#15161 = VECTOR ( 'NONE', #29990, 1000.000000000000227 ) ;
#15162 = CARTESIAN_POINT ( 'NONE',  ( -10.94028622754223967, 0.000000000000000000, 11.14038480894692995 ) ) ;
#15163 = ORIENTED_EDGE ( 'NONE', *, *, #38819, .F. ) ;
#15164 = ADVANCED_FACE ( 'NONE', ( #32521 ), #45547, .F. ) ;
#15165 = AXIS2_PLACEMENT_3D ( 'NONE', #28217, #49546, #49808 ) ;
#15166 = DIRECTION ( 'NONE',  ( 0.005961354470445682716, -0.6427876096865404731, -0.7660212471507180654 ) ) ;
#15167 = DIRECTION ( 'NONE',  ( 0.007781995580012663651, 0.000000000000000000, -0.9999697198139515519 ) ) ;
#15168 = CARTESIAN_POINT ( 'NONE',  ( -12.70113610826450845, 4.333955019861509328, 8.927632253102496307 ) ) ;
#15169 = CARTESIAN_POINT ( 'NONE',  ( -18.67775241435682432, 0.000000000000000000, 4.136394454059623804 ) ) ;
#15170 = CARTESIAN_POINT ( 'NONE',  ( -12.30028049777745558, 0.000000000000000000, 6.771349903807757364 ) ) ;
#15171 = LINE ( 'NONE', #22063, #24622 ) ;
#15172 = CARTESIAN_POINT ( 'NONE',  ( -21.47263955680318404, 0.000000000000000000, 5.022634149262071190 ) ) ;
#15173 = ORIENTED_EDGE ( 'NONE', *, *, #48624, .F. ) ;
#15174 = VERTEX_POINT ( 'NONE', #41016 ) ;
#15175 = VECTOR ( 'NONE', #28276, 1000.000000000000114 ) ;
#15176 = CARTESIAN_POINT ( 'NONE',  ( -11.67244013076689946, 0.000000000000000000, 11.50401908778467863 ) ) ;
#15177 = FACE_OUTER_BOUND ( 'NONE', #14631, .T. ) ;
#15178 = CARTESIAN_POINT ( 'NONE',  ( -10.70637586329141122, 0.000000000000000000, 6.783754038227788108 ) ) ;
#15179 = DIRECTION ( 'NONE',  ( -0.5364919789714478471, 0.6444004775717705469, -0.5449076811759709926 ) ) ;
#15180 = LINE ( 'NONE', #53499, #19484 ) ;
#15181 = VERTEX_POINT ( 'NONE', #28237 ) ;
#15182 = FACE_OUTER_BOUND ( 'NONE', #32262, .T. ) ;
#15183 = DIRECTION ( 'NONE',  ( 0.007781995580012662783, 0.000000000000000000, -0.9999697198139514409 ) ) ;
#15184 = ORIENTED_EDGE ( 'NONE', *, *, #24070, .F. ) ;
#15185 = CARTESIAN_POINT ( 'NONE',  ( -15.13495153988577968, 0.000000000000000000, 12.76973526769478084 ) ) ;
#15186 = CARTESIAN_POINT ( 'NONE',  ( -26.84049344369173085, 17.16190973098311900, -4.646098577050644884 ) ) ;
#15187 = VERTEX_POINT ( 'NONE', #1826 ) ;
#15188 = CARTESIAN_POINT ( 'NONE',  ( -18.61801697800028066, 0.000000000000000000, 8.368838110497661020 ) ) ;
#15189 = CARTESIAN_POINT ( 'NONE',  ( -15.60102546347950536, 0.000000000000000000, 12.95077420755565356 ) ) ;
#15190 = DIRECTION ( 'NONE',  ( 0.6427681459581294776, -0.7660444431189769032, 0.005002170337467562802 ) ) ;
#15191 = EDGE_CURVE ( 'NONE', #37975, #2305, #19439, .T. ) ;
#15192 = PLANE ( 'NONE',  #54086 ) ;
#15193 = DIRECTION ( 'NONE',  ( -0.5449076811759708816, 0.6444004775717707689, 0.5364919789714475140 ) ) ;
#15194 = ORIENTED_EDGE ( 'NONE', *, *, #30670, .F. ) ;
#15195 = ADVANCED_FACE ( 'NONE', ( #19151 ), #54097, .F. ) ;
#15196 = VERTEX_POINT ( 'NONE', #53524 ) ;
#15197 = LINE ( 'NONE', #49557, #51147 ) ;
#15198 = LINE ( 'NONE', #23434, #24946 ) ;
#15199 = CARTESIAN_POINT ( 'NONE',  ( -15.85841441797052731, -2.298917212465658721, 2.967920335911165886 ) ) ;
#15200 = EDGE_CURVE ( 'NONE', #51439, #12052, #18618, .T. ) ;
#15201 = DIRECTION ( 'NONE',  ( 0.5449076811759707706, 0.6444004775717708799, -0.5364919789714476250 ) ) ;
#15202 = EDGE_CURVE ( 'NONE', #6270, #12635, #15206, .T. ) ;
#15203 = LINE ( 'NONE', #37055, #15836 ) ;
#15204 = VERTEX_POINT ( 'NONE', #53799 ) ;
#15205 = CARTESIAN_POINT ( 'NONE',  ( -14.41904058539880751, 0.000000000000000000, 6.185523096863160042 ) ) ;
#15207 = VECTOR ( 'NONE', #33136, 999.9999999999998863 ) ;
#15206 = LINE ( 'NONE', #6969, #48626 ) ;
#15208 = FACE_OUTER_BOUND ( 'NONE', #9470, .T. ) ;
#15209 = VERTEX_POINT ( 'NONE', #53279 ) ;
#15210 = DIRECTION ( 'NONE',  ( -0.5364919789714478471, 0.6444004775717705469, -0.5449076811759709926 ) ) ;
#15211 = DIRECTION ( 'NONE',  ( -0.7660212471507179544, -0.6427876096865405842, -0.005961354470445141482 ) ) ;
#15212 = FACE_OUTER_BOUND ( 'NONE', #11583, .T. ) ;
#15213 = ORIENTED_EDGE ( 'NONE', *, *, #29841, .F. ) ;
#15214 = VECTOR ( 'NONE', #48465, 999.9999999999998863 ) ;
#15215 = LINE ( 'NONE', #32529, #5077 ) ;
#15216 = ORIENTED_EDGE ( 'NONE', *, *, #16007, .F. ) ;
#15217 = ORIENTED_EDGE ( 'NONE', *, *, #1015, .F. ) ;
#15218 = VERTEX_POINT ( 'NONE', #32245 ) ;
#15219 = FACE_OUTER_BOUND ( 'NONE', #13872, .T. ) ;
#15220 = ORIENTED_EDGE ( 'NONE', *, *, #55262, .T. ) ;
#15221 = ORIENTED_EDGE ( 'NONE', *, *, #7986, .T. ) ;
#15222 = DIRECTION ( 'NONE',  ( 0.5364919789714477361, 0.6444004775717706579, 0.5449076811759711036 ) ) ;
#15223 = EDGE_LOOP ( 'NONE', ( #22179, #33695, #23316, #41400 ) ) ;
#15224 = ADVANCED_FACE ( 'NONE', ( #14913 ), #23981, .F. ) ;
#15225 = ORIENTED_EDGE ( 'NONE', *, *, #40811, .F. ) ;
#15226 = CARTESIAN_POINT ( 'NONE',  ( -22.40634380310664397, 0.000000000000000000, 5.584705972946605534 ) ) ;
#15227 = ORIENTED_EDGE ( 'NONE', *, *, #34209, .F. ) ;
#15228 = ORIENTED_EDGE ( 'NONE', *, *, #51527, .T. ) ;
#15229 = ADVANCED_FACE ( 'NONE', ( #50084 ), #49567, .F. ) ;
#15230 = ADVANCED_FACE ( 'NONE', ( #11195 ), #49824, .F. ) ;
#15231 = ORIENTED_EDGE ( 'NONE', *, *, #24483, .T. ) ;
#15232 = LINE ( 'NONE', #54962, #2960 ) ;
#15233 = DIRECTION ( 'NONE',  ( 0.6427681459581294776, -0.7660444431189769032, 0.005002170337467562802 ) ) ;
#15234 = FACE_OUTER_BOUND ( 'NONE', #4852, .T. ) ;
#15235 = LINE ( 'NONE', #24555, #5081 ) ;
#15236 = ORIENTED_EDGE ( 'NONE', *, *, #9372, .T. ) ;
#15237 = DIRECTION ( 'NONE',  ( -0.1139275668495183386, 0.9934890585767658377, 4.694855797473113547E-16 ) ) ;
#15238 = ORIENTED_EDGE ( 'NONE', *, *, #21385, .F. ) ;
#15239 = ORIENTED_EDGE ( 'NONE', *, *, #54873, .T. ) ;
#15240 = FACE_OUTER_BOUND ( 'NONE', #10644, .T. ) ;
#15241 = EDGE_CURVE ( 'NONE', #13117, #56078, #27401, .T. ) ;
#15242 = CARTESIAN_POINT ( 'NONE',  ( -29.11308221448052080, 15.84982999241088919, -4.729108557267000634 ) ) ;
#15243 = LINE ( 'NONE', #40538, #3136 ) ;
#15244 = DIRECTION ( 'NONE',  ( 0.007781995580012663651, 0.000000000000000000, -0.9999697198139515519 ) ) ;
#15245 = CARTESIAN_POINT ( 'NONE',  ( -13.63328395545196159, 4.333955019861509328, 9.289710132824241740 ) ) ;
#15246 = EDGE_LOOP ( 'NONE', ( #36455, #47686, #15817, #49005 ) ) ;
#15247 = DIRECTION ( 'NONE',  ( 0.7660212471507180654, -0.6427876096865404731, 0.005961354470445141482 ) ) ;
#15248 = ORIENTED_EDGE ( 'NONE', *, *, #31142, .F. ) ;
#15249 = VECTOR ( 'NONE', #20808, 999.9999999999998863 ) ;
#15250 = FACE_OUTER_BOUND ( 'NONE', #38258, .T. ) ;
#15251 = DIRECTION ( 'NONE',  ( 0.5364919789714477361, 0.6444004775717706579, 0.5449076811759711036 ) ) ;
#15252 = CARTESIAN_POINT ( 'NONE',  ( -9.952547186413761793, 0.000000000000000000, 3.634957892622900033 ) ) ;
#15253 = DIRECTION ( 'NONE',  ( 0.005961354470445682716, -0.6427876096865404731, -0.7660212471507180654 ) ) ;
#15254 = CARTESIAN_POINT ( 'NONE',  ( -15.25611291248567980, -2.137015261443160341, 2.739131496823017375 ) ) ;
#15255 = VERTEX_POINT ( 'NONE', #19731 ) ;
#15256 = CARTESIAN_POINT ( 'NONE',  ( -50.99228148001754590, 2.341865487272625668, 2.999999999999993339 ) ) ;
#15257 = DIRECTION ( 'NONE',  ( 0.9999697198139515519, 0.000000000000000000, 0.007781995580013368816 ) ) ;
#15258 = FACE_OUTER_BOUND ( 'NONE', #45696, .T. ) ;
#15259 = CARTESIAN_POINT ( 'NONE',  ( -69.99028037491666510, 0.2761374490229266399, -7.501514206501484594 ) ) ;
#15260 = ADVANCED_FACE ( 'NONE', ( #40760 ), #44722, .F. ) ;
#15261 = DIRECTION ( 'NONE',  ( 0.000000000000000000, -1.000000000000000000, 0.000000000000000000 ) ) ;
#15262 = CARTESIAN_POINT ( 'NONE',  ( -9.442067484779661513, -0.1191753592594197858, 10.59804618892231254 ) ) ;
#15263 = CARTESIAN_POINT ( 'NONE',  ( -14.46888367232926420, 0.000000000000000000, 12.59025272694991315 ) ) ;
#15264 = FACE_OUTER_BOUND ( 'NONE', #21369, .T. ) ;
#15265 = CARTESIAN_POINT ( 'NONE',  ( -20.19048558356006495, 0.000000000000000000, 5.601950293978301687 ) ) ;
#15266 = EDGE_CURVE ( 'NONE', #33543, #27412, #15452, .T. ) ;
#15267 = ORIENTED_EDGE ( 'NONE', *, *, #5344, .F. ) ;
#15268 = EDGE_CURVE ( 'NONE', #51780, #2633, #28519, .T. ) ;
#15269 = EDGE_CURVE ( 'NONE', #44507, #48671, #18908, .T. ) ;
#15270 = ORIENTED_EDGE ( 'NONE', *, *, #33779, .F. ) ;
#15271 = ORIENTED_EDGE ( 'NONE', *, *, #50850, .F. ) ;
#15272 = ORIENTED_EDGE ( 'NONE', *, *, #40795, .F. ) ;
#15273 = ORIENTED_EDGE ( 'NONE', *, *, #3482, .T. ) ;
#15274 = CARTESIAN_POINT ( 'NONE',  ( -20.67682646184930206, -3.594132820645662196, 4.798231048616345085 ) ) ;
#15275 = EDGE_CURVE ( 'NONE', #13570, #36235, #31948, .T. ) ;
#15276 = CARTESIAN_POINT ( 'NONE',  ( -1.753914626039396296, 5.922546351860411562, 3.899653579608918896 ) ) ;
#15277 = AXIS2_PLACEMENT_3D ( 'NONE', #34255, #21164, #51562 ) ;
#15279 = EDGE_CURVE ( 'NONE', #12863, #17764, #28820, .T. ) ;
#15278 = ORIENTED_EDGE ( 'NONE', *, *, #1371, .T. ) ;
#15280 = DIRECTION ( 'NONE',  ( 0.005961354470445682716, -0.6427876096865404731, -0.7660212471507180654 ) ) ;
#15281 = ORIENTED_EDGE ( 'NONE', *, *, #11607, .T. ) ;
#15282 = ORIENTED_EDGE ( 'NONE', *, *, #7716, .T. ) ;
#15283 = ADVANCED_FACE ( 'NONE', ( #38155 ), #46681, .F. ) ;
#15284 = CARTESIAN_POINT ( 'NONE',  ( -67.76121356559087872, -9.465062053996337710, 8.159882300530348687 ) ) ;
#15285 = CARTESIAN_POINT ( 'NONE',  ( -8.443718568120347712, 8.231294610302708037, 6.498200617411320934 ) ) ;
#15286 = LINE ( 'NONE', #11003, #16874 ) ;
#15287 = VERTEX_POINT ( 'NONE', #11499 ) ;
#15288 = CARTESIAN_POINT ( 'NONE',  ( -20.52784467904771759, 0.000000000000000000, 14.94375894514125491 ) ) ;
#15289 = EDGE_CURVE ( 'NONE', #8713, #44261, #24528, .T. ) ;
#15290 = DIRECTION ( 'NONE',  ( -0.7660212471507179544, -0.6427876096865405842, -0.005961354470445141482 ) ) ;
#15291 = LINE ( 'NONE', #53895, #42945 ) ;
#15292 = EDGE_CURVE ( 'NONE', #54772, #43897, #2667, .T. ) ;
#15293 = DIRECTION ( 'NONE',  ( 0.007781995580012663651, 0.000000000000000000, -0.9999697198139515519 ) ) ;
#15294 = DIRECTION ( 'NONE',  ( -0.5364919789714478471, 0.6444004775717705469, -0.5449076811759709926 ) ) ;
#15295 = CARTESIAN_POINT ( 'NONE',  ( -24.57312748012714820, 18.34675972927921350, -4.549864808573585329 ) ) ;
#15296 = DIRECTION ( 'NONE',  ( -0.7660212471507179544, -0.6427876096865405842, -0.005961354470445141482 ) ) ;
#15297 = PLANE ( 'NONE',  #42052 ) ;
#15298 = DIRECTION ( 'NONE',  ( -0.5449076811759708816, 0.6444004775717707689, 0.5364919789714475140 ) ) ;
#15299 = ORIENTED_EDGE ( 'NONE', *, *, #20054, .T. ) ;
#15300 = FACE_OUTER_BOUND ( 'NONE', #54624, .T. ) ;
#15301 = ORIENTED_EDGE ( 'NONE', *, *, #16576, .F. ) ;
#15302 = CARTESIAN_POINT ( 'NONE',  ( 1.086233639165236964, 0.000000000000000000, 2.796443541562362078 ) ) ;
#15303 = CARTESIAN_POINT ( 'NONE',  ( -16.39848171883952332, -0.1191753592594198830, 8.855446145018868620 ) ) ;
#15304 = PLANE ( 'NONE',  #29499 ) ;
#15305 = DIRECTION ( 'NONE',  ( 0.005002170337468016433, -0.7660444431189770143, -0.6427681459581293666 ) ) ;
#15306 = CARTESIAN_POINT ( 'NONE',  ( -26.13337879274045505, 0.000000000000000000, 6.833023547870798353 ) ) ;
#15307 = CARTESIAN_POINT ( 'NONE',  ( -15.83019559695375911, 0.000000000000000000, 8.390533581105717786 ) ) ;
#15308 = DIRECTION ( 'NONE',  ( 0.005002170337468016433, -0.7660444431189770143, -0.6427681459581293666 ) ) ;
#15309 =( NAMED_UNIT ( * ) SI_UNIT ( $, .STERADIAN. ) SOLID_ANGLE_UNIT ( ) );
#15310 = DIRECTION ( 'NONE',  ( 0.007781995580012663651, -3.146120232559066537E-19, -0.9999697198139514409 ) ) ;
#15311 = CARTESIAN_POINT ( 'NONE',  ( -64.10539783498545319, 7.375519243179410545, -3.000000000000000000 ) ) ;
#15312 = CARTESIAN_POINT ( 'NONE',  ( -20.54049170961573267, 0.000000000000000000, 4.660556269540326646 ) ) ;
#15313 = CARTESIAN_POINT ( 'NONE',  ( -20.42542555003737093, -0.2049780936125319142, 5.058787616018051381 ) ) ;
#15314 = LINE ( 'NONE', #45678, #54077 ) ;
#15315 = AXIS2_PLACEMENT_3D ( 'NONE', #14816, #22513, #44082 ) ;
#15316 = FACE_OUTER_BOUND ( 'NONE', #43747, .T. ) ;
#15317 = ADVANCED_FACE ( 'NONE', ( #20835 ), #55204, .F. ) ;
#15318 = PLANE ( 'NONE',  #27564 ) ;
#15319 = DIRECTION ( 'NONE',  ( 0.000000000000000000, -1.000000000000000000, 0.000000000000000000 ) ) ;
#15320 = LINE ( 'NONE', #53646, #45586 ) ;
#15321 = VERTEX_POINT ( 'NONE', #29678 ) ;
#15322 = DIRECTION ( 'NONE',  ( 0.007781995580012662783, 0.000000000000000000, -0.9999697198139514409 ) ) ;
#15323 = EDGE_LOOP ( 'NONE', ( #46477, #33424, #34494 ) ) ;
#15324 = PLANE ( 'NONE',  #5096 ) ;
#15325 = CARTESIAN_POINT ( 'NONE',  ( -14.17413731849972613, 0.000000000000000000, 8.724089865898580598 ) ) ;
#15326 = VERTEX_POINT ( 'NONE', #25127 ) ;
#15327 = CARTESIAN_POINT ( 'NONE',  ( -18.28310086152664127, -0.1941918491731536578, 4.102410910690207579 ) ) ;
#15328 = ORIENTED_EDGE ( 'NONE', *, *, #51503, .F. ) ;
#15329 = DIRECTION ( 'NONE',  ( -1.000000000000000000, 0.000000000000000000, -0.000000000000000000 ) ) ;
#15330 = EDGE_CURVE ( 'NONE', #10233, #24902, #16038, .T. ) ;
#15331 = ORIENTED_EDGE ( 'NONE', *, *, #3822, .F. ) ;
#15332 = EDGE_LOOP ( 'NONE', ( #42274, #50101, #22133, #39367 ) ) ;
#15333 = ORIENTED_EDGE ( 'NONE', *, *, #16068, .T. ) ;
#15334 = FACE_OUTER_BOUND ( 'NONE', #28828, .T. ) ;
#15335 = CARTESIAN_POINT ( 'NONE',  ( -12.23851102634202448, -0.1191753592594197858, 11.68427982808754884 ) ) ;
#15336 = DIRECTION ( 'NONE',  ( 0.005961354470445682716, -0.6427876096865404731, -0.7660212471507180654 ) ) ;
#15337 = EDGE_CURVE ( 'NONE', #33548, #33876, #20576, .T. ) ;
#15338 = VERTEX_POINT ( 'NONE', #41841 ) ;
#15339 = ORIENTED_EDGE ( 'NONE', *, *, #33475, .F. ) ;
#15340 = EDGE_CURVE ( 'NONE', #30955, #40959, #29075, .T. ) ;
#15341 = FACE_OUTER_BOUND ( 'NONE', #10058, .T. ) ;
#15342 = ORIENTED_EDGE ( 'NONE', *, *, #20590, .F. ) ;
#15343 = CARTESIAN_POINT ( 'NONE',  ( -15.62609718784551838, 0.1245042932765041271, 2.747666204937259771 ) ) ;
#15344 = ORIENTED_EDGE ( 'NONE', *, *, #4103, .F. ) ;
#15345 = CARTESIAN_POINT ( 'NONE',  ( -18.39611916365119271, 3.362543313726509719, 9.545504970550553026 ) ) ;
#15346 = LINE ( 'NONE', #33248, #16756 ) ;
#15347 = ADVANCED_FACE ( 'NONE', ( #25385 ), #2939, .F. ) ;
#15348 = AXIS2_PLACEMENT_3D ( 'NONE', #11099, #11673, #49987 ) ;
#15349 = ORIENTED_EDGE ( 'NONE', *, *, #53064, .F. ) ;
#15350 = CARTESIAN_POINT ( 'NONE',  ( -15.36555870011267366, 0.000000000000000000, 8.394149492873728136 ) ) ;
#15351 = EDGE_CURVE ( 'NONE', #49806, #29206, #42140, .T. ) ;
#15352 = CARTESIAN_POINT ( 'NONE',  ( -18.72630217577924583, -0.1191753592594160666, 9.433079126556494387 ) ) ;
#15353 = ORIENTED_EDGE ( 'NONE', *, *, #37623, .F. ) ;
#15354 = DIRECTION ( 'NONE',  ( 0.000000000000000000, -1.000000000000000000, 0.000000000000000000 ) ) ;
#15355 = CARTESIAN_POINT ( 'NONE',  ( -16.81345671998191449, 0.000000000000000000, 3.412238694616132495 ) ) ;
#15356 = ORIENTED_EDGE ( 'NONE', *, *, #42390, .F. ) ;
#15357 = DIRECTION ( 'NONE',  ( -0.5449076811759708816, 0.6444004775717707689, 0.5364919789714475140 ) ) ;
#15358 = LINE ( 'NONE', #49155, #16037 ) ;
#15359 = DIRECTION ( 'NONE',  ( -0.9321478471874540261, 0.000000000000000000, 0.3620778797217457656 ) ) ;
#15360 = DIRECTION ( 'NONE',  ( -0.6427681459581293666, -0.7660444431189770143, -0.005002170337467561935 ) ) ;
#15361 = DIRECTION ( 'NONE',  ( 0.9999697198139515519, 0.000000000000000000, 0.007781995580013368816 ) ) ;
#15362 = CARTESIAN_POINT ( 'NONE',  ( -28.92982233430281980, 0.000000000000000000, 7.919257187036034651 ) ) ;
#15363 = FACE_OUTER_BOUND ( 'NONE', #46248, .T. ) ;
#15364 = VERTEX_POINT ( 'NONE', #46380 ) ;
#15365 = PLANE ( 'NONE',  #27116 ) ;
#15366 = CARTESIAN_POINT ( 'NONE',  ( -21.47263955680318404, 0.000000000000000000, 5.022634149262071190 ) ) ;
#15367 = CARTESIAN_POINT ( 'NONE',  ( -68.75638519912476454, -2.100476156393307137E-11, -7.380886937888696764 ) ) ;
#15368 = ORIENTED_EDGE ( 'NONE', *, *, #54714, .F. ) ;
#15369 = DIRECTION ( 'NONE',  ( -0.005002170337468016433, -0.7660444431189770143, 0.6427681459581293666 ) ) ;
#15370 = FACE_OUTER_BOUND ( 'NONE', #11600, .T. ) ;
#15371 = DIRECTION ( 'NONE',  ( 0.5000000000000011102, -0.8660254037844380415, 0.000000000000000000 ) ) ;
#15372 = EDGE_CURVE ( 'NONE', #41034, #19170, #54620, .T. ) ;
#15373 = PLANE ( 'NONE',  #29665 ) ;
#15374 = CARTESIAN_POINT ( 'NONE',  ( -13.20345603875051665, 5.467268677019013090, 10.98271116061314956 ) ) ;
#15375 = ORIENTED_EDGE ( 'NONE', *, *, #7002, .T. ) ;
#15376 = EDGE_CURVE ( 'NONE', #32426, #41467, #33613, .T. ) ;
#15377 = ORIENTED_EDGE ( 'NONE', *, *, #17837, .F. ) ;
#15378 = EDGE_CURVE ( 'NONE', #45628, #98, #42433, .T. ) ;
#15379 = CARTESIAN_POINT ( 'NONE',  ( -21.47419595591918906, 0.000000000000000000, 5.222628093224860102 ) ) ;
#15380 = EDGE_CURVE ( 'NONE', #17338, #34543, #3789, .T. ) ;
#15381 = EDGE_CURVE ( 'NONE', #44617, #54969, #50389, .T. ) ;
#15382 = ADVANCED_FACE ( 'NONE', ( #19333 ), #15618, .F. ) ;
#15383 = CARTESIAN_POINT ( 'NONE',  ( 2.072287782118878319, 0.000000000000000000, -2.950529333540147015 ) ) ;
#15384 = VERTEX_POINT ( 'NONE', #28718 ) ;
#15385 = FACE_OUTER_BOUND ( 'NONE', #29354, .T. ) ;
#15386 = ORIENTED_EDGE ( 'NONE', *, *, #50894, .F. ) ;
#15387 = LINE ( 'NONE', #40943, #2926 ) ;
#15388 = VERTEX_POINT ( 'NONE', #2830 ) ;
#15389 = ORIENTED_EDGE ( 'NONE', *, *, #17009, .F. ) ;
#15390 = CARTESIAN_POINT ( 'NONE',  ( -9.941050972392631024, 0.000000000000000000, 2.157719079591843059 ) ) ;
#15391 = FACE_OUTER_BOUND ( 'NONE', #49064, .T. ) ;
#15392 = DIRECTION ( 'NONE',  ( 0.9999697198139515519, 0.000000000000000000, 0.007781995580013368816 ) ) ;
#15393 = ORIENTED_EDGE ( 'NONE', *, *, #52441, .F. ) ;
#15394 = CARTESIAN_POINT ( 'NONE',  ( -13.22955429145962469, 0.000000000000000000, 6.764118080271738442 ) ) ;
#15395 = ADVANCED_FACE ( 'NONE', ( #11089 ), #36671, .F. ) ;
#15396 = ORIENTED_EDGE ( 'NONE', *, *, #30363, .T. ) ;
#15398 = ORIENTED_EDGE ( 'NONE', *, *, #5228, .F. ) ;
#15397 = ADVANCED_FACE ( 'NONE', ( #53431 ), #19633, .F. ) ;
#15399 = ORIENTED_EDGE ( 'NONE', *, *, #32306, .T. ) ;
#15400 = DIRECTION ( 'NONE',  ( 0.5449076811759707706, 0.6444004775717708799, -0.5364919789714476250 ) ) ;
#15401 = EDGE_CURVE ( 'NONE', #45158, #54577, #14527, .T. ) ;
#15402 = EDGE_LOOP ( 'NONE', ( #4663, #34833, #13218, #46300 ) ) ;
#15403 = DIRECTION ( 'NONE',  ( 0.000000000000000000, -0.000000000000000000, -1.000000000000000000 ) ) ;
#15404 = EDGE_LOOP ( 'NONE', ( #5101, #4318, #50292, #42505 ) ) ;
#15405 = CARTESIAN_POINT ( 'NONE',  ( -19.32961685222932147, 0.000000000000000000, 14.39908572644263351 ) ) ;
#15406 = DIRECTION ( 'NONE',  ( 0.000000000000000000, 0.000000000000000000, 1.000000000000000000 ) ) ;
#15407 = ADVANCED_FACE ( 'NONE', ( #40915 ), #1996, .F. ) ;
#15408 = ORIENTED_EDGE ( 'NONE', *, *, #13346, .T. ) ;
#15409 = DIRECTION ( 'NONE',  ( 0.000000000000000000, -0.000000000000000000, -1.000000000000000000 ) ) ;
#15410 = VERTEX_POINT ( 'NONE', #54265 ) ;
#15411 = VECTOR ( 'NONE', #44198, 999.9999999999998863 ) ;
#15412 = CARTESIAN_POINT ( 'NONE',  ( -23.33771345073609638, -0.1191753592594197858, 5.846786880686956955 ) ) ;
#15413 = CARTESIAN_POINT ( 'NONE',  ( -19.60912206198628027, -0.1191753592594197858, 4.398475361799976113 ) ) ;
#15414 = DIRECTION ( 'NONE',  ( -0.6427681459581293666, -0.7660444431189770143, -0.005002170337467561935 ) ) ;
#15415 = FACE_OUTER_BOUND ( 'NONE', #41105, .T. ) ;
#15416 = CARTESIAN_POINT ( 'NONE',  ( -18.67775241435682432, 0.000000000000000000, 4.136394454059623804 ) ) ;
#15417 = LINE ( 'NONE', #37022, #4758 ) ;
#15418 = ORIENTED_EDGE ( 'NONE', *, *, #8767, .T. ) ;
#15419 = ORIENTED_EDGE ( 'NONE', *, *, #51725, .F. ) ;
#15420 = DIRECTION ( 'NONE',  ( -0.7660212471507179544, -0.6427876096865405842, -0.005961354470445141482 ) ) ;
#15421 = DIRECTION ( 'NONE',  ( -0.7660212471507179544, -0.6427876096865405842, -0.005961354470445141482 ) ) ;
#15422 = LINE ( 'NONE', #37280, #47544 ) ;
#15423 = FACE_OUTER_BOUND ( 'NONE', #5851, .T. ) ;
#15424 = DIRECTION ( 'NONE',  ( 0.007781995580012662783, 0.000000000000000000, -0.9999697198139514409 ) ) ;
#15425 = ORIENTED_EDGE ( 'NONE', *, *, #18551, .T. ) ;
#15426 = CARTESIAN_POINT ( 'NONE',  ( -16.43317633868556626, -0.1191753592594197858, 13.31363028683540151 ) ) ;
#15427 = DIRECTION ( 'NONE',  ( 0.000000000000000000, -0.000000000000000000, -1.000000000000000000 ) ) ;
#15428 = VERTEX_POINT ( 'NONE', #7134 ) ;
#15429 = DIRECTION ( 'NONE',  ( -0.6427681459581293666, -0.7660444431189770143, -0.005002170337467561935 ) ) ;
#15430 = CARTESIAN_POINT ( 'NONE',  ( -22.40634380310664397, 0.000000000000000000, 5.584705972946605534 ) ) ;
#15431 = EDGE_LOOP ( 'NONE', ( #13787, #49812, #41003, #17341 ) ) ;
#15432 = FACE_OUTER_BOUND ( 'NONE', #36267, .T. ) ;
#15433 = LINE ( 'NONE', #3223, #24232 ) ;
#15434 = CARTESIAN_POINT ( 'NONE',  ( -26.13493519185646008, 0.000000000000000000, 7.033017491833586377 ) ) ;
#15435 = PLANE ( 'NONE',  #23286 ) ;
#15436 = DIRECTION ( 'NONE',  ( 0.007781995580012663651, 0.000000000000000000, -0.9999697198139515519 ) ) ;
#15437 = ORIENTED_EDGE ( 'NONE', *, *, #28594, .T. ) ;
#15438 = EDGE_CURVE ( 'NONE', #3168, #55625, #10827, .T. ) ;
#15439 = ORIENTED_EDGE ( 'NONE', *, *, #43049, .F. ) ;
#15440 = LINE ( 'NONE', #23969, #52044 ) ;
#15441 = FACE_OUTER_BOUND ( 'NONE', #48811, .T. ) ;
#15442 = LINE ( 'NONE', #32765, #32349 ) ;
#15443 = EDGE_CURVE ( 'NONE', #9714, #1292, #24430, .T. ) ;
#15444 = ADVANCED_FACE ( 'NONE', ( #6031 ), #6560, .F. ) ;
#15445 = CARTESIAN_POINT ( 'NONE',  ( -13.61720543878437439, -0.1191753592594146788, 8.507758610330894200 ) ) ;
#15446 = CARTESIAN_POINT ( 'NONE',  ( -21.47693870893288093, 3.200641362704010007, 4.922186869281591548 ) ) ;
#15447 = LINE ( 'NONE', #28515, #27655 ) ;
#15449 = EDGE_CURVE ( 'NONE', #18021, #25146, #14807, .T. ) ;
#15448 = EDGE_LOOP ( 'NONE', ( #15225, #14490, #18398 ) ) ;
#15450 = DIRECTION ( 'NONE',  ( -0.005961354470445682716, -0.6427876096865404731, 0.7660212471507180654 ) ) ;
#15451 = VECTOR ( 'NONE', #51282, 1000.000000000000227 ) ;
#15452 = LINE ( 'NONE', #32773, #25077 ) ;
#15453 = CARTESIAN_POINT ( 'NONE',  ( -19.99180929398655593, 0.000000000000000000, 5.772822452389281267 ) ) ;
#15454 = ORIENTED_EDGE ( 'NONE', *, *, #31695, .F. ) ;
#15455 = CARTESIAN_POINT ( 'NONE',  ( -14.40136551438387436, -1.651309408375657428, 4.985991233126853217 ) ) ;
#15456 = CARTESIAN_POINT ( 'NONE',  ( -14.87086361382948141, 0.000000000000000000, 4.535352612769118608 ) ) ;
#15457 = DIRECTION ( 'NONE',  ( -0.5364919789714478471, 0.6444004775717705469, -0.5449076811759709926 ) ) ;
#15458 = ORIENTED_EDGE ( 'NONE', *, *, #2792, .T. ) ;
#15459 = CARTESIAN_POINT ( 'NONE',  ( -18.67775241435682432, 0.000000000000000000, 4.136394454059623804 ) ) ;
#15460 = VERTEX_POINT ( 'NONE', #31843 ) ;
#15461 = EDGE_CURVE ( 'NONE', #17816, #19391, #15358, .T. ) ;
#15462 = ORIENTED_EDGE ( 'NONE', *, *, #8653, .T. ) ;
#15463 = EDGE_LOOP ( 'NONE', ( #13953, #13330, #36458, #30076 ) ) ;
#15464 = ORIENTED_EDGE ( 'NONE', *, *, #2520, .F. ) ;
#15465 = EDGE_CURVE ( 'NONE', #27011, #36001, #1734, .T. ) ;
#15466 = EDGE_LOOP ( 'NONE', ( #3438, #48031, #35825, #39855 ) ) ;
#15467 = DIRECTION ( 'NONE',  ( 0.007781995580012663651, -3.146120232559066537E-19, -0.9999697198139514409 ) ) ;
#15468 = ORIENTED_EDGE ( 'NONE', *, *, #44825, .T. ) ;
#15469 = ADVANCED_FACE ( 'NONE', ( #49978 ), #45728, .F. ) ;
#15470 = VERTEX_POINT ( 'NONE', #36379 ) ;
#15471 = CARTESIAN_POINT ( 'NONE',  ( -26.25138199253913385, 17.50203338588876179, 4.621929860192643069 ) ) ;
#15472 = EDGE_LOOP ( 'NONE', ( #18736, #46857, #28168, #12973 ) ) ;
#15473 = ORIENTED_EDGE ( 'NONE', *, *, #27573, .T. ) ;
#15474 = EDGE_CURVE ( 'NONE', #883, #45963, #23872, .T. ) ;
#15475 = ORIENTED_EDGE ( 'NONE', *, *, #34804, .F. ) ;
#15476 = CARTESIAN_POINT ( 'NONE',  ( -19.22540549493500350, 3.848249166794009302, 4.026952827025455761 ) ) ;
#15477 = LINE ( 'NONE', #55796, #11271 ) ;
#15478 = LINE ( 'NONE', #19759, #26888 ) ;
#15479 = DIRECTION ( 'NONE',  ( 0.9999697198139515519, 0.000000000000000000, 0.007781995580013368816 ) ) ;
#15480 = ORIENTED_EDGE ( 'NONE', *, *, #53130, .F. ) ;
#15481 = CARTESIAN_POINT ( 'NONE',  ( -18.25415525269858463, -0.1191753592594158168, 8.471672794689057540 ) ) ;
#15482 = VERTEX_POINT ( 'NONE', #45195 ) ;
#15483 = ORIENTED_EDGE ( 'NONE', *, *, #47711, .F. ) ;
#15484 = CIRCLE ( 'NONE', #38148, 3.692809041582069352 ) ;
#15485 = LINE ( 'NONE', #3286, #23075 ) ;
#15486 = CARTESIAN_POINT ( 'NONE',  ( -9.908141408373387193, -0.1191753592594197858, 10.77908512878318703 ) ) ;
#15487 = UNCERTAINTY_MEASURE_WITH_UNIT (LENGTH_MEASURE( 1.000000000000000082E-05 ), #40020, 'distance_accuracy_value', 'NONE');
#15488 = CIRCLE ( 'NONE', #46317, 1.750000000000003331 ) ;
#15489 = DIRECTION ( 'NONE',  ( 0.000000000000000000, -1.000000000000000000, 0.000000000000000000 ) ) ;
#15490 = DIRECTION ( 'NONE',  ( 0.005002170337468016433, -0.7660444431189770143, -0.6427681459581293666 ) ) ;
#15491 = FACE_OUTER_BOUND ( 'NONE', #42158, .T. ) ;
#15492 = PLANE ( 'NONE',  #18639 ) ;
#15493 = ORIENTED_EDGE ( 'NONE', *, *, #55348, .F. ) ;
#15494 = DIRECTION ( 'NONE',  ( 0.007781995580012663651, 0.000000000000000000, -0.9999697198139515519 ) ) ;
#15495 = ORIENTED_EDGE ( 'NONE', *, *, #35106, .F. ) ;
#15496 = DIRECTION ( 'NONE',  ( 0.005002170337468016433, -0.7660444431189770143, -0.6427681459581293666 ) ) ;
#15497 = CARTESIAN_POINT ( 'NONE',  ( -9.955421239919042264, 0.000000000000000000, 4.004267595880665276 ) ) ;
#15498 = CARTESIAN_POINT ( 'NONE',  ( -24.53374897521541698, 18.49370927080960669, -4.545578601930409413 ) ) ;
#15499 = PLANE ( 'NONE',  #9581 ) ;
#15500 = DIRECTION ( 'NONE',  ( 0.007781995580012662783, 0.000000000000000000, -0.9999697198139514409 ) ) ;
#15501 = ORIENTED_EDGE ( 'NONE', *, *, #43021, .F. ) ;
#15502 = DIRECTION ( 'NONE',  ( 0.9999697198139515519, 0.000000000000000000, 0.007781995580013368816 ) ) ;
#15503 = DIRECTION ( 'NONE',  ( 0.000000000000000000, -0.000000000000000000, -1.000000000000000000 ) ) ;
#15504 = CARTESIAN_POINT ( 'NONE',  ( -15.23885966822254368, 0.7721120973665037690, 2.576587922124613517 ) ) ;
#15505 =( REPRESENTATION_RELATIONSHIP ('NONE','NONE', #51076, #12294 ) REPRESENTATION_RELATIONSHIP_WITH_TRANSFORMATION ( #4494 )SHAPE_REPRESENTATION_RELATIONSHIP( ) );
#15506 = EDGE_CURVE ( 'NONE', #36899, #3799, #19895, .T. ) ;
#15507 = VECTOR ( 'NONE', #43204, 1000.000000000000000 ) ;
#15508 = AXIS2_PLACEMENT_3D ( 'NONE', #26722, #9710, #36109 ) ;
#15509 = CARTESIAN_POINT ( 'NONE',  ( -19.08498593125663234, -3.917936722690662954, 4.169575087627404031 ) ) ;
#15510 = DIRECTION ( 'NONE',  ( 0.9999697198139515519, 0.000000000000000000, 0.007781995580013368816 ) ) ;
#15511 = EDGE_CURVE ( 'NONE', #24571, #50552, #50272, .T. ) ;
#15512 = PLANE ( 'NONE',  #45421 ) ;
#15513 = ADVANCED_FACE ( 'NONE', ( #3689 ), #37492, .F. ) ;
#15514 = DIRECTION ( 'NONE',  ( 0.6427681459581294776, -0.7660444431189769032, 0.005002170337467562802 ) ) ;
#15515 = CARTESIAN_POINT ( 'NONE',  ( -22.40634380310664397, 0.000000000000000000, 5.584705972946605534 ) ) ;
#15516 = DIRECTION ( 'NONE',  ( 0.007781995580012663651, -3.146120232559066537E-19, -0.9999697198139514409 ) ) ;
#15517 = ORIENTED_EDGE ( 'NONE', *, *, #50755, .F. ) ;
#15518 = ORIENTED_EDGE ( 'NONE', *, *, #4511, .F. ) ;
#15519 = AXIS2_PLACEMENT_3D ( 'NONE', #21282, #38897, #4525 ) ;
#15520 = ORIENTED_EDGE ( 'NONE', *, *, #52011, .F. ) ;
#15521 = ORIENTED_EDGE ( 'NONE', *, *, #5581, .F. ) ;
#15522 = VERTEX_POINT ( 'NONE', #12518 ) ;
#15523 = ORIENTED_EDGE ( 'NONE', *, *, #26643, .F. ) ;
#15524 = DIRECTION ( 'NONE',  ( 0.007781995580012663651, 0.000000000000000000, -0.9999697198139515519 ) ) ;
#15525 = CARTESIAN_POINT ( 'NONE',  ( -21.75645231962154824, -2.622721114510657703, 9.437208831783232554 ) ) ;
#15526 = DIRECTION ( 'NONE',  ( -0.005961354470445682716, -0.6427876096865404731, 0.7660212471507180654 ) ) ;
#15527 = EDGE_LOOP ( 'NONE', ( #51783, #19382, #47102, #32026 ) ) ;
#15528 = ORIENTED_EDGE ( 'NONE', *, *, #28403, .F. ) ;
#15529 = VERTEX_POINT ( 'NONE', #25552 ) ;
#15530 = ORIENTED_EDGE ( 'NONE', *, *, #480, .T. ) ;
#15531 = ADVANCED_FACE ( 'NONE', ( #15924 ), #42027, .F. ) ;
#15532 = CARTESIAN_POINT ( 'NONE',  ( -65.19876137812605066, -9.171214889434388340, 1.903866651539666943 ) ) ;
#15533 = ADVANCED_FACE ( 'NONE', ( #55959 ), #34100, .F. ) ;
#15534 = CARTESIAN_POINT ( 'NONE',  ( -14.56888064431065821, -0.1191753592594197858, 12.58947452739191064 ) ) ;
#15535 = DIRECTION ( 'NONE',  ( 0.7660212471507180654, -0.6427876096865404731, 0.005961354470445141482 ) ) ;
#15536 = ORIENTED_EDGE ( 'NONE', *, *, #19834, .F. ) ;
#15537 = DIRECTION ( 'NONE',  ( 0.9321478471874541372, 0.000000000000000000, -0.3620778797217453771 ) ) ;
#15538 = VERTEX_POINT ( 'NONE', #3428 ) ;
#15539 = VECTOR ( 'NONE', #22594, 999.9999999999998863 ) ;
#15540 = VECTOR ( 'NONE', #29168, 1000.000000000000114 ) ;
#15541 = CARTESIAN_POINT ( 'NONE',  ( -13.55751301594631286, -0.1191753592594181482, 2.047824894809781249 ) ) ;
#15542 = ADVANCED_FACE ( 'NONE', ( #50570 ), #20465, .F. ) ;
#15543 = CARTESIAN_POINT ( 'NONE',  ( -12.28722788464031979, 0.000000000000000000, 5.094117146813910146 ) ) ;
#15544 = DIRECTION ( 'NONE',  ( 0.005961354470445682716, -0.6427876096865404731, -0.7660212471507180654 ) ) ;
#15545 = CARTESIAN_POINT ( 'NONE',  ( -11.37675481110584741, 0.000000000000000000, 7.517201133859304996 ) ) ;
#15546 = VECTOR ( 'NONE', #11991, 999.9999999999998863 ) ;
#15547 = CARTESIAN_POINT ( 'NONE',  ( -45.73406441860519323, 4.435048094716154132, 5.000000000000000000 ) ) ;
#15548 = CARTESIAN_POINT ( 'NONE',  ( -69.11683642851026832, -9.015837829197110409, 7.493101075386320531 ) ) ;
#15549 = LINE ( 'NONE', #32879, #23990 ) ;
#15550 = CARTESIAN_POINT ( 'NONE',  ( -9.302286613136297788, 0.000000000000000000, 5.486678719795735404 ) ) ;
#15551 = PLANE ( 'NONE',  #48341 ) ;
#15552 = VERTEX_POINT ( 'NONE', #38061 ) ;
#15553 = DIRECTION ( 'NONE',  ( -0.1139275668495183524, 0.9934890585767659488, 4.694855797473114533E-16 ) ) ;
#15554 = EDGE_LOOP ( 'NONE', ( #42809, #34608, #20537, #3721 ) ) ;
#15555 = DIRECTION ( 'NONE',  ( 0.000000000000000000, -1.000000000000000000, 0.000000000000000000 ) ) ;
#15556 = CARTESIAN_POINT ( 'NONE',  ( -10.67895298262786241, 0.000000000000000000, 3.259972764945120005 ) ) ;
#15557 = CARTESIAN_POINT ( 'NONE',  ( -13.70568740232184091, 0.000000000000000000, 8.237740981534788176 ) ) ;
#15558 = FACE_OUTER_BOUND ( 'NONE', #25343, .T. ) ;
#15559 = DIRECTION ( 'NONE',  ( -0.7660212471507179544, -0.6427876096865405842, -0.005961354470445141482 ) ) ;
#15560 = ADVANCED_FACE ( 'NONE', ( #50826 ), #8236, .F. ) ;
#15561 = VECTOR ( 'NONE', #37137, 1000.000000000000227 ) ;
#15562 = LINE ( 'NONE', #55310, #10296 ) ;
#15563 = EDGE_LOOP ( 'NONE', ( #18192, #20595, #2144, #36863 ) ) ;
#15564 = CARTESIAN_POINT ( 'NONE',  ( -9.742613427545842697, 0.000000000000000000, 2.359269422670635219 ) ) ;
#15565 = CARTESIAN_POINT ( 'NONE',  ( 2.072287782118878319, 0.000000000000000000, -2.950529333540147015 ) ) ;
#15566 = CARTESIAN_POINT ( 'NONE',  ( -8.860905869600903983, 1.712176620043476140E-14, 3.600000000000000089 ) ) ;
#15567 = EDGE_CURVE ( 'NONE', #15599, #34233, #55110, .T. ) ;
#15568 = CARTESIAN_POINT ( 'NONE',  ( -9.342070512798265725, 0.000000000000000000, 10.59882438848031505 ) ) ;
#15569 = DIRECTION ( 'NONE',  ( 0.005961354470445682716, -0.6427876096865404731, -0.7660212471507180654 ) ) ;
#15570 = ADVANCED_FACE ( 'NONE', ( #33262 ), #25292, .F. ) ;
#15571 = LINE ( 'NONE', #7627, #37275 ) ;
#15572 = DIRECTION ( 'NONE',  ( 0.005961354470445682716, -0.6427876096865404731, -0.7660212471507180654 ) ) ;
#15573 = DIRECTION ( 'NONE',  ( -0.005961354470445682716, -0.6427876096865404731, 0.7660212471507180654 ) ) ;
#15574 = EDGE_CURVE ( 'NONE', #40214, #5277, #34369, .T. ) ;
#15575 = DIRECTION ( 'NONE',  ( 0.9999697198139515519, 0.000000000000000000, 0.007781995580013368816 ) ) ;
#15576 = ORIENTED_EDGE ( 'NONE', *, *, #11744, .T. ) ;
#15577 = DIRECTION ( 'NONE',  ( 0.005961354470445682716, -0.6427876096865404731, -0.7660212471507180654 ) ) ;
#15578 = ORIENTED_EDGE ( 'NONE', *, *, #25928, .T. ) ;
#15579 = DIRECTION ( 'NONE',  ( 0.007781995580012663651, -3.146120232559066537E-19, -0.9999697198139514409 ) ) ;
#15580 = DIRECTION ( 'NONE',  ( 0.6427681459581294776, -0.7660444431189769032, 0.005002170337467562802 ) ) ;
#15581 = VECTOR ( 'NONE', #27325, 1000.000000000000227 ) ;
#15582 = VECTOR ( 'NONE', #36739, 1000.000000000000227 ) ;
#15583 = ORIENTED_EDGE ( 'NONE', *, *, #30628, .F. ) ;
#15584 = ORIENTED_EDGE ( 'NONE', *, *, #51804, .F. ) ;
#15585 = DIRECTION ( 'NONE',  ( 0.7660212471507180654, -0.6427876096865404731, 0.005961354470445141482 ) ) ;
#15586 = EDGE_CURVE ( 'NONE', #18997, #33290, #30098, .T. ) ;
#15587 = EDGE_LOOP ( 'NONE', ( #38447, #4394, #153, #45778 ) ) ;
#15588 = ORIENTED_EDGE ( 'NONE', *, *, #37628, .F. ) ;
#15589 = CIRCLE ( 'NONE', #16527, 0.5000000000000004441 ) ;
#15590 = ORIENTED_EDGE ( 'NONE', *, *, #24722, .T. ) ;
#15591 = DIRECTION ( 'NONE',  ( 0.6427681459581294776, -0.7660444431189769032, 0.005002170337467562802 ) ) ;
#15592 = CARTESIAN_POINT ( 'NONE',  ( -13.95152963505244159, 0.000000000000000000, 5.819829305373406036 ) ) ;
#15593 = FACE_OUTER_BOUND ( 'NONE', #47542, .T. ) ;
#15594 = ORIENTED_EDGE ( 'NONE', *, *, #29078, .T. ) ;
#15595 = VECTOR ( 'NONE', #40839, 1000.000000000000114 ) ;
#15596 = EDGE_LOOP ( 'NONE', ( #49767, #42721, #55990, #40677 ) ) ;
#15597 = PLANE ( 'NONE',  #30273 ) ;
#15598 = DIRECTION ( 'NONE',  ( -0.005961354470445682716, -0.6427876096865404731, 0.7660212471507180654 ) ) ;
#15599 = VERTEX_POINT ( 'NONE', #51113 ) ;
#15600 = CARTESIAN_POINT ( 'NONE',  ( -26.13337879274045505, 0.000000000000000000, 6.833023547870798353 ) ) ;
#15601 = EDGE_LOOP ( 'NONE', ( #31755, #3865, #14712, #51173 ) ) ;
#15602 = CARTESIAN_POINT ( 'NONE',  ( -10.20281987176564442, 0.000000000000000000, 1.786349863682072936 ) ) ;
#15603 = DIRECTION ( 'NONE',  ( -0.005002170337468016433, -0.7660444431189770143, 0.6427681459581293666 ) ) ;
#15604 = ORIENTED_EDGE ( 'NONE', *, *, #29886, .F. ) ;
#15605 = LINE ( 'NONE', #32664, #8682 ) ;
#15606 = ADVANCED_FACE ( 'NONE', ( #43184 ), #42335, .F. ) ;
#15607 = VECTOR ( 'NONE', #28656, 999.9999999999998863 ) ;
#15608 = CYLINDRICAL_SURFACE ( 'NONE', #34542, 1.000000000000000444 ) ;
#15609 = ORIENTED_EDGE ( 'NONE', *, *, #5465, .F. ) ;
#15610 = DIRECTION ( 'NONE',  ( -0.5449076811759708816, 0.6444004775717707689, 0.5364919789714475140 ) ) ;
#15611 = AXIS2_PLACEMENT_3D ( 'NONE', #19729, #2666, #10375 ) ;
#15612 = CARTESIAN_POINT ( 'NONE',  ( -20.54049170961573267, 0.000000000000000000, 4.660556269540326646 ) ) ;
#15613 = EDGE_LOOP ( 'NONE', ( #29144, #16247, #16208, #4637 ) ) ;
#15614 = EDGE_CURVE ( 'NONE', #35268, #8997, #16201, .T. ) ;
#15615 = AXIS2_PLACEMENT_3D ( 'NONE', #7938, #54762, #38281 ) ;
#15616 = VECTOR ( 'NONE', #35220, 999.9999999999998863 ) ;
#15617 = CARTESIAN_POINT ( 'NONE',  ( -50.27554558092695913, 4.209026340267034705, -5.000000000000000000 ) ) ;
#15618 = PLANE ( 'NONE',  #4252 ) ;
#15619 = LINE ( 'NONE', #49732, #14947 ) ;
#15620 = LINE ( 'NONE', #54518, #36808 ) ;
#15621 = EDGE_CURVE ( 'NONE', #3020, #26788, #25013, .T. ) ;
#15622 = CARTESIAN_POINT ( 'NONE',  ( -27.06630483948590893, -0.1191753592594197858, 7.295098399573937797 ) ) ;
#15624 = EDGE_CURVE ( 'NONE', #32592, #4309, #47134, .T. ) ;
#15623 = LINE ( 'NONE', #11389, #40627 ) ;
#15625 = VECTOR ( 'NONE', #33978, 1000.000000000000000 ) ;
#15626 = FACE_OUTER_BOUND ( 'NONE', #23335, .T. ) ;
#15627 = AXIS2_PLACEMENT_3D ( 'NONE', #42799, #7611, #7922 ) ;
#15628 = VERTEX_POINT ( 'NONE', #16466 ) ;
#15629 =( LENGTH_UNIT ( ) NAMED_UNIT ( * ) SI_UNIT ( .MILLI., .METRE. ) );
#15630 = CARTESIAN_POINT ( 'NONE',  ( -58.00000000000000711, -9.999999999999998224, 7.102951435054649637E-15 ) ) ;
#15631 = CARTESIAN_POINT ( 'NONE',  ( -66.55592414517043665, -9.044681206892926412E-12, 1.786740587093984534 ) ) ;
#15632 = ORIENTED_EDGE ( 'NONE', *, *, #49629, .T. ) ;
#15633 = CARTESIAN_POINT ( 'NONE',  ( -24.26986129792355129, -0.1191753592594197858, 6.208864760408702388 ) ) ;
#15634 = EDGE_CURVE ( 'NONE', #34711, #3752, #35646, .T. ) ;
#15635 = CARTESIAN_POINT ( 'NONE',  ( -13.92434549911562058, 0.000000000000000000, 2.326726216758550514 ) ) ;
#15636 = EDGE_CURVE ( 'NONE', #21767, #34530, #51418, .T. ) ;
#15637 = FACE_BOUND ( 'NONE', #54536, .T. ) ;
#15638 = LINE ( 'NONE', #32978, #6993 ) ;
#15639 = EDGE_CURVE ( 'NONE', #33398, #54767, #31218, .T. ) ;
#15640 = CARTESIAN_POINT ( 'NONE',  ( -58.00000000000000711, 0.000000000000000000, -2.999999999999994227 ) ) ;
#15641 = EDGE_LOOP ( 'NONE', ( #11686, #42539, #30899, #18132 ) ) ;
#15642 = ORIENTED_EDGE ( 'NONE', *, *, #15380, .F. ) ;
#15643 = CARTESIAN_POINT ( 'NONE',  ( -12.76623504900782180, 0.000000000000000000, 6.937049751334724235 ) ) ;
#15644 = FACE_OUTER_BOUND ( 'NONE', #34312, .T. ) ;
#15645 = EDGE_CURVE ( 'NONE', #713, #9548, #259, .T. ) ;
#15646 = DIRECTION ( 'NONE',  ( 0.005961354470445682716, -0.6427876096865404731, -0.7660212471507180654 ) ) ;
#15647 = ORIENTED_EDGE ( 'NONE', *, *, #44506, .F. ) ;
#15648 = DIRECTION ( 'NONE',  ( 0.9999697198139515519, 0.000000000000000000, 0.007781995580013368816 ) ) ;
#15649 = VECTOR ( 'NONE', #28431, 999.9999999999998863 ) ;
#15650 = EDGE_LOOP ( 'NONE', ( #40575, #15129, #39882, #43212 ) ) ;
#15651 = CYLINDRICAL_SURFACE ( 'NONE', #25646, 1.000000000000000222 ) ;
#15652 = ADVANCED_FACE ( 'NONE', ( #8830 ), #52520, .F. ) ;
#15653 = EDGE_LOOP ( 'NONE', ( #26650, #19400, #12954, #1779 ) ) ;
#15654 = ORIENTED_EDGE ( 'NONE', *, *, #40263, .F. ) ;
#15655 = LINE ( 'NONE', #7722, #42018 ) ;
#15656 = VECTOR ( 'NONE', #28376, 999.9999999999998863 ) ;
#15657 = CARTESIAN_POINT ( 'NONE',  ( -10.32371341784202023, -0.1191753592594179401, 4.470736558909812253 ) ) ;
#15658 = DIRECTION ( 'NONE',  ( -0.005002170337468016433, -0.7660444431189770143, 0.6427681459581293666 ) ) ;
#15659 = VERTEX_POINT ( 'NONE', #9081 ) ;
#15660 = VECTOR ( 'NONE', #38971, 1000.000000000000114 ) ;
#15661 = AXIS2_PLACEMENT_3D ( 'NONE', #5890, #40802, #53321 ) ;
#15662 = DIRECTION ( 'NONE',  ( 0.6427681459581294776, -0.7660444431189769032, 0.005002170337467562802 ) ) ;
#15663 = ORIENTED_EDGE ( 'NONE', *, *, #1417, .F. ) ;
#15664 = ORIENTED_EDGE ( 'NONE', *, *, #37190, .T. ) ;
#15665 = AXIS2_PLACEMENT_3D ( 'NONE', #21699, #30779, #56062 ) ;
#15666 = ORIENTED_EDGE ( 'NONE', *, *, #5406, .T. ) ;
#15667 = PLANE ( 'NONE',  #21367 ) ;
#15668 = AXIS2_PLACEMENT_3D ( 'NONE', #2310, #20480, #36977 ) ;
#15669 = DIRECTION ( 'NONE',  ( -0.7660212471507179544, -0.6427876096865405842, -0.005961354470445141482 ) ) ;
#15670 = ORIENTED_EDGE ( 'NONE', *, *, #50925, .T. ) ;
#15671 = PLANE ( 'NONE',  #23924 ) ;
#15672 = ORIENTED_EDGE ( 'NONE', *, *, #54541, .T. ) ;
#15673 = CARTESIAN_POINT ( 'NONE',  ( -26.26580391614848864, 17.49370688441070953, -4.657437592157546824 ) ) ;
#15674 = DIRECTION ( 'NONE',  ( -0.005961354470445682716, -0.6427876096865404731, 0.7660212471507180654 ) ) ;
#15675 = ORIENTED_EDGE ( 'NONE', *, *, #10148, .F. ) ;
#15677 = VECTOR ( 'NONE', #23657, 1000.000000000000227 ) ;
#15676 = CARTESIAN_POINT ( 'NONE',  ( -14.00280974873554030, 0.000000000000000000, 12.40921378708904044 ) ) ;
#15678 = EDGE_CURVE ( 'NONE', #36899, #5305, #39755, .T. ) ;
#15679 = ORIENTED_EDGE ( 'NONE', *, *, #6131, .T. ) ;
#15680 = VECTOR ( 'NONE', #2958, 1000.000000000000227 ) ;
#15681 = DIRECTION ( 'NONE',  ( 0.007781995580012663651, 0.000000000000000000, -0.9999697198139515519 ) ) ;
#15682 = DIRECTION ( 'NONE',  ( 0.2426528472758542054, 0.7422098413412800966, 0.6246952433987894571 ) ) ;
#15683 = PLANE ( 'NONE',  #6008 ) ;
#15684 = DIRECTION ( 'NONE',  ( -0.5364919789714478471, 0.6444004775717705469, -0.5449076811759709926 ) ) ;
#15685 = CARTESIAN_POINT ( 'NONE',  ( -21.47263955680318404, 0.000000000000000000, 5.022634149262071190 ) ) ;
#15686 = DIRECTION ( 'NONE',  ( -0.005002170337468016433, -0.7660444431189770143, 0.6427681459581293666 ) ) ;
#15687 = EDGE_LOOP ( 'NONE', ( #46985, #35852, #49604, #24713 ) ) ;
#15688 = EDGE_CURVE ( 'NONE', #53048, #26165, #44292, .T. ) ;
#15689 = VECTOR ( 'NONE', #41345, 1000.000000000000000 ) ;
#15690 = EDGE_CURVE ( 'NONE', #36809, #41926, #38912, .T. ) ;
#15691 = ORIENTED_EDGE ( 'NONE', *, *, #19245, .T. ) ;
#15692 = FACE_OUTER_BOUND ( 'NONE', #19679, .T. ) ;
#15693 = CARTESIAN_POINT ( 'NONE',  ( -9.175487151985130652, -0.1191753592594191058, 3.371676111792005770 ) ) ;
#15694 = AXIS2_PLACEMENT_3D ( 'NONE', #38663, #17079, #8554 ) ;
#15695 = CARTESIAN_POINT ( 'NONE',  ( -19.60834386242827776, 0.000000000000000000, 4.298478389818581213 ) ) ;
#15696 = PLANE ( 'NONE',  #22168 ) ;
#15698 = ADVANCED_FACE ( 'NONE', ( #5391 ), #5122, .F. ) ;
#15697 = CARTESIAN_POINT ( 'NONE',  ( -16.81267852042391198, -0.1191753592594197858, 3.312241722634738039 ) ) ;
#15699 = DIRECTION ( 'NONE',  ( -0.005961354470445682716, -0.6427876096865404731, 0.7660212471507180654 ) ) ;
#15700 = VERTEX_POINT ( 'NONE', #30931 ) ;
#15701 = LINE ( 'NONE', #28793, #24978 ) ;
#15702 = LINE ( 'NONE', #29908, #31419 ) ;
#15703 = EDGE_LOOP ( 'NONE', ( #32125, #29376, #46729, #17872 ) ) ;
#15705 = DIRECTION ( 'NONE',  ( -0.6246952433987893460, -0.7422098413412802076, 0.2426528472758542054 ) ) ;
#15704 = AXIS2_PLACEMENT_3D ( 'NONE', #39013, #43296, #51525 ) ;
#15706 = DIRECTION ( 'NONE',  ( 0.9999697198139515519, 0.000000000000000000, 0.007781995580013368816 ) ) ;
#15707 = ORIENTED_EDGE ( 'NONE', *, *, #26796, .F. ) ;
#15708 = VECTOR ( 'NONE', #31385, 999.9999999999998863 ) ;
#15709 = PLANE ( 'NONE',  #9823 ) ;
#15710 = CARTESIAN_POINT ( 'NONE',  ( -22.40478740399063895, 0.000000000000000000, 5.384712028983816623 ) ) ;
#15711 = EDGE_CURVE ( 'NONE', #9919, #47750, #573, .T. ) ;
#15712 = CARTESIAN_POINT ( 'NONE',  ( -9.749679188945689745, 0.000000000000000000, 3.267204588481138927 ) ) ;
#15713 = DIRECTION ( 'NONE',  ( 0.000000000000000000, -0.000000000000000000, -1.000000000000000000 ) ) ;
#15714 = EDGE_CURVE ( 'NONE', #50133, #41831, #26678, .T. ) ;
#15715 = CARTESIAN_POINT ( 'NONE',  ( -11.73199437589168781, -0.1191753592594185784, 6.306437339894606531 ) ) ;
#15716 = EDGE_LOOP ( 'NONE', ( #9844, #29796, #18490, #50803 ) ) ;
#15717 = VECTOR ( 'NONE', #16150, 1000.000000000000000 ) ;
#15718 = ORIENTED_EDGE ( 'NONE', *, *, #39138, .F. ) ;
#15719 = EDGE_CURVE ( 'NONE', #48671, #35152, #39472, .T. ) ;
#15720 = DIRECTION ( 'NONE',  ( 0.007781995580012663651, 0.000000000000000000, -0.9999697198139515519 ) ) ;
#15721 = DIRECTION ( 'NONE',  ( 0.9999697198139515519, 0.000000000000000000, 0.007781995580013368816 ) ) ;
#15722 = DIRECTION ( 'NONE',  ( -0.05705673239519651330, 0.9983709377222390602, 2.401210743435858319E-16 ) ) ;
#15723 = FACE_OUTER_BOUND ( 'NONE', #52357, .T. ) ;
#15724 = ADVANCED_FACE ( 'NONE', ( #17305 ), #13066, .F. ) ;
#15725 = CARTESIAN_POINT ( 'NONE',  ( 0.09621548157177266247, -1.683565401097097070, -3.964956190634384326E-16 ) ) ;
#15726 = DIRECTION ( 'NONE',  ( 0.000000000000000000, -0.000000000000000000, -1.000000000000000000 ) ) ;
#15727 = ORIENTED_EDGE ( 'NONE', *, *, #50033, .T. ) ;
#15728 = DIRECTION ( 'NONE',  ( -0.7660212471507179544, -0.6427876096865405842, -0.005961354470445141482 ) ) ;
#15729 = DIRECTION ( 'NONE',  ( 0.007781995580012663651, 0.000000000000000000, -0.9999697198139515519 ) ) ;
#15730 = CARTESIAN_POINT ( 'NONE',  ( 2.072287782118878319, 0.000000000000000000, -2.950529333540147015 ) ) ;
#15731 = ORIENTED_EDGE ( 'NONE', *, *, #2561, .F. ) ;
#15732 = VECTOR ( 'NONE', #47836, 999.9999999999998863 ) ;
#15733 = DIRECTION ( 'NONE',  ( 0.000000000000000000, -0.000000000000000000, -1.000000000000000000 ) ) ;
#15734 = DIRECTION ( 'NONE',  ( 0.007781995580012663651, -3.146120232559066537E-19, -0.9999697198139514409 ) ) ;
#15735 = AXIS2_PLACEMENT_3D ( 'NONE', #36585, #53076, #5944 ) ;
#15736 = DIRECTION ( 'NONE',  ( 0.7660212471507180654, -0.6427876096865404731, 0.005961354470445141482 ) ) ;
#15737 = VERTEX_POINT ( 'NONE', #14209 ) ;
#15738 = DIRECTION ( 'NONE',  ( 0.7660212471507180654, -0.6427876096865404731, 0.005961354470445141482 ) ) ;
#15739 = CIRCLE ( 'NONE', #47489, 1.000000000000000000 ) ;
#15740 = EDGE_LOOP ( 'NONE', ( #22617, #37455, #24581, #7667 ) ) ;
#15741 = ORIENTED_EDGE ( 'NONE', *, *, #11387, .F. ) ;
#15742 = ORIENTED_EDGE ( 'NONE', *, *, #34059, .T. ) ;
#15743 = ORIENTED_EDGE ( 'NONE', *, *, #322, .T. ) ;
#15744 = ORIENTED_EDGE ( 'NONE', *, *, #23710, .F. ) ;
#15745 = AXIS2_PLACEMENT_3D ( 'NONE', #40050, #299, #31561 ) ;
#15746 = DIRECTION ( 'NONE',  ( -0.6427681459581293666, -0.7660444431189770143, -0.005002170337467561935 ) ) ;
#15748 = EDGE_CURVE ( 'NONE', #7193, #223, #53091, .T. ) ;
#15747 = EDGE_LOOP ( 'NONE', ( #46901, #2543, #47568, #16786, #40826, #55078, #5234 ) ) ;
#15749 = AXIS2_PLACEMENT_3D ( 'NONE', #53369, #5951, #44834 ) ;
#15750 = VERTEX_POINT ( 'NONE', #9934 ) ;
#15751 = PLANE ( 'NONE',  #23134 ) ;
#15752 = ORIENTED_EDGE ( 'NONE', *, *, #37827, .F. ) ;
#15753 = EDGE_CURVE ( 'NONE', #10299, #15737, #39172, .T. ) ;
#15754 = ORIENTED_EDGE ( 'NONE', *, *, #20395, .F. ) ;
#15755 = VECTOR ( 'NONE', #20975, 999.9999999999998863 ) ;
#15756 = AXIS2_PLACEMENT_3D ( 'NONE', #5279, #5828, #1570 ) ;
#15757 = PLANE ( 'NONE',  #49226 ) ;
#15758 = CARTESIAN_POINT ( 'NONE',  ( 1.086233639165236964, 0.000000000000000000, 2.796443541562362078 ) ) ;
#15759 = CARTESIAN_POINT ( 'NONE',  ( -13.08486533123210194, 0.000000000000000000, 1.963927175729152541 ) ) ;
#15760 = DIRECTION ( 'NONE',  ( 0.9999697198139515519, 0.000000000000000000, 0.007781995580013368816 ) ) ;
#15761 = ORIENTED_EDGE ( 'NONE', *, *, #27351, .T. ) ;
#15762 = CARTESIAN_POINT ( 'NONE',  ( -23.33771345073609638, -0.1191753592594197858, 5.846786880686956955 ) ) ;
#15763 = VERTEX_POINT ( 'NONE', #35476 ) ;
#15764 = EDGE_CURVE ( 'NONE', #5026, #19711, #56216, .T. ) ;
#15765 = ADVANCED_FACE ( 'NONE', ( #13891 ), #13365, .F. ) ;
#15766 = EDGE_CURVE ( 'NONE', #2545, #46574, #17903, .T. ) ;
#15767 = EDGE_LOOP ( 'NONE', ( #52236, #9981, #37002, #32843 ) ) ;
#15768 = LINE ( 'NONE', #46150, #10396 ) ;
#15769 = CARTESIAN_POINT ( 'NONE',  ( -21.47263955680318404, 0.000000000000000000, 5.022634149262071190 ) ) ;
#15770 = ADVANCED_FACE ( 'NONE', ( #29309 ), #56011, .F. ) ;
#15771 = DIRECTION ( 'NONE',  ( 0.007781995580012663651, -3.146120232559066537E-19, -0.9999697198139514409 ) ) ;
#15772 = DIRECTION ( 'NONE',  ( 0.007781995580012663651, 0.000000000000000000, -0.9999697198139515519 ) ) ;
#15773 = AXIS2_PLACEMENT_3D ( 'NONE', #30216, #13182, #17417 ) ;
#15774 = DIRECTION ( 'NONE',  ( 0.005002170337468016433, -0.7660444431189770143, -0.6427681459581293666 ) ) ;
#15775 = DIRECTION ( 'NONE',  ( -0.7660212471507179544, -0.6427876096865405842, -0.005961354470445141482 ) ) ;
#15776 = ORIENTED_EDGE ( 'NONE', *, *, #21979, .T. ) ;
#15777 = LINE ( 'NONE', #14960, #12972 ) ;
#15778 = AXIS2_PLACEMENT_3D ( 'NONE', #7258, #54388, #24305 ) ;
#15779 = VERTEX_POINT ( 'NONE', #46625 ) ;
#15780 = DIRECTION ( 'NONE',  ( -0.005002170337468016433, -0.7660444431189770143, 0.6427681459581293666 ) ) ;
#15781 = PLANE ( 'NONE',  #53192 ) ;
#15782 = DIRECTION ( 'NONE',  ( 0.000000000000000000, -1.000000000000000000, 0.000000000000000000 ) ) ;
#15783 = AXIS2_PLACEMENT_3D ( 'NONE', #39152, #51398, #8218 ) ;
#15784 = CARTESIAN_POINT ( 'NONE',  ( -16.79925329029790149, 0.000000000000000000, 13.49544742625427496 ) ) ;
#15785 = ADVANCED_FACE ( 'NONE', ( #4036 ), #38104, .F. ) ;
#15786 = DIRECTION ( 'NONE',  ( 0.5449076811759707706, 0.6444004775717708799, -0.5364919789714476250 ) ) ;
#15787 = EDGE_CURVE ( 'NONE', #16128, #45114, #38694, .T. ) ;
#15788 = ORIENTED_EDGE ( 'NONE', *, *, #6050, .T. ) ;
#15789 = ORIENTED_EDGE ( 'NONE', *, *, #12472, .T. ) ;
#15790 = ADVANCED_FACE ( 'NONE', ( #17102 ), #12281, .F. ) ;
#15791 = VECTOR ( 'NONE', #53880, 999.9999999999998863 ) ;
#15792 = LINE ( 'NONE', #33134, #33933 ) ;
#15793 = DIRECTION ( 'NONE',  ( 0.007781995580012663651, -3.146120232559066537E-19, -0.9999697198139514409 ) ) ;
#15794 = CARTESIAN_POINT ( 'NONE',  ( -1.086233639165236964, 0.000000000000000000, -2.796443541562362078 ) ) ;
#15795 = VECTOR ( 'NONE', #39947, 1000.000000000000227 ) ;
#15796 = ADVANCED_FACE ( 'NONE', ( #8025 ), #12830, .F. ) ;
#15797 = FACE_OUTER_BOUND ( 'NONE', #12503, .T. ) ;
#15798 = PLANE ( 'NONE',  #19407 ) ;
#15799 = DIRECTION ( 'NONE',  ( 0.7660212471507180654, -0.6427876096865404731, 0.005961354470445141482 ) ) ;
#15800 = CARTESIAN_POINT ( 'NONE',  ( -11.22056963685719211, 0.000000000000000000, 1.239771416285661010 ) ) ;
#15801 = EDGE_CURVE ( 'NONE', #9624, #46898, #21361, .T. ) ;
#15802 = AXIS2_PLACEMENT_3D ( 'NONE', #45616, #6731, #28878 ) ;
#15803 = VECTOR ( 'NONE', #54972, 1000.000000000000227 ) ;
#15804 = DIRECTION ( 'NONE',  ( 0.000000000000000000, 0.000000000000000000, -1.000000000000000000 ) ) ;
#15805 = DIRECTION ( 'NONE',  ( 0.5364919789714477361, 0.6444004775717706579, 0.5449076811759711036 ) ) ;
#15806 = VERTEX_POINT ( 'NONE', #34683 ) ;
#15807 = VECTOR ( 'NONE', #22894, 1000.000000000000227 ) ;
#15808 = ORIENTED_EDGE ( 'NONE', *, *, #20447, .T. ) ;
#15809 = VERTEX_POINT ( 'NONE', #3187 ) ;
#15810 = ORIENTED_EDGE ( 'NONE', *, *, #4873, .T. ) ;
#15811 = VECTOR ( 'NONE', #15060, 1000.000000000000114 ) ;
#15812 = EDGE_LOOP ( 'NONE', ( #25964, #9329 ) ) ;
#15813 = LINE ( 'NONE', #54426, #21461 ) ;
#15814 = DIRECTION ( 'NONE',  ( -0.5449076811759708816, 0.6444004775717707689, 0.5364919789714475140 ) ) ;
#15815 = CARTESIAN_POINT ( 'NONE',  ( -14.66887761629205222, 0.000000000000000000, 12.58869632783390990 ) ) ;
#15816 = VECTOR ( 'NONE', #21917, 1000.000000000000227 ) ;
#15817 = ORIENTED_EDGE ( 'NONE', *, *, #21440, .T. ) ;
#15818 = FACE_OUTER_BOUND ( 'NONE', #44331, .T. ) ;
#15819 = EDGE_LOOP ( 'NONE', ( #19747, #46329, #20612, #19517 ) ) ;
#15820 = DIRECTION ( 'NONE',  ( 0.9999697198139515519, 0.000000000000000000, 0.007781995580013368816 ) ) ;
#15821 = EDGE_LOOP ( 'NONE', ( #54698, #27244, #54440, #1700 ) ) ;
#15822 = AXIS2_PLACEMENT_3D ( 'NONE', #46416, #28856, #29404 ) ;
#15823 = CARTESIAN_POINT ( 'NONE',  ( -66.38245585351968714, -9.306954111037352817, -3.536654368697047968 ) ) ;
#15824 = VECTOR ( 'NONE', #49891, 1000.000000000000000 ) ;
#15825 = PLANE ( 'NONE',  #1016 ) ;
#15826 = DIRECTION ( 'NONE',  ( 0.5364919789714477361, 0.6444004775717706579, 0.5449076811759711036 ) ) ;
#15827 = EDGE_LOOP ( 'NONE', ( #47477, #46814, #6142, #39279 ) ) ;
#15828 = LINE ( 'NONE', #3616, #50945 ) ;
#15829 = VERTEX_POINT ( 'NONE', #30152 ) ;
#15830 = VECTOR ( 'NONE', #17058, 1000.000000000000227 ) ;
#15831 = ADVANCED_FACE ( 'NONE', ( #43240 ), #20521, .F. ) ;
#15832 = EDGE_CURVE ( 'NONE', #18640, #3029, #20031, .T. ) ;
#15833 = CARTESIAN_POINT ( 'NONE',  ( 1.086233639165236964, 0.000000000000000000, 2.796443541562362078 ) ) ;
#15834 = CARTESIAN_POINT ( 'NONE',  ( -20.70246366968693508, 4.495856970884011261, 4.580030303656299928 ) ) ;
#15835 = ADVANCED_FACE ( 'NONE', ( #37850 ), #50874, .F. ) ;
#15836 = VECTOR ( 'NONE', #27981, 999.9999999999998863 ) ;
#15837 = DIRECTION ( 'NONE',  ( -0.5449076811759708816, 0.6444004775717707689, 0.5364919789714475140 ) ) ;
#15838 = LINE ( 'NONE', #37409, #19661 ) ;
#15839 = AXIS2_PLACEMENT_3D ( 'NONE', #8961, #26264, #25421 ) ;
#15840 = CARTESIAN_POINT ( 'NONE',  ( 4.912750499197526821, -1.131233082521083455, -2.061810099490656079 ) ) ;
#15841 = CARTESIAN_POINT ( 'NONE',  ( -17.13623937202426362, 3.524445264749008100, 9.321833557735295983 ) ) ;
#15842 = DIRECTION ( 'NONE',  ( 0.9999697198139515519, 0.000000000000000000, 0.007781995580013368816 ) ) ;
#15843 = CARTESIAN_POINT ( 'NONE',  ( -22.40478740399063895, 0.000000000000000000, 5.384712028983816623 ) ) ;
#15844 = DIRECTION ( 'NONE',  ( -0.5449076811759708816, 0.6444004775717707689, 0.5364919789714475140 ) ) ;
#15845 = ORIENTED_EDGE ( 'NONE', *, *, #27074, .F. ) ;
#15846 = PLANE ( 'NONE',  #20155 ) ;
#15847 = ORIENTED_EDGE ( 'NONE', *, *, #3224, .F. ) ;
#15848 = LINE ( 'NONE', #32364, #28366 ) ;
#15849 = DIRECTION ( 'NONE',  ( 0.5364919789714477361, 0.6444004775717706579, 0.5449076811759711036 ) ) ;
#15850 = LINE ( 'NONE', #24373, #55850 ) ;
#15851 = CARTESIAN_POINT ( 'NONE',  ( -15.02486367781824939, -0.03739765774599677212, 2.656112488575108621 ) ) ;
#15852 = CARTESIAN_POINT ( 'NONE',  ( -0.3920807322492407820, -4.603227297713195831, 3.370671047187119296 ) ) ;
#15853 = VECTOR ( 'NONE', #50520, 1000.000000000000227 ) ;
#15854 = CARTESIAN_POINT ( 'NONE',  ( -50.02554558092695913, 3.776013638374815962, -5.000000000000000000 ) ) ;
#15855 = DIRECTION ( 'NONE',  ( 1.033913469176933741E-17, -6.946941504619725221E-18, 0.9999999999999998890 ) ) ;
#15856 = VECTOR ( 'NONE', #29757, 1000.000000000000227 ) ;
#15857 = ORIENTED_EDGE ( 'NONE', *, *, #24049, .T. ) ;
#15858 = PLANE ( 'NONE',  #16554 ) ;
#15859 = CARTESIAN_POINT ( 'NONE',  ( -18.19747506107908563, 0.000000000000000000, 14.03856424583689311 ) ) ;
#15860 = DIRECTION ( 'NONE',  ( -0.6427681459581293666, -0.7660444431189770143, -0.005002170337467561935 ) ) ;
#15861 = PLANE ( 'NONE',  #16420 ) ;
#15862 = VECTOR ( 'NONE', #16331, 1000.000000000000227 ) ;
#15863 = DIRECTION ( 'NONE',  ( -0.6427681459581293666, -0.7660444431189770143, -0.005002170337467561935 ) ) ;
#15864 = CARTESIAN_POINT ( 'NONE',  ( -23.33849165029409889, 0.000000000000000000, 5.946783852668351855 ) ) ;
#15865 = VECTOR ( 'NONE', #12510, 999.9999999999998863 ) ;
#15866 = DIRECTION ( 'NONE',  ( 0.005961354470445682716, -0.6427876096865404731, -0.7660212471507180654 ) ) ;
#15867 = EDGE_CURVE ( 'NONE', #34537, #36412, #25, .T. ) ;
#15868 = PLANE ( 'NONE',  #46866 ) ;
#15869 = CARTESIAN_POINT ( 'NONE',  ( -12.17271348132147679, -4.565544526780664469, 1.463951646762539971 ) ) ;
#15870 = EDGE_LOOP ( 'NONE', ( #37320, #15227, #32743, #28626 ) ) ;
#15871 = LINE ( 'NONE', #6516, #53899 ) ;
#15872 = VECTOR ( 'NONE', #38566, 999.9999999999998863 ) ;
#15873 = DIRECTION ( 'NONE',  ( 0.005002170337468016433, -0.7660444431189770143, -0.6427681459581293666 ) ) ;
#15874 = AXIS2_PLACEMENT_3D ( 'NONE', #23667, #31917, #10893 ) ;
#15875 = ORIENTED_EDGE ( 'NONE', *, *, #30008, .T. ) ;
#15876 = ADVANCED_FACE ( 'NONE', ( #51469 ), #25338, .F. ) ;
#15877 = VECTOR ( 'NONE', #16908, 1000.000000000000114 ) ;
#15878 = CARTESIAN_POINT ( 'NONE',  ( -15.25286141696295594, -5.375054281893161701, 11.42804088947178087 ) ) ;
#15879 = FACE_BOUND ( 'NONE', #2018, .T. ) ;
#15880 = EDGE_CURVE ( 'NONE', #42286, #9201, #29880, .T. ) ;
#15881 = VECTOR ( 'NONE', #26682, 999.9999999999998863 ) ;
#15882 = ORIENTED_EDGE ( 'NONE', *, *, #49337, .T. ) ;
#15883 = EDGE_CURVE ( 'NONE', #44182, #19378, #3737, .T. ) ;
#15884 = ORIENTED_EDGE ( 'NONE', *, *, #34913, .T. ) ;
#15885 = LINE ( 'NONE', #33226, #42958 ) ;
#15886 = AXIS2_PLACEMENT_3D ( 'NONE', #4012, #30128, #43216 ) ;
#15887 = ORIENTED_EDGE ( 'NONE', *, *, #2810, .F. ) ;
#15888 = AXIS2_PLACEMENT_3D ( 'NONE', #49164, #53177, #9741 ) ;
#15889 = ORIENTED_EDGE ( 'NONE', *, *, #18388, .F. ) ;
#15890 = ORIENTED_EDGE ( 'NONE', *, *, #50485, .T. ) ;
#15891 = CARTESIAN_POINT ( 'NONE',  ( -22.40556560354864146, -0.1191753592594197858, 5.484709000965211523 ) ) ;
#15892 = PLANE ( 'NONE',  #29662 ) ;
#15893 = CARTESIAN_POINT ( 'NONE',  ( -18.16487629518032065, 0.000000000000000000, 9.849692835296727011 ) ) ;
#15894 = ORIENTED_EDGE ( 'NONE', *, *, #44531, .F. ) ;
#15895 = ORIENTED_EDGE ( 'NONE', *, *, #38271, .T. ) ;
#15896 = VECTOR ( 'NONE', #32572, 999.9999999999998863 ) ;
#15897 = FACE_OUTER_BOUND ( 'NONE', #55691, .T. ) ;
#15898 = CARTESIAN_POINT ( 'NONE',  ( -15.53968616252791790, 0.000000000000000000, 5.068805764437843919 ) ) ;
#15899 = AXIS2_PLACEMENT_3D ( 'NONE', #36805, #11522, #41039 ) ;
#15900 = ORIENTED_EDGE ( 'NONE', *, *, #39788, .T. ) ;
#15901 = CARTESIAN_POINT ( 'NONE',  ( -27.06552663992790997, 0.000000000000000000, 7.195101427592543786 ) ) ;
#15902 = ADVANCED_FACE ( 'NONE', ( #47180 ), #42641, .F. ) ;
#15903 = ORIENTED_EDGE ( 'NONE', *, *, #3656, .F. ) ;
#15904 = VECTOR ( 'NONE', #3900, 999.9999999999998863 ) ;
#15905 = FACE_OUTER_BOUND ( 'NONE', #3141, .T. ) ;
#15906 = LINE ( 'NONE', #11369, #53921 ) ;
#15908 = EDGE_LOOP ( 'NONE', ( #9450, #16249, #49694, #12428, #25978 ) ) ;
#15907 = EDGE_CURVE ( 'NONE', #16052, #51781, #51168, .T. ) ;
#15909 = DIRECTION ( 'NONE',  ( -0.9999697198139514409, -0.000000000000000000, -0.007781995580013368816 ) ) ;
#15910 = VECTOR ( 'NONE', #49909, 1000.000000000000227 ) ;
#15911 = EDGE_CURVE ( 'NONE', #31521, #19558, #27282, .T. ) ;
#15912 = EDGE_CURVE ( 'NONE', #1446, #21607, #43755, .T. ) ;
#15913 = DIRECTION ( 'NONE',  ( 0.007781995580012662783, 0.000000000000000000, -0.9999697198139514409 ) ) ;
#15914 = AXIS2_PLACEMENT_3D ( 'NONE', #20449, #19883, #54252 ) ;
#15915 = AXIS2_PLACEMENT_3D ( 'NONE', #2620, #2051, #45494 ) ;
#15916 = ORIENTED_EDGE ( 'NONE', *, *, #2735, .F. ) ;
#15917 = CARTESIAN_POINT ( 'NONE',  ( -18.34475186460612761, 0.000000000000000000, 7.262968513376373281 ) ) ;
#15918 = DIRECTION ( 'NONE',  ( 0.5364919789714477361, 0.6444004775717706579, 0.5449076811759711036 ) ) ;
#15919 = CARTESIAN_POINT ( 'NONE',  ( -19.73541775872651272, 0.000000000000000000, 6.835171408663078374 ) ) ;
#15920 = EDGE_LOOP ( 'NONE', ( #54177, #36834, #15027, #39073 ) ) ;
#15921 = VECTOR ( 'NONE', #838, 1000.000000000000114 ) ;
#15922 = AXIS2_PLACEMENT_3D ( 'NONE', #43071, #36172, #465 ) ;
#15923 = LINE ( 'NONE', #49730, #23783 ) ;
#15924 = FACE_OUTER_BOUND ( 'NONE', #14774, .T. ) ;
#15925 = DIRECTION ( 'NONE',  ( 0.9999697198139515519, 0.000000000000000000, 0.007781995580013368816 ) ) ;
#15926 = AXIS2_PLACEMENT_3D ( 'NONE', #53338, #22401, #48494 ) ;
#15927 = CARTESIAN_POINT ( 'NONE',  ( -9.509585063225655333, 0.000000000000000000, 6.423735671158050664 ) ) ;
#15928 = PLANE ( 'NONE',  #32190 ) ;
#15929 = CARTESIAN_POINT ( 'NONE',  ( -14.93495759592298988, 0.000000000000000000, 12.77129166681078409 ) ) ;
#15930 = ADVANCED_FACE ( 'NONE', ( #35526 ), #44332, .F. ) ;
#15931 = VECTOR ( 'NONE', #18544, 999.9999999999998863 ) ;
#15932 = AXIS2_PLACEMENT_3D ( 'NONE', #27372, #14886, #964 ) ;
#15933 = CARTESIAN_POINT ( 'NONE',  ( -67.14664173531406277, -11.40769374184509388, -8.053057903409269969 ) ) ;
#15934 = ORIENTED_EDGE ( 'NONE', *, *, #11911, .T. ) ;
#15935 = DIRECTION ( 'NONE',  ( -0.005002170337468016433, -0.7660444431189770143, 0.6427681459581293666 ) ) ;
#15936 = LINE ( 'NONE', #19343, #21422 ) ;
#15937 = LINE ( 'NONE', #55969, #8764 ) ;
#15938 = ORIENTED_EDGE ( 'NONE', *, *, #38408, .F. ) ;
#15939 = CARTESIAN_POINT ( 'NONE',  ( -18.97909103874558312, 0.7721120973665051013, 5.520612101438020503 ) ) ;
#15940 = CARTESIAN_POINT ( 'NONE',  ( 2.072287782118878319, 0.000000000000000000, -2.950529333540147015 ) ) ;
#15941 = PLANE ( 'NONE',  #481 ) ;
#15942 = FACE_OUTER_BOUND ( 'NONE', #38471, .T. ) ;
#15943 = CARTESIAN_POINT ( 'NONE',  ( -14.56888064431065821, -0.1191753592594197858, 12.58947452739191064 ) ) ;
#15944 = VECTOR ( 'NONE', #21943, 1000.000000000000227 ) ;
#15945 = ORIENTED_EDGE ( 'NONE', *, *, #35156, .T. ) ;
#15946 = ORIENTED_EDGE ( 'NONE', *, *, #26719, .T. ) ;
#15947 = VECTOR ( 'NONE', #5683, 1000.000000000000227 ) ;
#15948 = PLANE ( 'NONE',  #5062 ) ;
#15949 = VECTOR ( 'NONE', #18883, 1000.000000000000227 ) ;
#15950 = PLANE ( 'NONE',  #38405 ) ;
#15951 = EDGE_LOOP ( 'NONE', ( #48093, #40040, #53256, #47611 ) ) ;
#15952 = FACE_OUTER_BOUND ( 'NONE', #29651, .T. ) ;
#15953 = EDGE_CURVE ( 'NONE', #31401, #26710, #40061, .T. ) ;
#15954 = AXIS2_PLACEMENT_3D ( 'NONE', #26391, #44002, #31788 ) ;
#15955 = ORIENTED_EDGE ( 'NONE', *, *, #20596, .T. ) ;
#15956 = CARTESIAN_POINT ( 'NONE',  ( -16.26477430435274130, 0.000000000000000000, 4.524504877465088448 ) ) ;
#15957 = VECTOR ( 'NONE', #28927, 1000.000000000000114 ) ;
#15958 = AXIS2_PLACEMENT_3D ( 'NONE', #37860, #11720, #29036 ) ;
#15959 = ORIENTED_EDGE ( 'NONE', *, *, #12120, .T. ) ;
#15960 = ORIENTED_EDGE ( 'NONE', *, *, #17011, .T. ) ;
#15961 = ORIENTED_EDGE ( 'NONE', *, *, #21161, .F. ) ;
#15962 = LINE ( 'NONE', #37245, #9362 ) ;
#15963 = PLANE ( 'NONE',  #22360 ) ;
#15964 = FACE_OUTER_BOUND ( 'NONE', #10963, .T. ) ;
#15965 = AXIS2_PLACEMENT_3D ( 'NONE', #30563, #52950, #39053 ) ;
#15966 = EDGE_CURVE ( 'NONE', #47675, #16451, #5707, .T. ) ;
#15967 = ORIENTED_EDGE ( 'NONE', *, *, #18408, .T. ) ;
#15968 = VECTOR ( 'NONE', #14185, 1000.000000000000114 ) ;
#15969 = DIRECTION ( 'NONE',  ( -0.7660212471507179544, -0.6427876096865405842, -0.005961354470445141482 ) ) ;
#15970 = ORIENTED_EDGE ( 'NONE', *, *, #23243, .T. ) ;
#15971 = ADVANCED_FACE ( 'NONE', ( #52564 ), #13660, .F. ) ;
#15972 = EDGE_CURVE ( 'NONE', #31317, #33602, #39221, .T. ) ;
#15973 = VECTOR ( 'NONE', #53464, 1000.000000000000000 ) ;
#15974 = ORIENTED_EDGE ( 'NONE', *, *, #27525, .T. ) ;
#15975 = VECTOR ( 'NONE', #15786, 1000.000000000000114 ) ;
#15976 = EDGE_LOOP ( 'NONE', ( #14622, #46732, #7728, #23830, #1142 ) ) ;
#15977 = LINE ( 'NONE', #38689, #44962 ) ;
#15978 = CARTESIAN_POINT ( 'NONE',  ( -15.56267859057018121, 0.000000000000000000, 8.023283390499960532 ) ) ;
#15979 = VERTEX_POINT ( 'NONE', #5436 ) ;
#15980 = PLANE ( 'NONE',  #51119 ) ;
#15981 = ADVANCED_FACE ( 'NONE', ( #18794 ), #35827, .F. ) ;
#15982 = ORIENTED_EDGE ( 'NONE', *, *, #30523, .T. ) ;
#15983 = FACE_OUTER_BOUND ( 'NONE', #41462, .T. ) ;
#15984 = CARTESIAN_POINT ( 'NONE',  ( -11.40636015113596180, 0.000000000000000000, 11.32142374880780089 ) ) ;
#15985 = ORIENTED_EDGE ( 'NONE', *, *, #42815, .F. ) ;
#15986 = ADVANCED_FACE ( 'NONE', ( #14258 ), #30454, .F. ) ;
#15987 = DIRECTION ( 'NONE',  ( -0.6427681459581293666, -0.7660444431189770143, -0.005002170337467561935 ) ) ;
#15988 = EDGE_LOOP ( 'NONE', ( #42781, #28738, #34162 ) ) ;
#15989 = ADVANCED_FACE ( 'NONE', ( #9126 ), #36113, .F. ) ;
#15990 = VECTOR ( 'NONE', #31804, 1000.000000000000227 ) ;
#15991 = CARTESIAN_POINT ( 'NONE',  ( -31.72704407542318350, -0.1191753592594197858, 9.105487798182664960 ) ) ;
#15992 = LINE ( 'NONE', #54050, #8453 ) ;
#15993 = CARTESIAN_POINT ( 'NONE',  ( -17.26532721389163072, 0.000000000000000000, 13.67648636611514590 ) ) ;
#15994 = DIRECTION ( 'NONE',  ( -0.7660212471507179544, -0.6427876096865405842, -0.005961354470445141482 ) ) ;
#15995 = CARTESIAN_POINT ( 'NONE',  ( -16.75745944145380406, 4.172053068839010059, 10.23753730508299142 ) ) ;
#15996 = LINE ( 'NONE', #2631, #35543 ) ;
#15997 = VECTOR ( 'NONE', #43198, 1000.000000000000227 ) ;
#15998 = ORIENTED_EDGE ( 'NONE', *, *, #28197, .T. ) ;
#15999 = ADVANCED_FACE ( 'NONE', ( #8878 ), #316, .F. ) ;
#16000 = ORIENTED_EDGE ( 'NONE', *, *, #11359, .T. ) ;
#16001 = DIRECTION ( 'NONE',  ( 0.5364919789714477361, 0.6444004775717706579, 0.5449076811759711036 ) ) ;
#16002 = VECTOR ( 'NONE', #4631, 999.9999999999998863 ) ;
#16003 = CARTESIAN_POINT ( 'NONE',  ( -21.47341775636118655, -0.1191753592594197858, 5.122631121243466090 ) ) ;
#16004 = CARTESIAN_POINT ( 'NONE',  ( -67.62088067883519216, 0.1329945644841871721, 2.681528892132510222 ) ) ;
#16005 = DIRECTION ( 'NONE',  ( 0.2113248654051873565, 0.7886751345948121994, -0.5773502691896263972 ) ) ;
#16006 = DIRECTION ( 'NONE',  ( -0.005961354470445682716, -0.6427876096865404731, 0.7660212471507180654 ) ) ;
#16007 = EDGE_CURVE ( 'NONE', #39014, #30987, #5176, .T. ) ;
#16008 = VECTOR ( 'NONE', #3909, 999.9999999999998863 ) ;
#16009 = CARTESIAN_POINT ( 'NONE',  ( -32.65841372305263235, 0.000000000000000000, 9.367568705923016381 ) ) ;
#16010 = VERTEX_POINT ( 'NONE', #26438 ) ;
#16011 = FACE_OUTER_BOUND ( 'NONE', #8413, .T. ) ;
#16012 = DIRECTION ( 'NONE',  ( 0.000000000000000000, 0.000000000000000000, 1.000000000000000000 ) ) ;
#16013 = ORIENTED_EDGE ( 'NONE', *, *, #36568, .F. ) ;
#16014 = LINE ( 'NONE', #19414, #28398 ) ;
#16015 = CARTESIAN_POINT ( 'NONE',  ( -18.68717756098156713, -0.1191753592594176070, 4.405650147085642843 ) ) ;
#16016 = ORIENTED_EDGE ( 'NONE', *, *, #54015, .T. ) ;
#16017 = CARTESIAN_POINT ( 'NONE',  ( -70.45024891871291572, 2.000000000000000000, 8.217082732571151737 ) ) ;
#16018 = B_SPLINE_CURVE_WITH_KNOTS ( 'NONE', 3,
 ( #35618, #23663, #49796, #50635, #2369, #20231, #11727, #40984 ),
 .UNSPECIFIED., .F., .F.,
 ( 4, 2, 2, 4 ),
 ( 4.827458356132498828E-16, 0.0004770940840306632427, 0.0009541881680608437985, 0.001908376336121245459 ),
 .UNSPECIFIED. ) ;
#16019 = DIRECTION ( 'NONE',  ( -0.6427681459581293666, -0.7660444431189770143, -0.005002170337467561935 ) ) ;
#16020 = VECTOR ( 'NONE', #43842, 1000.000000000000114 ) ;
#16021 = CARTESIAN_POINT ( 'NONE',  ( -11.20636620717317378, 0.000000000000000000, 11.32298014792380414 ) ) ;
#16022 = CARTESIAN_POINT ( 'NONE',  ( -14.00280974873554030, 0.000000000000000000, 12.40921378708904044 ) ) ;
#16023 = AXIS2_PLACEMENT_3D ( 'NONE', #28313, #6749, #24072 ) ;
#16024 = CARTESIAN_POINT ( 'NONE',  ( -19.12962290826653700, 0.000000000000000000, 14.40064212555863854 ) ) ;
#16025 = EDGE_LOOP ( 'NONE', ( #49086, #3467, #30591, #10701 ) ) ;
#16026 = AXIS2_PLACEMENT_3D ( 'NONE', #50652, #50908, #37884 ) ;
#16027 = ORIENTED_EDGE ( 'NONE', *, *, #13717, .T. ) ;
#16028 = FACE_OUTER_BOUND ( 'NONE', #14641, .T. ) ;
#16029 = CARTESIAN_POINT ( 'NONE',  ( 5.585384566839274534, -1.054099306315943396, 2.341018106606942428 ) ) ;
#16030 = CARTESIAN_POINT ( 'NONE',  ( -16.81267852042391198, -0.1191753592594197858, 3.312241722634738039 ) ) ;
#16031 = LINE ( 'NONE', #33606, #10653 ) ;
#16032 = LINE ( 'NONE', #28814, #11937 ) ;
#16033 = CARTESIAN_POINT ( 'NONE',  ( -22.40478740399063895, 0.000000000000000000, 5.384712028983816623 ) ) ;
#16034 = EDGE_CURVE ( 'NONE', #52765, #42667, #22195, .T. ) ;
#16035 = EDGE_LOOP ( 'NONE', ( #2522, #55916, #1601, #16719 ) ) ;
#16036 = FACE_OUTER_BOUND ( 'NONE', #12665, .T. ) ;
#16037 = VECTOR ( 'NONE', #40662, 1000.000000000000000 ) ;
#16038 = LINE ( 'NONE', #19988, #2405 ) ;
#16039 = FACE_OUTER_BOUND ( 'NONE', #18147, .T. ) ;
#16040 = ORIENTED_EDGE ( 'NONE', *, *, #27250, .T. ) ;
#16041 = DIRECTION ( 'NONE',  ( 0.000000000000000000, -1.000000000000000000, 0.000000000000000000 ) ) ;
#16042 = PLANE ( 'NONE',  #3246 ) ;
#16043 = CARTESIAN_POINT ( 'NONE',  ( -13.71629766702752562, -5.213152330870663320, 10.56547866312180339 ) ) ;
#16044 = EDGE_LOOP ( 'NONE', ( #42074, #14927, #20416, #40092 ) ) ;
#16045 = CARTESIAN_POINT ( 'NONE',  ( -17.93139508144814442, 0.000000000000000000, 13.85596890686001537 ) ) ;
#16046 = VECTOR ( 'NONE', #46122, 1000.000000000000227 ) ;
#16047 = ORIENTED_EDGE ( 'NONE', *, *, #39003, .T. ) ;
#16048 = ADVANCED_FACE ( 'NONE', ( #35269 ), #48292, .F. ) ;
#16049 = ORIENTED_EDGE ( 'NONE', *, *, #42701, .F. ) ;
#16050 = AXIS2_PLACEMENT_3D ( 'NONE', #44558, #22458, #46957 ) ;
#16051 = ORIENTED_EDGE ( 'NONE', *, *, #42193, .F. ) ;
#16052 = VERTEX_POINT ( 'NONE', #18195 ) ;
#16053 = PLANE ( 'NONE',  #2103 ) ;
#16054 = ORIENTED_EDGE ( 'NONE', *, *, #23216, .F. ) ;
#16055 = CIRCLE ( 'NONE', #8818, 2.000000000000001776 ) ;
#16056 = ORIENTED_EDGE ( 'NONE', *, *, #52128, .F. ) ;
#16057 = DIRECTION ( 'NONE',  ( 0.005002170337468016433, -0.7660444431189770143, -0.6427681459581293666 ) ) ;
#16058 = EDGE_CURVE ( 'NONE', #9638, #11120, #27025, .T. ) ;
#16059 = ORIENTED_EDGE ( 'NONE', *, *, #34070, .T. ) ;
#16060 = ORIENTED_EDGE ( 'NONE', *, *, #3462, .T. ) ;
#16061 = ADVANCED_FACE ( 'NONE', ( #9715 ), #41479, .F. ) ;
#16062 = AXIS2_PLACEMENT_3D ( 'NONE', #14488, #14228, #9681 ) ;
#16063 = LINE ( 'NONE', #42167, #10373 ) ;
#16064 = DIRECTION ( 'NONE',  ( -0.6246952433987894571, 0.7422098413412802076, 0.2426528472758539834 ) ) ;
#16065 = FACE_OUTER_BOUND ( 'NONE', #16550, .T. ) ;
#16066 = FACE_OUTER_BOUND ( 'NONE', #47999, .T. ) ;
#16067 = ORIENTED_EDGE ( 'NONE', *, *, #16736, .T. ) ;
#16068 = EDGE_CURVE ( 'NONE', #43321, #48873, #19315, .T. ) ;
#16069 = VERTEX_POINT ( 'NONE', #15602 ) ;
#16070 = CARTESIAN_POINT ( 'NONE',  ( -8.207176806059445440, 0.000000000000000000, 5.864533187340529530 ) ) ;
#16071 = CARTESIAN_POINT ( 'NONE',  ( -13.68844308129014564, 0.000000000000000000, 6.021882761988201160 ) ) ;
#16072 = DIRECTION ( 'NONE',  ( 0.007781995580012663651, 0.000000000000000000, -0.9999697198139515519 ) ) ;
#16073 = EDGE_CURVE ( 'NONE', #10456, #17295, #19043, .T. ) ;
#16074 = CARTESIAN_POINT ( 'NONE',  ( 2.072287782118878319, 0.000000000000000000, -2.950529333540147015 ) ) ;
#16075 = CARTESIAN_POINT ( 'NONE',  ( -13.27065584551087163, 0.000000000000000000, 12.04557950825129176 ) ) ;
#16076 = DIRECTION ( 'NONE',  ( 0.9999697198139515519, 0.000000000000000000, 0.007781995580013368816 ) ) ;
#16077 = VERTEX_POINT ( 'NONE', #32118 ) ;
#16078 = DIRECTION ( 'NONE',  ( -0.6427681459581293666, -0.7660444431189770143, -0.005002170337467561935 ) ) ;
#16079 = EDGE_LOOP ( 'NONE', ( #13688, #2422, #43692, #5542 ) ) ;
#16080 = FACE_OUTER_BOUND ( 'NONE', #33039, .T. ) ;
#16081 = DIRECTION ( 'NONE',  ( 0.007781995580012663651, 0.000000000000000000, -0.9999697198139515519 ) ) ;
#16082 = DIRECTION ( 'NONE',  ( 0.5449076811759707706, 0.6444004775717708799, -0.5364919789714476250 ) ) ;
#16083 = DIRECTION ( 'NONE',  ( 0.000000000000000000, -0.000000000000000000, -1.000000000000000000 ) ) ;
#16084 = DIRECTION ( 'NONE',  ( 0.007781995580012662783, 0.000000000000000000, -0.9999697198139514409 ) ) ;
#16085 = LINE ( 'NONE', #54680, #15975 ) ;
#16086 = VECTOR ( 'NONE', #42490, 1000.000000000000227 ) ;
#16087 = ORIENTED_EDGE ( 'NONE', *, *, #25360, .T. ) ;
#16088 = ORIENTED_EDGE ( 'NONE', *, *, #1356, .T. ) ;
#16089 = LINE ( 'NONE', #15256, #5809 ) ;
#16090 = DIRECTION ( 'NONE',  ( 0.5449076811759707706, 0.6444004775717708799, -0.5364919789714476250 ) ) ;
#16091 = DIRECTION ( 'NONE',  ( 0.9999697198139515519, 0.000000000000000000, 0.007781995580013368816 ) ) ;
#16092 = EDGE_CURVE ( 'NONE', #14416, #16426, #46017, .T. ) ;
#16093 = VECTOR ( 'NONE', #34247, 1000.000000000000114 ) ;
#16094 = LINE ( 'NONE', #32834, #12844 ) ;
#16095 = DIRECTION ( 'NONE',  ( 0.007781995580012663651, 0.000000000000000000, -0.9999697198139515519 ) ) ;
#16096 = ADVANCED_FACE ( 'NONE', ( #24415 ), #36658, .F. ) ;
#16097 = LINE ( 'NONE', #46177, #29091 ) ;
#16098 = DIRECTION ( 'NONE',  ( -0.6246952433987894571, 0.7422098413412802076, 0.2426528472758539834 ) ) ;
#16099 = DIRECTION ( 'NONE',  ( 0.005002170337468016433, -0.7660444431189770143, -0.6427681459581293666 ) ) ;
#16100 = ADVANCED_FACE ( 'NONE', ( #53968 ), #2816, .F. ) ;
#16101 = DIRECTION ( 'NONE',  ( 0.5449076811759707706, 0.6444004775717708799, -0.5364919789714476250 ) ) ;
#16102 = ORIENTED_EDGE ( 'NONE', *, *, #3841, .F. ) ;
#16103 = EDGE_CURVE ( 'NONE', #3799, #39923, #2559, .T. ) ;
#16104 = ADVANCED_FACE ( 'NONE', ( #19617 ), #10557, .F. ) ;
#16105 = EDGE_CURVE ( 'NONE', #8484, #12293, #28122, .T. ) ;
#16106 = ORIENTED_EDGE ( 'NONE', *, *, #1876, .F. ) ;
#16107 = EDGE_LOOP ( 'NONE', ( #37545, #55397, #28056, #50976 ) ) ;
#16108 = ORIENTED_EDGE ( 'NONE', *, *, #19215, .F. ) ;
#16109 = ORIENTED_EDGE ( 'NONE', *, *, #23738, .T. ) ;
#16110 = ORIENTED_EDGE ( 'NONE', *, *, #24347, .F. ) ;
#16111 = LINE ( 'NONE', #33431, #6952 ) ;
#16112 = PLANE ( 'NONE',  #18407 ) ;
#16113 = FACE_OUTER_BOUND ( 'NONE', #2997, .T. ) ;
#16114 = VERTEX_POINT ( 'NONE', #32940 ) ;
#16115 = DIRECTION ( 'NONE',  ( 0.005002170337468016433, -0.7660444431189770143, -0.6427681459581293666 ) ) ;
#16116 = EDGE_CURVE ( 'NONE', #48743, #33120, #40901, .T. ) ;
#16117 = ORIENTED_EDGE ( 'NONE', *, *, #22696, .T. ) ;
#16118 = CARTESIAN_POINT ( 'NONE',  ( -64.95503971932161846, -11.15637352545318706, 3.244935472806012022 ) ) ;
#16119 = ORIENTED_EDGE ( 'NONE', *, *, #12662, .F. ) ;
#16120 = EDGE_CURVE ( 'NONE', #22349, #32717, #3502, .T. ) ;
#16121 = AXIS2_PLACEMENT_3D ( 'NONE', #17561, #52209, #13324 ) ;
#16122 = CARTESIAN_POINT ( 'NONE',  ( -66.67188136048933700, -8.735183455216070314, -1.700609907707529400 ) ) ;
#16123 = EDGE_CURVE ( 'NONE', #51745, #18836, #20142, .T. ) ;
#16124 = FACE_OUTER_BOUND ( 'NONE', #41594, .T. ) ;
#16125 = DIRECTION ( 'NONE',  ( -0.6427681459581293666, -0.7660444431189770143, -0.005002170337467561935 ) ) ;
#16126 = ORIENTED_EDGE ( 'NONE', *, *, #5419, .F. ) ;
#16127 = CARTESIAN_POINT ( 'NONE',  ( -9.110551994824897193, 0.000000000000000000, 3.538847790438064411 ) ) ;
#16128 = VERTEX_POINT ( 'NONE', #23331 ) ;
#16129 = ADVANCED_FACE ( 'NONE', ( #36365 ), #40646, .F. ) ;
#16130 = VECTOR ( 'NONE', #21384, 1000.000000000000114 ) ;
#16131 = DIRECTION ( 'NONE',  ( -0.9999697198139514409, -0.000000000000000000, -0.007781995580013368816 ) ) ;
#16132 = DIRECTION ( 'NONE',  ( -0.5364919789714478471, 0.6444004775717705469, -0.5449076811759709926 ) ) ;
#16133 = DIRECTION ( 'NONE',  ( 0.5364919789714477361, 0.6444004775717706579, 0.5449076811759711036 ) ) ;
#16134 = DIRECTION ( 'NONE',  ( 0.005002170337468016433, -0.7660444431189770143, -0.6427681459581293666 ) ) ;
#16135 = LINE ( 'NONE', #33451, #31242 ) ;
#16136 = DIRECTION ( 'NONE',  ( 0.007781995580012662783, 0.000000000000000000, -0.9999697198139514409 ) ) ;
#16137 = DIRECTION ( 'NONE',  ( 0.9999697198139515519, 0.000000000000000000, 0.007781995580013368816 ) ) ;
#16138 = CARTESIAN_POINT ( 'NONE',  ( 2.072287782118878319, 0.000000000000000000, -2.950529333540147015 ) ) ;
#16139 = ORIENTED_EDGE ( 'NONE', *, *, #25618, .T. ) ;
#16140 = DIRECTION ( 'NONE',  ( -0.005002170337468016433, -0.7660444431189770143, 0.6427681459581293666 ) ) ;
#16141 = EDGE_LOOP ( 'NONE', ( #11521, #5922, #54281, #2908, #49070 ) ) ;
#16142 = PLANE ( 'NONE',  #6608 ) ;
#16143 = DIRECTION ( 'NONE',  ( -0.005002170337468016433, -0.7660444431189770143, 0.6427681459581293666 ) ) ;
#16144 = PLANE ( 'NONE',  #53143 ) ;
#16145 = DIRECTION ( 'NONE',  ( -0.005002170337468016433, -0.7660444431189770143, 0.6427681459581293666 ) ) ;
#16146 = CARTESIAN_POINT ( 'NONE',  ( -18.29747203306047609, -0.1191753592594177458, 14.03778604627889059 ) ) ;
#16147 = CARTESIAN_POINT ( 'NONE',  ( -16.89925026227929195, -0.1191753592594197858, 13.49466922669627422 ) ) ;
#16148 = ORIENTED_EDGE ( 'NONE', *, *, #18745, .T. ) ;
#16149 = CARTESIAN_POINT ( 'NONE',  ( -14.66887761629205222, 0.000000000000000000, 12.58869632783390990 ) ) ;
#16150 = DIRECTION ( 'NONE',  ( -0.3583679495452925523, -0.9335804264972047406, -0.000000000000000000 ) ) ;
#16151 = FACE_OUTER_BOUND ( 'NONE', #38000, .T. ) ;
#16152 = DIRECTION ( 'NONE',  ( 0.007781995580012662783, 0.000000000000000000, -0.9999697198139514409 ) ) ;
#16153 = LINE ( 'NONE', #49930, #36862 ) ;
#16154 = DIRECTION ( 'NONE',  ( 0.000000000000000000, -0.000000000000000000, -1.000000000000000000 ) ) ;
#16155 = DIRECTION ( 'NONE',  ( 0.9999697198139515519, 0.000000000000000000, 0.007781995580013368816 ) ) ;
#16156 = CARTESIAN_POINT ( 'NONE',  ( -21.47419595591918906, 0.000000000000000000, 5.222628093224860102 ) ) ;
#16157 = PLANE ( 'NONE',  #17458 ) ;
#16158 = ORIENTED_EDGE ( 'NONE', *, *, #35191, .F. ) ;
#16159 = DIRECTION ( 'NONE',  ( 0.9999697198139515519, 0.000000000000000000, 0.007781995580013368816 ) ) ;
#16160 = DIRECTION ( 'NONE',  ( -0.000000000000000000, 0.000000000000000000, -1.000000000000000000 ) ) ;
#16161 = ORIENTED_EDGE ( 'NONE', *, *, #38681, .F. ) ;
#16162 = ORIENTED_EDGE ( 'NONE', *, *, #5655, .F. ) ;
#16163 = CARTESIAN_POINT ( 'NONE',  ( -24.27063949748155380, 0.000000000000000000, 6.308861732390097288 ) ) ;
#16164 = EDGE_CURVE ( 'NONE', #39726, #20170, #6836, .T. ) ;
#16165 = EDGE_CURVE ( 'NONE', #32592, #28407, #24160, .T. ) ;
#16166 = VECTOR ( 'NONE', #25860, 1000.000000000000000 ) ;
#16167 = ORIENTED_EDGE ( 'NONE', *, *, #173, .F. ) ;
#16168 = ORIENTED_EDGE ( 'NONE', *, *, #41803, .F. ) ;
#16169 = DIRECTION ( 'NONE',  ( 0.6427681459581294776, -0.7660444431189769032, 0.005002170337467562802 ) ) ;
#16170 = ADVANCED_FACE ( 'NONE', ( #44895 ), #1717, .F. ) ;
#16171 = EDGE_LOOP ( 'NONE', ( #50562, #27604, #20436, #9850 ) ) ;
#16172 = ORIENTED_EDGE ( 'NONE', *, *, #45511, .T. ) ;
#16173 = ORIENTED_EDGE ( 'NONE', *, *, #26618, .F. ) ;
#16174 = PLANE ( 'NONE',  #31132 ) ;
#16175 = DIRECTION ( 'NONE',  ( 0.6427681459581294776, -0.7660444431189769032, 0.005002170337467562802 ) ) ;
#16176 = CARTESIAN_POINT ( 'NONE',  ( -10.84028925556084388, -0.1191753592594197858, 11.14116300850493246 ) ) ;
#16177 = ORIENTED_EDGE ( 'NONE', *, *, #28616, .T. ) ;
#16178 = ORIENTED_EDGE ( 'NONE', *, *, #52405, .T. ) ;
#16179 = ADVANCED_FACE ( 'NONE', ( #55355 ), #46263, .F. ) ;
#16180 = CARTESIAN_POINT ( 'NONE',  ( -20.54204810873173415, 0.000000000000000000, 4.860550213503115558 ) ) ;
#16181 = CARTESIAN_POINT ( 'NONE',  ( -20.54049170961573267, 0.000000000000000000, 4.660556269540326646 ) ) ;
#16182 = ORIENTED_EDGE ( 'NONE', *, *, #34736, .F. ) ;
#16183 = EDGE_CURVE ( 'NONE', #44937, #29422, #37784, .T. ) ;
#16184 = DIRECTION ( 'NONE',  ( 0.005961354470445682716, -0.6427876096865404731, -0.7660212471507180654 ) ) ;
#16185 = ORIENTED_EDGE ( 'NONE', *, *, #27727, .F. ) ;
#16186 = DIRECTION ( 'NONE',  ( 0.000000000000000000, -0.000000000000000000, -1.000000000000000000 ) ) ;
#16187 = DIRECTION ( 'NONE',  ( -0.9321478471874540261, 0.000000000000000000, 0.3620778797217457656 ) ) ;
#16188 = ORIENTED_EDGE ( 'NONE', *, *, #25767, .F. ) ;
#16189 = EDGE_CURVE ( 'NONE', #16632, #23911, #46549, .T. ) ;
#16190 = CARTESIAN_POINT ( 'NONE',  ( -24.26908309836554878, 0.000000000000000000, 6.108867788427308376 ) ) ;
#16191 = ADVANCED_FACE ( 'NONE', ( #3674 ), #54795, .F. ) ;
#16192 = DIRECTION ( 'NONE',  ( 0.9999697198139515519, 0.000000000000000000, 0.007781995580013368816 ) ) ;
#16193 = EDGE_LOOP ( 'NONE', ( #43696, #36961, #26419, #47109 ) ) ;
#16194 = DIRECTION ( 'NONE',  ( -0.5449076811759708816, 0.6444004775717707689, 0.5364919789714475140 ) ) ;
#16195 = CARTESIAN_POINT ( 'NONE',  ( -0.9975486161969306931, 4.078988103069860038, 3.605855335088290925 ) ) ;
#16196 = CARTESIAN_POINT ( 'NONE',  ( -23.33771345073609638, -0.1191753592594197858, 5.846786880686956955 ) ) ;
#16197 = ADVANCED_FACE ( 'NONE', ( #42012 ), #16448, .F. ) ;
#16198 = EDGE_LOOP ( 'NONE', ( #27332, #49885, #55378, #8777 ) ) ;
#16199 = VECTOR ( 'NONE', #39262, 1000.000000000000227 ) ;
#16200 = CARTESIAN_POINT ( 'NONE',  ( -15.80145506190093130, 0.000000000000000000, 4.697436548528074240 ) ) ;
#16201 = LINE ( 'NONE', #29251, #44123 ) ;
#16202 = EDGE_CURVE ( 'NONE', #17993, #24549, #3112, .T. ) ;
#16203 = CARTESIAN_POINT ( 'NONE',  ( -55.17209868701984732, 6.284443032133043339, -0.3805810627426228776 ) ) ;
#16204 = PLANE ( 'NONE',  #8725 ) ;
#16205 = LINE ( 'NONE', #24708, #41261 ) ;
#16206 = LINE ( 'NONE', #3133, #3477 ) ;
#16207 = CARTESIAN_POINT ( 'NONE',  ( -69.07439616956314410, -9.749369762244352700, -7.034467916848615943 ) ) ;
#16208 = ORIENTED_EDGE ( 'NONE', *, *, #28803, .T. ) ;
#16209 = LINE ( 'NONE', #38068, #3554 ) ;
#16210 = CARTESIAN_POINT ( 'NONE',  ( -19.75809492754008900, 2.229229656569007290, 8.214581822483392415 ) ) ;
#16211 = LINE ( 'NONE', #46885, #40499 ) ;
#16212 = EDGE_LOOP ( 'NONE', ( #43106, #52290, #22978, #14088 ) ) ;
#16213 = DIRECTION ( 'NONE',  ( 0.007781995580012662783, 0.000000000000000000, -0.9999697198139514409 ) ) ;
#16214 = CARTESIAN_POINT ( 'NONE',  ( -12.15271748404464880, 0.000000000000000000, 1.601849296007406664 ) ) ;
#16215 = CARTESIAN_POINT ( 'NONE',  ( -14.06264638353402141, 5.467268677019013978, 1.969906661245985457 ) ) ;
#16216 = PLANE ( 'NONE',  #55059 ) ;
#16217 = CARTESIAN_POINT ( 'NONE',  ( -24.96676581047183063, 18.24370688441070953, 4.565775410814726598 ) ) ;
#16218 = ORIENTED_EDGE ( 'NONE', *, *, #6200, .T. ) ;
#16219 = ORIENTED_EDGE ( 'NONE', *, *, #12901, .F. ) ;
#16220 = LINE ( 'NONE', #33819, #8714 ) ;
#16221 = LINE ( 'NONE', #25312, #28429 ) ;
#16222 = EDGE_CURVE ( 'NONE', #15181, #17295, #33775, .T. ) ;
#16223 = ORIENTED_EDGE ( 'NONE', *, *, #11433, .F. ) ;
#16224 = LINE ( 'NONE', #25314, #55778 ) ;
#16225 = ORIENTED_EDGE ( 'NONE', *, *, #24040, .F. ) ;
#16226 = LINE ( 'NONE', #2864, #44695 ) ;
#16227 = ADVANCED_FACE ( 'NONE', ( #15905 ), #30856, .F. ) ;
#16228 = ADVANCED_FACE ( 'NONE', ( #35150 ), #46858, .F. ) ;
#16229 = ORIENTED_EDGE ( 'NONE', *, *, #54546, .T. ) ;
#16230 = ORIENTED_EDGE ( 'NONE', *, *, #13229, .T. ) ;
#16231 = ORIENTED_EDGE ( 'NONE', *, *, #31592, .T. ) ;
#16232 = DIRECTION ( 'NONE',  ( -0.005002170337468016433, -0.7660444431189770143, 0.6427681459581293666 ) ) ;
#16233 = FACE_OUTER_BOUND ( 'NONE', #33818, .T. ) ;
#16234 = CARTESIAN_POINT ( 'NONE',  ( -10.40149616133915345, 0.000000000000000000, 1.615477705271093800 ) ) ;
#16235 = COLOUR_RGB ( '', 0.09019608, 0.27058824, 0.51372549) ;
#16236 = CARTESIAN_POINT ( 'NONE',  ( -14.46888367232926420, 0.000000000000000000, 12.59025272694991315 ) ) ;
#16237 = ORIENTED_EDGE ( 'NONE', *, *, #26059, .T. ) ;
#16238 = EDGE_LOOP ( 'NONE', ( #45089, #55752, #15903, #23568 ) ) ;
#16239 = ORIENTED_EDGE ( 'NONE', *, *, #5337, .T. ) ;
#16240 = CARTESIAN_POINT ( 'NONE',  ( -10.00813838035478298, 0.000000000000000000, 10.77830692922518452 ) ) ;
#16241 = LINE ( 'NONE', #20785, #43964 ) ;
#16242 = ORIENTED_EDGE ( 'NONE', *, *, #6459, .F. ) ;
#16243 = DIRECTION ( 'NONE',  ( 0.005002170337468016433, -0.7660444431189770143, -0.6427681459581293666 ) ) ;
#16244 = ORIENTED_EDGE ( 'NONE', *, *, #23325, .T. ) ;
#16245 = DIRECTION ( 'NONE',  ( 0.9659258262890692004, -0.2588190451025176864, 0.000000000000000000 ) ) ;
#16246 = CARTESIAN_POINT ( 'NONE',  ( -18.76354595665420177, -0.1191753592594177458, 14.21882498613976331 ) ) ;
#16247 = ORIENTED_EDGE ( 'NONE', *, *, #26889, .F. ) ;
#16248 = DIRECTION ( 'NONE',  ( -0.5364919789714478471, 0.6444004775717705469, -0.5449076811759709926 ) ) ;
#16249 = ORIENTED_EDGE ( 'NONE', *, *, #38708, .F. ) ;
#16250 = ADVANCED_FACE ( 'NONE', ( #20445 ), #7371, .F. ) ;
#16251 = CARTESIAN_POINT ( 'NONE',  ( -8.844954222421781864, 0.000000000000000000, 6.428907982042063374 ) ) ;
#16252 = CARTESIAN_POINT ( 'NONE',  ( -8.932676780824044371, -0.1191753592594177180, 4.850893997471606767 ) ) ;
#16253 = EDGE_CURVE ( 'NONE', #47896, #55726, #30606, .T. ) ;
#16254 =( BOUNDED_CURVE ( )  B_SPLINE_CURVE ( 3, ( #1857, #27429, #27739, #44758 ),
 .UNSPECIFIED., .F., .F. ) 
 B_SPLINE_CURVE_WITH_KNOTS ( ( 4, 4 ),
 ( 1.140403016137406356, 2.754752525938840790 ),
 .UNSPECIFIED. ) 
 CURVE ( )  GEOMETRIC_REPRESENTATION_ITEM ( )  RATIONAL_B_SPLINE_CURVE ( ( 1.000000000000000000, 0.7943613114863616875, 0.7943613114863616875, 1.000000000000000000 ) ) 
 REPRESENTATION_ITEM ( '' )  );
#16255 = DIRECTION ( 'NONE',  ( 0.005002170337468016433, -0.7660444431189770143, -0.6427681459581293666 ) ) ;
#16256 = FACE_OUTER_BOUND ( 'NONE', #7071, .T. ) ;
#16257 = LINE ( 'NONE', #38399, #6522 ) ;
#16258 = APPLICATION_CONTEXT ( 'automotive_design' ) ;
#16259 = ORIENTED_EDGE ( 'NONE', *, *, #48083, .F. ) ;
#16260 = ORIENTED_EDGE ( 'NONE', *, *, #4556, .F. ) ;
#16261 = CARTESIAN_POINT ( 'NONE',  ( -62.23823698199102950, 6.658783344088819334, 5.000000000000000000 ) ) ;
#16262 = EDGE_CURVE ( 'NONE', #15067, #14438, #42317, .T. ) ;
#16263 = LINE ( 'NONE', #50048, #50232 ) ;
#16264 = CARTESIAN_POINT ( 'NONE',  ( -68.25801324219597177, 0.1329745449598424278, 4.605078063924990417 ) ) ;
#16265 = CARTESIAN_POINT ( 'NONE',  ( -21.53432988685325356, 2.714935509636508204, 4.959976111460639103 ) ) ;
#16266 = CARTESIAN_POINT ( 'NONE',  ( -12.60458797795435615, 0.000000000000000000, 11.86609696750642229 ) ) ;
#16267 = DIRECTION ( 'NONE',  ( -0.7660212471507179544, -0.6427876096865405842, -0.005961354470445141482 ) ) ;
#16268 = VERTEX_POINT ( 'NONE', #52445 ) ;
#16269 = CARTESIAN_POINT ( 'NONE',  ( -10.00813838035478298, 0.000000000000000000, 10.77830692922518452 ) ) ;
#16270 = FACE_OUTER_BOUND ( 'NONE', #20219, .T. ) ;
#16271 = ORIENTED_EDGE ( 'NONE', *, *, #27733, .T. ) ;
#16272 = FACE_OUTER_BOUND ( 'NONE', #43754, .T. ) ;
#16273 = ORIENTED_EDGE ( 'NONE', *, *, #10965, .T. ) ;
#16274 = LINE ( 'NONE', #34443, #47051 ) ;
#16275 = DIRECTION ( 'NONE',  ( 0.000000000000000000, 0.000000000000000000, 1.000000000000000000 ) ) ;
#16276 = CARTESIAN_POINT ( 'NONE',  ( -18.62819553763212710, 0.000000000000000000, 9.676761164233743884 ) ) ;
#16277 = ADVANCED_FACE ( 'NONE', ( #4734 ), #25276, .F. ) ;
#16278 = DIRECTION ( 'NONE',  ( 0.007781995580012663651, 0.000000000000000000, -0.9999697198139515519 ) ) ;
#16279 = CARTESIAN_POINT ( 'NONE',  ( -67.56998338746467425, 1.999999999999990452, 7.586268967162788535 ) ) ;
#16280 = ORIENTED_EDGE ( 'NONE', *, *, #31297, .F. ) ;
#16281 = ORIENTED_EDGE ( 'NONE', *, *, #3465, .F. ) ;
#16282 = LINE ( 'NONE', #33603, #14929 ) ;
#16283 = CARTESIAN_POINT ( 'NONE',  ( -22.02718324817240969, 19.65220053346460816, -4.407437592157546824 ) ) ;
#16284 = DIRECTION ( 'NONE',  ( -0.9999697198139514409, -0.000000000000000000, -0.007781995580013368816 ) ) ;
#16285 = EDGE_CURVE ( 'NONE', #43426, #41524, #28968, .T. ) ;
#16286 = FACE_OUTER_BOUND ( 'NONE', #15740, .T. ) ;
#16287 = DIRECTION ( 'NONE',  ( -0.5364919789714478471, 0.6444004775717705469, -0.5449076811759709926 ) ) ;
#16288 = ADVANCED_FACE ( 'NONE', ( #34847 ), #13279, .F. ) ;
#16289 = CARTESIAN_POINT ( 'NONE',  ( -8.460163181381084030, -0.1064616600236961419, 5.213234893987049645 ) ) ;
#16290 = EDGE_LOOP ( 'NONE', ( #47185, #54712, #1755, #36233 ) ) ;
#16291 = DIRECTION ( 'NONE',  ( 0.000000000000000000, -1.000000000000000000, 0.000000000000000000 ) ) ;
#16292 = EDGE_CURVE ( 'NONE', #10480, #40212, #43911, .T. ) ;
#16293 = CARTESIAN_POINT ( 'NONE',  ( -11.59440027503052129, 3.038739411681507185, 6.372068998963611897 ) ) ;
#16294 = CARTESIAN_POINT ( 'NONE',  ( 2.072287782118878319, 0.000000000000000000, -2.950529333540147015 ) ) ;
#16295 = VERTEX_POINT ( 'NONE', #45316 ) ;
#16296 = CARTESIAN_POINT ( 'NONE',  ( 2.072287782118878319, 0.000000000000000000, -2.950529333540147015 ) ) ;
#16297 = CARTESIAN_POINT ( 'NONE',  ( -17.74482636761137044, -0.1191753592594197858, 3.674319602356483916 ) ) ;
#16298 = CARTESIAN_POINT ( 'NONE',  ( -58.00000000000000711, 8.000000000000000000, 7.102951435054649637E-15 ) ) ;
#16299 = EDGE_CURVE ( 'NONE', #19103, #31662, #10116, .T. ) ;
#16300 = EDGE_LOOP ( 'NONE', ( #49502, #38230, #16419, #1595 ) ) ;
#16301 = EDGE_CURVE ( 'NONE', #41698, #31162, #40526, .T. ) ;
#16302 = CARTESIAN_POINT ( 'NONE',  ( -22.40478740399063895, 0.000000000000000000, 5.384712028983816623 ) ) ;
#16303 = ORIENTED_EDGE ( 'NONE', *, *, #45150, .T. ) ;
#16304 = EDGE_CURVE ( 'NONE', #40075, #51697, #27428, .T. ) ;
#16305 = VERTEX_POINT ( 'NONE', #1607 ) ;
#16306 = ORIENTED_EDGE ( 'NONE', *, *, #31634, .T. ) ;
#16307 = EDGE_LOOP ( 'NONE', ( #17911, #39298, #18042, #4271 ) ) ;
#16308 = LINE ( 'NONE', #11215, #22956 ) ;
#16309 = ORIENTED_EDGE ( 'NONE', *, *, #38562, .F. ) ;
#16310 = DIRECTION ( 'NONE',  ( -0.005961354470445682716, -0.6427876096865404731, 0.7660212471507180654 ) ) ;
#16311 = ORIENTED_EDGE ( 'NONE', *, *, #52884, .F. ) ;
#16312 = FACE_OUTER_BOUND ( 'NONE', #26538, .T. ) ;
#16313 = ORIENTED_EDGE ( 'NONE', *, *, #2556, .T. ) ;
#16314 = VERTEX_POINT ( 'NONE', #14117 ) ;
#16315 = CARTESIAN_POINT ( 'NONE',  ( -15.33837456417585088, 0.000000000000000000, 4.901046404258871725 ) ) ;
#16316 = CARTESIAN_POINT ( 'NONE',  ( -9.408809891686260585, -0.1191753592594168437, 6.324516898734651171 ) ) ;
#16317 = LINE ( 'NONE', #11229, #9530 ) ;
#16318 = PLANE ( 'NONE',  #18739 ) ;
#16319 = LINE ( 'NONE', #50953, #26516 ) ;
#16320 = ORIENTED_EDGE ( 'NONE', *, *, #29886, .T. ) ;
#16321 = ORIENTED_EDGE ( 'NONE', *, *, #41190, .T. ) ;
#16322 = CARTESIAN_POINT ( 'NONE',  ( -9.195139935026407585, 2.581774180789586648, 3.321081197191737555 ) ) ;
#16323 = EDGE_CURVE ( 'NONE', #13662, #53459, #20896, .T. ) ;
#16324 = DIRECTION ( 'NONE',  ( -0.9999697198139514409, -0.000000000000000000, -0.007781995580013368816 ) ) ;
#16325 = LINE ( 'NONE', #55807, #46904 ) ;
#16326 = PLANE ( 'NONE',  #42142 ) ;
#16327 = CARTESIAN_POINT ( 'NONE',  ( -27.06552663992790997, 0.000000000000000000, 7.195101427592543786 ) ) ;
#16328 = CARTESIAN_POINT ( 'NONE',  ( -29.86352658060627618, 0.000000000000000000, 8.481329010720569883 ) ) ;
#16329 = VERTEX_POINT ( 'NONE', #53552 ) ;
#16330 = CARTESIAN_POINT ( 'NONE',  ( -15.32687835015472011, 0.000000000000000000, 3.423807591227812530 ) ) ;
#16331 = DIRECTION ( 'NONE',  ( -0.9999697198139514409, -0.000000000000000000, -0.007781995580013368816 ) ) ;
#16332 = ORIENTED_EDGE ( 'NONE', *, *, #42982, .T. ) ;
#16333 = ADVANCED_FACE ( 'NONE', ( #22364 ), #49016, .F. ) ;
#16334 = CARTESIAN_POINT ( 'NONE',  ( -12.80458192191714595, 0.000000000000000000, 11.86454056839041726 ) ) ;
#16335 = LINE ( 'NONE', #46163, #35079 ) ;
#16336 = DIRECTION ( 'NONE',  ( 0.000000000000000000, -1.000000000000000000, 0.000000000000000000 ) ) ;
#16337 = DIRECTION ( 'NONE',  ( 0.9999697198139515519, 0.000000000000000000, 0.007781995580013368816 ) ) ;
#16338 = ADVANCED_FACE ( 'NONE', ( #18078 ), #49297, .T. ) ;
#16339 = EDGE_CURVE ( 'NONE', #43960, #12251, #1856, .T. ) ;
#16340 = DIRECTION ( 'NONE',  ( -0.5364919789714478471, 0.6444004775717705469, -0.5449076811759709926 ) ) ;
#16341 = VECTOR ( 'NONE', #10099, 999.9999999999998863 ) ;
#16342 = ORIENTED_EDGE ( 'NONE', *, *, #53909, .T. ) ;
#16343 = VERTEX_POINT ( 'NONE', #10411 ) ;
#16344 = CARTESIAN_POINT ( 'NONE',  ( -30.79411802867772607, 0.000000000000000000, 8.643412946479525516 ) ) ;
#16345 = DIRECTION ( 'NONE',  ( -0.005002170337468016433, -0.7660444431189770143, 0.6427681459581293666 ) ) ;
#16346 = DIRECTION ( 'NONE',  ( 0.005961354470445682716, -0.6427876096865404731, -0.7660212471507180654 ) ) ;
#16347 = FACE_OUTER_BOUND ( 'NONE', #36949, .T. ) ;
#16348 = ADVANCED_FACE ( 'NONE', ( #39933 ), #48457, .F. ) ;
#16349 = FACE_OUTER_BOUND ( 'NONE', #3190, .T. ) ;
#16350 = CARTESIAN_POINT ( 'NONE',  ( -21.98208829179906232, -3.432230869623159819, 10.85339692575916537 ) ) ;
#16351 = DIRECTION ( 'NONE',  ( 0.9999697198139515519, 0.000000000000000000, 0.007781995580013368816 ) ) ;
#16352 = ADVANCED_FACE ( 'NONE', ( #26899 ), #23470, .F. ) ;
#16353 = CARTESIAN_POINT ( 'NONE',  ( -11.30636317915456779, -0.1191753592594197858, 11.32220194836580340 ) ) ;
#16354 = DIRECTION ( 'NONE',  ( -0.005961354470445682716, -0.6427876096865404731, 0.7660212471507180654 ) ) ;
#16355 = CARTESIAN_POINT ( 'NONE',  ( -13.73672976910459909, 0.000000000000000000, 12.22661844811216270 ) ) ;
#16356 = VERTEX_POINT ( 'NONE', #36511 ) ;
#16357 = CARTESIAN_POINT ( 'NONE',  ( -20.23219776430595829, -4.727446477803164626, 4.589363523624652608 ) ) ;
#16358 = ADVANCED_FACE ( 'NONE', ( #9858 ), #40221, .F. ) ;
#16359 = ORIENTED_EDGE ( 'NONE', *, *, #11210, .T. ) ;
#16360 = ORIENTED_EDGE ( 'NONE', *, *, #4325, .F. ) ;
#16361 = EDGE_CURVE ( 'NONE', #39727, #42260, #1307, .T. ) ;
#16362 = ORIENTED_EDGE ( 'NONE', *, *, #16464, .F. ) ;
#16363 = ORIENTED_EDGE ( 'NONE', *, *, #54763, .F. ) ;
#16364 = ORIENTED_EDGE ( 'NONE', *, *, #7197, .F. ) ;
#16365 = ORIENTED_EDGE ( 'NONE', *, *, #2551, .T. ) ;
#16366 = CARTESIAN_POINT ( 'NONE',  ( -31.72704407542318350, -0.1191753592594197858, 9.105487798182664960 ) ) ;
#16367 = CARTESIAN_POINT ( 'NONE',  ( -28.93137873341882127, 0.000000000000000000, 8.119251130998824451 ) ) ;
#16368 = CARTESIAN_POINT ( 'NONE',  ( -23.33693525117809386, 0.000000000000000000, 5.746789908705562944 ) ) ;
#16369 = AXIS2_PLACEMENT_3D ( 'NONE', #25000, #33513, #37483 ) ;
#16370 = VERTEX_POINT ( 'NONE', #32277 ) ;
#16371 = PLANE ( 'NONE',  #45811 ) ;
#16372 = ORIENTED_EDGE ( 'NONE', *, *, #17932, .F. ) ;
#16373 = PLANE ( 'NONE',  #1404 ) ;
#16374 = VERTEX_POINT ( 'NONE', #49598 ) ;
#16375 = AXIS2_PLACEMENT_3D ( 'NONE', #55124, #25563, #41753 ) ;
#16376 = CARTESIAN_POINT ( 'NONE',  ( -65.38876380835138491, -9.193003266854505640, -3.032880804691990395 ) ) ;
#16377 = CARTESIAN_POINT ( 'NONE',  ( -19.60990026154428278, 0.000000000000000000, 4.498472333781370125 ) ) ;
#16378 = CARTESIAN_POINT ( 'NONE',  ( -69.23151552270924469, -10.31681141643477773, -7.498719848001563548 ) ) ;
#16379 = ORIENTED_EDGE ( 'NONE', *, *, #38227, .T. ) ;
#16380 = PLANE ( 'NONE',  #44627 ) ;
#16381 = EDGE_CURVE ( 'NONE', #37296, #55481, #28009, .T. ) ;
#16382 = VERTEX_POINT ( 'NONE', #18346 ) ;
#16383 = LINE ( 'NONE', #33709, #47333 ) ;
#16384 = ADVANCED_FACE ( 'NONE', ( #35687 ), #27163, .F. ) ;
#16385 = DIRECTION ( 'NONE',  ( 0.007781995580012663651, -3.146120232559066537E-19, -0.9999697198139514409 ) ) ;
#16386 = FACE_OUTER_BOUND ( 'NONE', #41236, .T. ) ;
#16387 = EDGE_CURVE ( 'NONE', #41466, #24940, #10947, .T. ) ;
#16388 = DIRECTION ( 'NONE',  ( 0.005002170337468016433, -0.7660444431189770143, -0.6427681459581293666 ) ) ;
#16389 = DIRECTION ( 'NONE',  ( 0.000000000000000000, -1.000000000000000000, 0.000000000000000000 ) ) ;
#16390 = CARTESIAN_POINT ( 'NONE',  ( -10.00813838035478298, 0.000000000000000000, 10.77830692922518452 ) ) ;
#16391 = CARTESIAN_POINT ( 'NONE',  ( -18.69579972149740854, -0.1191753592594173433, 5.513579256858934130 ) ) ;
#16392 = CARTESIAN_POINT ( 'NONE',  ( -8.875996589204540044, 0.000000000000000000, 10.41778544861944233 ) ) ;
#16393 = ORIENTED_EDGE ( 'NONE', *, *, #8880, .T. ) ;
#16394 = CARTESIAN_POINT ( 'NONE',  ( -25.83279121425626812, 17.74370688441070953, 4.657440554554202805 ) ) ;
#16395 = ORIENTED_EDGE ( 'NONE', *, *, #26676, .T. ) ;
#16396 = EDGE_CURVE ( 'NONE', #43993, #8713, #54380, .T. ) ;
#16397 = ADVANCED_FACE ( 'NONE', ( #11228 ), #41607, .F. ) ;
#16398 = EDGE_CURVE ( 'NONE', #33916, #43669, #20608, .T. ) ;
#16399 = VECTOR ( 'NONE', #1713, 1000.000000000000000 ) ;
#16400 = PLANE ( 'NONE',  #55564 ) ;
#16401 = DIRECTION ( 'NONE',  ( -0.005961354470445682716, -0.6427876096865404731, 0.7660212471507180654 ) ) ;
#16402 = CARTESIAN_POINT ( 'NONE',  ( -19.44088468089161026, -1.003701604285655469, 5.880676884387883163 ) ) ;
#16403 = LINE ( 'NONE', #46809, #2249 ) ;
#16404 = DIRECTION ( 'NONE',  ( -0.7660212471507179544, -0.6427876096865405842, -0.005961354470445141482 ) ) ;
#16405 = EDGE_CURVE ( 'NONE', #53889, #44242, #24860, .T. ) ;
#16406 = LINE ( 'NONE', #37426, #6688 ) ;
#16407 = CONTEXT_DEPENDENT_SHAPE_REPRESENTATION ( #13692, #45078 ) ;
#16408 = ORIENTED_EDGE ( 'NONE', *, *, #26064, .F. ) ;
#16409 = CARTESIAN_POINT ( 'NONE',  ( -29.86197018149027116, 0.000000000000000000, 8.281335066757780083 ) ) ;
#16410 = CARTESIAN_POINT ( 'NONE',  ( -11.13274803382162226, 24.49872996416489457, 3.250237613767693823 ) ) ;
#16411 = CARTESIAN_POINT ( 'NONE',  ( -16.94377541268302778, 0.000000000000000000, 6.365881082869898400 ) ) ;
#16412 = DIRECTION ( 'NONE',  ( -0.9999697198139514409, -0.000000000000000000, -0.007781995580013368816 ) ) ;
#16413 = AXIS2_PLACEMENT_3D ( 'NONE', #49665, #6772, #45126 ) ;
#16414 = CARTESIAN_POINT ( 'NONE',  ( -10.14100915727248164, 0.000000000000000000, 7.157485922469027706 ) ) ;
#16415 = ADVANCED_FACE ( 'NONE', ( #28550 ), #32546, .F. ) ;
#16416 = DIRECTION ( 'NONE',  ( 0.005002170337468016433, -0.7660444431189770143, -0.6427681459581293666 ) ) ;
#16417 = CARTESIAN_POINT ( 'NONE',  ( -20.57654483182816918, -1.813211359398158029, 4.816098976698940604 ) ) ;
#16418 = DIRECTION ( 'NONE',  ( 0.9999697198139515519, 0.000000000000000000, 0.007781995580013368816 ) ) ;
#16419 = ORIENTED_EDGE ( 'NONE', *, *, #25838, .T. ) ;
#16420 = AXIS2_PLACEMENT_3D ( 'NONE', #46506, #50521, #24954 ) ;
#16421 = EDGE_CURVE ( 'NONE', #27552, #23390, #29393, .T. ) ;
#16422 = PLANE ( 'NONE',  #2212 ) ;
#16423 = FACE_OUTER_BOUND ( 'NONE', #39356, .T. ) ;
#16424 = ORIENTED_EDGE ( 'NONE', *, *, #49170, .F. ) ;
#16425 = EDGE_CURVE ( 'NONE', #41830, #28682, #11528, .T. ) ;
#16426 = VERTEX_POINT ( 'NONE', #55229 ) ;
#16427 = FACE_OUTER_BOUND ( 'NONE', #52709, .T. ) ;
#16428 = EDGE_CURVE ( 'NONE', #16370, #31087, #29097, .T. ) ;
#16429 = EDGE_LOOP ( 'NONE', ( #51865, #13150, #12701, #17225 ) ) ;
#16430 = ORIENTED_EDGE ( 'NONE', *, *, #31397, .T. ) ;
#16431 = PLANE ( 'NONE',  #14833 ) ;
#16432 = ORIENTED_EDGE ( 'NONE', *, *, #24683, .T. ) ;
#16433 = ORIENTED_EDGE ( 'NONE', *, *, #36359, .T. ) ;
#16434 = ORIENTED_EDGE ( 'NONE', *, *, #30905, .T. ) ;
#16435 = DIRECTION ( 'NONE',  ( -0.6427681459581293666, -0.7660444431189770143, -0.005002170337467561935 ) ) ;
#16436 = DIRECTION ( 'NONE',  ( 0.007781995580012663651, -3.146120232559066537E-19, -0.9999697198139514409 ) ) ;
#16437 = CARTESIAN_POINT ( 'NONE',  ( -16.00719711287428737, 0.000000000000000000, 5.434499555927599701 ) ) ;
#16438 = AXIS2_PLACEMENT_3D ( 'NONE', #3381, #29197, #41694 ) ;
#16439 = VECTOR ( 'NONE', #14723, 999.9999999999998863 ) ;
#16440 = VERTEX_POINT ( 'NONE', #50111 ) ;
#16441 = ORIENTED_EDGE ( 'NONE', *, *, #32645, .T. ) ;
#16442 = DIRECTION ( 'NONE',  ( 0.007781995580012663651, -3.146120232559066537E-19, -0.9999697198139514409 ) ) ;
#16443 = CARTESIAN_POINT ( 'NONE',  ( 2.072287782118878319, 0.000000000000000000, -2.950529333540147015 ) ) ;
#16444 = ORIENTED_EDGE ( 'NONE', *, *, #53364, .F. ) ;
#16445 = FACE_OUTER_BOUND ( 'NONE', #803, .T. ) ;
#16446 = DIRECTION ( 'NONE',  ( 0.007781995580012662783, 0.000000000000000000, -0.9999697198139514409 ) ) ;
#16447 = ORIENTED_EDGE ( 'NONE', *, *, #30736, .F. ) ;
#16448 = PLANE ( 'NONE',  #16715 ) ;
#16449 = PLANE ( 'NONE',  #29448 ) ;
#16450 = EDGE_CURVE ( 'NONE', #29013, #24466, #54649, .T. ) ;
#16451 = VERTEX_POINT ( 'NONE', #6699 ) ;
#16452 = CARTESIAN_POINT ( 'NONE',  ( -19.25070634120488222, 0.000000000000000000, 4.259254523999361552 ) ) ;
#16453 = EDGE_CURVE ( 'NONE', #41032, #24619, #20012, .T. ) ;
#16454 = AXIS2_PLACEMENT_3D ( 'NONE', #15901, #16184, #28120 ) ;
#16455 = LINE ( 'NONE', #33783, #39089 ) ;
#16456 = ORIENTED_EDGE ( 'NONE', *, *, #41617, .F. ) ;
#16457 = LINE ( 'NONE', #1089, #33999 ) ;
#16458 = PLANE ( 'NONE',  #5728 ) ;
#16459 = DIRECTION ( 'NONE',  ( 0.005961354470445682716, -0.6427876096865404731, -0.7660212471507180654 ) ) ;
#16460 = LINE ( 'NONE', #33789, #15616 ) ;
#16461 = ORIENTED_EDGE ( 'NONE', *, *, #718, .F. ) ;
#16462 = EDGE_CURVE ( 'NONE', #31624, #24198, #54963, .T. ) ;
#16463 = EDGE_CURVE ( 'NONE', #21299, #35152, #37337, .T. ) ;
#16464 = EDGE_CURVE ( 'NONE', #44511, #46096, #33099, .T. ) ;
#16465 = CARTESIAN_POINT ( 'NONE',  ( -18.76354595665420177, -0.1191753592594177458, 14.21882498613976331 ) ) ;
#16466 = CARTESIAN_POINT ( 'NONE',  ( -10.21012437789221217, 0.000000000000000000, 2.724963214160391445 ) ) ;
#16467 = DIRECTION ( 'NONE',  ( -0.5449076811759708816, 0.6444004775717707689, 0.5364919789714475140 ) ) ;
#16468 = CARTESIAN_POINT ( 'NONE',  ( -14.94760462649100496, 0.000000000000000000, 2.488088991209854051 ) ) ;
#16469 = EDGE_CURVE ( 'NONE', #53596, #27982, #3274, .T. ) ;
#16470 = DIRECTION ( 'NONE',  ( 0.7660212471507180654, -0.6427876096865404731, 0.005961354470445141482 ) ) ;
#16471 = DIRECTION ( 'NONE',  ( 0.5364919789714477361, 0.6444004775717706579, 0.5449076811759711036 ) ) ;
#16472 = CARTESIAN_POINT ( 'NONE',  ( 2.072287782118878319, 0.000000000000000000, -2.950529333540147015 ) ) ;
#16473 = ORIENTED_EDGE ( 'NONE', *, *, #48624, .T. ) ;
#16474 = SURFACE_STYLE_FILL_AREA ( #34949 ) ;
#16475 = PLANE ( 'NONE',  #2413 ) ;
#16476 = VERTEX_POINT ( 'NONE', #16316 ) ;
#16477 = DIRECTION ( 'NONE',  ( -0.5449076811759708816, 0.6444004775717707689, 0.5364919789714475140 ) ) ;
#16478 = CARTESIAN_POINT ( 'NONE',  ( -17.88038292028693732, -3.594132820645663084, 3.711997409451107455 ) ) ;
#16479 = AXIS2_PLACEMENT_3D ( 'NONE', #12407, #9237, #29735 ) ;
#16480 = VECTOR ( 'NONE', #27361, 999.9999999999998863 ) ;
#16481 = CARTESIAN_POINT ( 'NONE',  ( -19.79569077582305070, 0.000000000000000000, 14.58012466630350445 ) ) ;
#16482 = PLANE ( 'NONE',  #13352 ) ;
#16483 = ADVANCED_FACE ( 'NONE', ( #33635 ), #50949, .F. ) ;
#16484 = LINE ( 'NONE', #20486, #25638 ) ;
#16485 = ORIENTED_EDGE ( 'NONE', *, *, #1085, .F. ) ;
#16486 = VECTOR ( 'NONE', #40150, 999.9999999999998863 ) ;
#16487 = EDGE_LOOP ( 'NONE', ( #12559, #7411, #25415, #39860 ) ) ;
#16488 = ADVANCED_FACE ( 'NONE', ( #23726 ), #2139, .F. ) ;
#16489 = CARTESIAN_POINT ( 'NONE',  ( -12.10028655381466578, 0.000000000000000000, 6.772906302923760613 ) ) ;
#16490 = CARTESIAN_POINT ( 'NONE',  ( -25.84533184003709039, 17.69690463183794193, -4.605409455127198015 ) ) ;
#16491 = ORIENTED_EDGE ( 'NONE', *, *, #10402, .T. ) ;
#16492 = CARTESIAN_POINT ( 'NONE',  ( -9.876320842032628278, -0.1191753592594181482, 6.690210690224407841 ) ) ;
#16493 = EDGE_CURVE ( 'NONE', #54483, #38787, #15477, .T. ) ;
#16494 = ORIENTED_EDGE ( 'NONE', *, *, #52345, .T. ) ;
#16495 = LINE ( 'NONE', #24458, #53993 ) ;
#16496 = AXIS2_PLACEMENT_3D ( 'NONE', #38544, #12445, #43089 ) ;
#16497 = VERTEX_POINT ( 'NONE', #17437 ) ;
#16498 = CARTESIAN_POINT ( 'NONE',  ( -15.03495456790438389, -0.1191753592594197858, 12.77051346725278158 ) ) ;
#16499 = EDGE_CURVE ( 'NONE', #43061, #23916, #12908, .T. ) ;
#16500 = VECTOR ( 'NONE', #43086, 1000.000000000000227 ) ;
#16501 = ORIENTED_EDGE ( 'NONE', *, *, #45209, .T. ) ;
#16502 = VERTEX_POINT ( 'NONE', #51798 ) ;
#16503 = ORIENTED_EDGE ( 'NONE', *, *, #53331, .F. ) ;
#16504 = LINE ( 'NONE', #4576, #10304 ) ;
#16505 = DIRECTION ( 'NONE',  ( -0.7660212471507179544, -0.6427876096865405842, -0.005961354470445141482 ) ) ;
#16506 = CARTESIAN_POINT ( 'NONE',  ( -13.88852388610687250, 1.905425754524005200, 5.403223730618197607 ) ) ;
#16507 = PLANE ( 'NONE',  #10231 ) ;
#16508 = ORIENTED_EDGE ( 'NONE', *, *, #37671, .F. ) ;
#16509 = EDGE_LOOP ( 'NONE', ( #867, #9634, #1377, #16792 ) ) ;
#16510 = EDGE_LOOP ( 'NONE', ( #19452, #8003, #37825, #37098 ) ) ;
#16511 = DIRECTION ( 'NONE',  ( -0.5449076811759708816, 0.6444004775717707689, 0.5364919789714475140 ) ) ;
#16512 = LINE ( 'NONE', #24760, #24920 ) ;
#16513 = EDGE_LOOP ( 'NONE', ( #31563, #8852, #32722, #48708 ) ) ;
#16514 = VECTOR ( 'NONE', #28653, 999.9999999999998863 ) ;
#16515 = CARTESIAN_POINT ( 'NONE',  ( -12.82965364628315719, 0.1245042932765029059, 1.661432565772024361 ) ) ;
#16516 = ORIENTED_EDGE ( 'NONE', *, *, #15159, .T. ) ;
#16517 = DIRECTION ( 'NONE',  ( 0.005002170337468016433, -0.7660444431189770143, -0.6427681459581293666 ) ) ;
#16518 = DIRECTION ( 'NONE',  ( 0.9999697198139515519, 0.000000000000000000, 0.007781995580013368816 ) ) ;
#16519 = AXIS2_PLACEMENT_3D ( 'NONE', #2934, #11754, #36777 ) ;
#16520 = VECTOR ( 'NONE', #27035, 1000.000000000000227 ) ;
#16521 = ORIENTED_EDGE ( 'NONE', *, *, #29536, .F. ) ;
#16522 = CARTESIAN_POINT ( 'NONE',  ( -17.20554431205604828, 0.000000000000000000, 5.994511866960127833 ) ) ;
#16523 = VERTEX_POINT ( 'NONE', #25687 ) ;
#16524 = VECTOR ( 'NONE', #21817, 999.9999999999998863 ) ;
#16525 = DIRECTION ( 'NONE',  ( -0.5449076811759708816, 0.6444004775717707689, 0.5364919789714475140 ) ) ;
#16526 = DIRECTION ( 'NONE',  ( -0.005002170337468016433, -0.7660444431189770143, 0.6427681459581293666 ) ) ;
#16527 = AXIS2_PLACEMENT_3D ( 'NONE', #15617, #42026, #23871 ) ;
#16528 = ORIENTED_EDGE ( 'NONE', *, *, #42472, .F. ) ;
#16529 = PLANE ( 'NONE',  #48593 ) ;
#16530 = FACE_OUTER_BOUND ( 'NONE', #4536, .T. ) ;
#16531 = CARTESIAN_POINT ( 'NONE',  ( -17.32200740551113327, -0.1191753592594158168, 8.109594914967312107 ) ) ;
#16532 = LINE ( 'NONE', #11456, #22857 ) ;
#16533 = ORIENTED_EDGE ( 'NONE', *, *, #24889, .T. ) ;
#16534 = EDGE_CURVE ( 'NONE', #42137, #25299, #47256, .T. ) ;
#16535 = ORIENTED_EDGE ( 'NONE', *, *, #43197, .T. ) ;
#16536 = DIRECTION ( 'NONE',  ( 0.9999697198139515519, 0.000000000000000000, 0.007781995580013368816 ) ) ;
#16537 = PLANE ( 'NONE',  #30355 ) ;
#16538 = VECTOR ( 'NONE', #22827, 999.9999999999998863 ) ;
#16539 = DIRECTION ( 'NONE',  ( -0.9999697198139514409, -0.000000000000000000, -0.007781995580013368816 ) ) ;
#16540 = EDGE_CURVE ( 'NONE', #593, #24779, #55495, .T. ) ;
#16541 = EDGE_CURVE ( 'NONE', #10709, #50934, #16907, .T. ) ;
#16542 = LINE ( 'NONE', #6634, #29427 ) ;
#16543 = FACE_OUTER_BOUND ( 'NONE', #55024, .T. ) ;
#16544 = LINE ( 'NONE', #24788, #55767 ) ;
#16545 = ORIENTED_EDGE ( 'NONE', *, *, #36954, .T. ) ;
#16546 = DIRECTION ( 'NONE',  ( -0.6427681459581293666, -0.7660444431189770143, -0.005002170337467561935 ) ) ;
#16547 = DIRECTION ( 'NONE',  ( 0.007781995580012663651, -3.146120232559066537E-19, -0.9999697198139514409 ) ) ;
#16548 = ORIENTED_EDGE ( 'NONE', *, *, #40899, .F. ) ;
#16549 = DIRECTION ( 'NONE',  ( -0.6427681459581293666, -0.7660444431189770143, -0.005002170337467561935 ) ) ;
#16550 = EDGE_LOOP ( 'NONE', ( #1010, #46002, #7287, #55995 ) ) ;
#16551 = CARTESIAN_POINT ( 'NONE',  ( -23.34675887425330743, 18.98665486385284495, -4.490845947935475202 ) ) ;
#16552 = CARTESIAN_POINT ( 'NONE',  ( -16.79925329029790149, 0.000000000000000000, 13.49544742625427496 ) ) ;
#16553 = CARTESIAN_POINT ( 'NONE',  ( -19.60990026154428278, 0.000000000000000000, 4.498472333781370125 ) ) ;
#16554 = AXIS2_PLACEMENT_3D ( 'NONE', #16149, #24950, #7332 ) ;
#16555 = FACE_OUTER_BOUND ( 'NONE', #11823, .T. ) ;
#16556 = CARTESIAN_POINT ( 'NONE',  ( -68.39906907640694556, 2.000000000000000000, -8.694190345976133827 ) ) ;
#16557 = VERTEX_POINT ( 'NONE', #43012 ) ;
#16558 = EDGE_LOOP ( 'NONE', ( #18082, #55705, #45299, #49447 ) ) ;
#16559 = DIRECTION ( 'NONE',  ( -0.005961354470445682716, -0.6427876096865404731, 0.7660212471507180654 ) ) ;
#16560 = LINE ( 'NONE', #24518, #43115 ) ;
#16561 = AXIS2_PLACEMENT_3D ( 'NONE', #11194, #15728, #23979 ) ;
#16562 = PLANE ( 'NONE',  #36049 ) ;
#16563 = AXIS2_PLACEMENT_3D ( 'NONE', #14694, #23502, #15514 ) ;
#16564 = LINE ( 'NONE', #46374, #17894 ) ;
#16565 = AXIS2_PLACEMENT_3D ( 'NONE', #37416, #54201, #11854 ) ;
#16566 = PLANE ( 'NONE',  #36472 ) ;
#16567 = CARTESIAN_POINT ( 'NONE',  ( -21.47419595591918906, 0.000000000000000000, 5.222628093224860102 ) ) ;
#16568 = ORIENTED_EDGE ( 'NONE', *, *, #52068, .F. ) ;
#16569 = DIRECTION ( 'NONE',  ( 0.007781995580012662783, 0.000000000000000000, -0.9999697198139514409 ) ) ;
#16570 = ADVANCED_FACE ( 'NONE', ( #34239 ), #13482, .F. ) ;
#16571 = DIRECTION ( 'NONE',  ( 0.005961354470445682716, -0.6427876096865404731, -0.7660212471507180654 ) ) ;
#16572 = VECTOR ( 'NONE', #34743, 1000.000000000000000 ) ;
#16573 = LINE ( 'NONE', #32774, #17879 ) ;
#16574 = VECTOR ( 'NONE', #11857, 1000.000000000000227 ) ;
#16575 = ORIENTED_EDGE ( 'NONE', *, *, #39853, .F. ) ;
#16576 = EDGE_CURVE ( 'NONE', #37968, #11293, #21138, .T. ) ;
#16577 = CARTESIAN_POINT ( 'NONE',  ( -14.62700148656139199, -2.460819163488158878, 6.402179327102785145 ) ) ;
#16578 = CARTESIAN_POINT ( 'NONE',  ( -17.73140113748535285, 0.000000000000000000, 13.85752530597602039 ) ) ;
#16579 = DIRECTION ( 'NONE',  ( 0.5364919789714477361, 0.6444004775717706579, 0.5449076811759711036 ) ) ;
#16580 = VERTEX_POINT ( 'NONE', #21981 ) ;
#16581 = CARTESIAN_POINT ( 'NONE',  ( -11.33076995502132256, 0.000000000000000000, 1.608245881735075100 ) ) ;
#16582 = EDGE_CURVE ( 'NONE', #29241, #30062, #4121, .T. ) ;
#16583 = VECTOR ( 'NONE', #26129, 999.9999999999998863 ) ;
#16584 = EDGE_LOOP ( 'NONE', ( #33446, #13041, #52750, #21032 ) ) ;
#16585 = VECTOR ( 'NONE', #54709, 999.9999999999998863 ) ;
#16586 = ORIENTED_EDGE ( 'NONE', *, *, #36974, .T. ) ;
#16587 = EDGE_LOOP ( 'NONE', ( #34902, #26886, #18173, #30353 ) ) ;
#16588 = ORIENTED_EDGE ( 'NONE', *, *, #14823, .T. ) ;
#16589 = CARTESIAN_POINT ( 'NONE',  ( -14.94838282604900748, -0.1191753592594197858, 2.588085963191248506 ) ) ;
#16590 = ORIENTED_EDGE ( 'NONE', *, *, #40754, .F. ) ;
#16591 = AXIS2_PLACEMENT_3D ( 'NONE', #22822, #52637, #14033 ) ;
#16592 = CARTESIAN_POINT ( 'NONE',  ( -26.13493519185646008, 0.000000000000000000, 7.033017491833586377 ) ) ;
#16593 = EDGE_LOOP ( 'NONE', ( #43611, #40346, #40034, #48628 ) ) ;
#16594 = DIRECTION ( 'NONE',  ( -0.6427681459581293666, -0.7660444431189770143, -0.005002170337467561935 ) ) ;
#16595 = ORIENTED_EDGE ( 'NONE', *, *, #50157, .F. ) ;
#16596 = AXIS2_PLACEMENT_3D ( 'NONE', #44630, #5468, #52602 ) ;
#16597 = ORIENTED_EDGE ( 'NONE', *, *, #11490, .T. ) ;
#16598 = CARTESIAN_POINT ( 'NONE',  ( -9.075990533167328067, 0.000000000000000000, 10.41622904950343909 ) ) ;
#16599 = CARTESIAN_POINT ( 'NONE',  ( -13.68269497427957937, 0.000000000000000000, 5.283263355472670675 ) ) ;
#16600 = FACE_OUTER_BOUND ( 'NONE', #12253, .T. ) ;
#16601 = CARTESIAN_POINT ( 'NONE',  ( -18.91005987905199603, 1.257817950434005683, 3.987110198832547248 ) ) ;
#16602 = AXIS2_PLACEMENT_3D ( 'NONE', #21884, #17634, #23311 ) ;
#16603 = EDGE_CURVE ( 'NONE', #27953, #30961, #39311, .T. ) ;
#16604 = CARTESIAN_POINT ( 'NONE',  ( -17.86574470023862560, 0.000000000000000000, 5.420035908855560969 ) ) ;
#16605 = ORIENTED_EDGE ( 'NONE', *, *, #17975, .T. ) ;
#16606 = VECTOR ( 'NONE', #43502, 1000.000000000000114 ) ;
#16607 = VECTOR ( 'NONE', #4682, 999.9999999999998863 ) ;
#16608 = EDGE_CURVE ( 'NONE', #33688, #1588, #38772, .T. ) ;
#16609 = ORIENTED_EDGE ( 'NONE', *, *, #1682, .F. ) ;
#16610 = LINE ( 'NONE', #20866, #34915 ) ;
#16611 = DIRECTION ( 'NONE',  ( 0.005002170337468016433, -0.7660444431189770143, -0.6427681459581293666 ) ) ;
#16612 = UNCERTAINTY_MEASURE_WITH_UNIT (LENGTH_MEASURE( 1.000000000000000082E-05 ), #49682, 'distance_accuracy_value', 'NONE');
#16613 = EDGE_CURVE ( 'NONE', #6528, #9930, #39031, .T. ) ;
#16614 = CARTESIAN_POINT ( 'NONE',  ( -14.02931237854957836, -0.1191753592594187450, 2.964570451734679146 ) ) ;
#16615 = AXIS2_PLACEMENT_3D ( 'NONE', #25321, #9114, #21889 ) ;
#16616 = AXIS2_PLACEMENT_3D ( 'NONE', #32148, #18513, #40387 ) ;
#16617 = PLANE ( 'NONE',  #9621 ) ;
#16618 = LINE ( 'NONE', #29713, #43972 ) ;
#16619 = DIRECTION ( 'NONE',  ( -0.3620778797217457101, 0.000000000000000000, -0.9321478471874540261 ) ) ;
#16620 = ORIENTED_EDGE ( 'NONE', *, *, #21719, .T. ) ;
#16621 = CARTESIAN_POINT ( 'NONE',  ( -15.60102546347950536, 0.000000000000000000, 12.95077420755565356 ) ) ;
#16622 = DIRECTION ( 'NONE',  ( -0.5449076811759708816, 0.6444004775717707689, 0.5364919789714475140 ) ) ;
#16623 = EDGE_LOOP ( 'NONE', ( #49346, #22485, #49113, #8437, #41987 ) ) ;
#16624 = LINE ( 'NONE', #12394, #37011 ) ;
#16625 = DIRECTION ( 'NONE',  ( 0.2426528472758542054, 0.7422098413412800966, 0.6246952433987894571 ) ) ;
#16626 = DIRECTION ( 'NONE',  ( 0.6427681459581294776, -0.7660444431189769032, 0.005002170337467562802 ) ) ;
#16627 = LINE ( 'NONE', #11803, #29559 ) ;
#16628 = VECTOR ( 'NONE', #15467, 1000.000000000000227 ) ;
#16629 = LINE ( 'NONE', #20881, #20473 ) ;
#16630 = EDGE_CURVE ( 'NONE', #866, #15209, #401, .T. ) ;
#16631 = VERTEX_POINT ( 'NONE', #52385 ) ;
#16632 = VERTEX_POINT ( 'NONE', #21721 ) ;
#16633 = LINE ( 'NONE', #37946, #37530 ) ;
#16634 = PLANE ( 'NONE',  #4118 ) ;
#16635 = CARTESIAN_POINT ( 'NONE',  ( -22.40478740399063895, 0.000000000000000000, 5.384712028983816623 ) ) ;
#16636 = AXIS2_PLACEMENT_3D ( 'NONE', #33710, #51026, #29472 ) ;
#16637 = LINE ( 'NONE', #3580, #42746 ) ;
#16638 = CARTESIAN_POINT ( 'NONE',  ( -19.59569683186026268, 0.000000000000000000, 14.58168106541950948 ) ) ;
#16639 = VECTOR ( 'NONE', #1499, 999.9999999999998863 ) ;
#16640 = CARTESIAN_POINT ( 'NONE',  ( -23.33771345073609638, -0.1191753592594197858, 5.846786880686956955 ) ) ;
#16641 = DIRECTION ( 'NONE',  ( 0.005002170337468016433, -0.7660444431189770143, -0.6427681459581293666 ) ) ;
#16642 = CARTESIAN_POINT ( 'NONE',  ( 2.072287782118878319, 0.000000000000000000, -2.950529333540147015 ) ) ;
#16643 = CARTESIAN_POINT ( 'NONE',  ( -69.20821692254106949, -9.630996011957124736, 8.593930712158170948 ) ) ;
#16644 = VECTOR ( 'NONE', #23170, 1000.000000000000000 ) ;
#16645 = DIRECTION ( 'NONE',  ( 0.5364919789714477361, 0.6444004775717706579, 0.5449076811759711036 ) ) ;
#16646 = EDGE_LOOP ( 'NONE', ( #51178, #14945, #5879, #27341 ) ) ;
#16647 = CARTESIAN_POINT ( 'NONE',  ( -60.74376512051347987, 7.691826835550698682, -3.000000000000007105 ) ) ;
#16648 = AXIS2_PLACEMENT_3D ( 'NONE', #11151, #15994, #49789 ) ;
#16649 = AXIS2_PLACEMENT_3D ( 'NONE', #31531, #35777, #48841 ) ;
#16650 = EDGE_LOOP ( 'NONE', ( #42431, #19293, #22002, #9250 ) ) ;
#16651 = EDGE_CURVE ( 'NONE', #55479, #48095, #47846, .T. ) ;
#16652 = ORIENTED_EDGE ( 'NONE', *, *, #52817, .T. ) ;
#16653 = AXIS2_PLACEMENT_3D ( 'NONE', #40509, #40772, #49281 ) ;
#16654 = ORIENTED_EDGE ( 'NONE', *, *, #15634, .T. ) ;
#16655 = EDGE_LOOP ( 'NONE', ( #50646, #50057, #5080, #3435 ) ) ;
#16656 = VECTOR ( 'NONE', #53106, 1000.000000000000000 ) ;
#16657 = ORIENTED_EDGE ( 'NONE', *, *, #8753, .F. ) ;
#16658 = VERTEX_POINT ( 'NONE', #56088 ) ;
#16659 = DIRECTION ( 'NONE',  ( 0.007781995580012662783, 0.000000000000000000, -0.9999697198139514409 ) ) ;
#16660 = LINE ( 'NONE', #16367, #12991 ) ;
#16661 = PLANE ( 'NONE',  #44817 ) ;
#16662 = EDGE_CURVE ( 'NONE', #947, #29012, #17173, .T. ) ;
#16663 = ORIENTED_EDGE ( 'NONE', *, *, #32786, .T. ) ;
#16664 = DIRECTION ( 'NONE',  ( 0.005961354470445682716, -0.6427876096865404731, -0.7660212471507180654 ) ) ;
#16665 = VERTEX_POINT ( 'NONE', #16599 ) ;
#16666 = DIRECTION ( 'NONE',  ( -0.005961354470445682716, -0.6427876096865404731, 0.7660212471507180654 ) ) ;
#16667 = EDGE_CURVE ( 'NONE', #48671, #40111, #33935, .T. ) ;
#16668 = ORIENTED_EDGE ( 'NONE', *, *, #3072, .T. ) ;
#16669 = EDGE_CURVE ( 'NONE', #19391, #26974, #17745, .T. ) ;
#16670 = LINE ( 'NONE', #166, #46630 ) ;
#16671 = VECTOR ( 'NONE', #50872, 1000.000000000000227 ) ;
#16672 = DIRECTION ( 'NONE',  ( 0.007781995580012663651, 0.000000000000000000, -0.9999697198139515519 ) ) ;
#16673 = CARTESIAN_POINT ( 'NONE',  ( -11.80977711938882280, 0.000000000000000000, 3.451178486255886302 ) ) ;
#16674 = EDGE_CURVE ( 'NONE', #50886, #43539, #8102, .T. ) ;
#16675 = EDGE_LOOP ( 'NONE', ( #19556, #27255, #56110, #20741 ) ) ;
#16676 = DIRECTION ( 'NONE',  ( 0.7660212471507180654, -0.6427876096865404731, 0.005961354470445141482 ) ) ;
#16677 = AXIS2_PLACEMENT_3D ( 'NONE', #20675, #51337, #25223 ) ;
#16678 = ORIENTED_EDGE ( 'NONE', *, *, #19814, .T. ) ;
#16679 = DIRECTION ( 'NONE',  ( -0.5449076811759708816, 0.6444004775717707689, 0.5364919789714475140 ) ) ;
#16680 = EDGE_CURVE ( 'NONE', #43283, #40959, #29703, .T. ) ;
#16682 = VECTOR ( 'NONE', #31992, 999.9999999999998863 ) ;
#16681 = DIRECTION ( 'NONE',  ( -0.5364919789714478471, 0.6444004775717705469, -0.5449076811759709926 ) ) ;
#16683 = EDGE_CURVE ( 'NONE', #36712, #30417, #53237, .T. ) ;
#16684 = LINE ( 'NONE', #42788, #7883 ) ;
#16685 = B_SPLINE_CURVE_WITH_KNOTS ( 'NONE', 3,
 ( #12232, #43714, #56230, #47993 ),
 .UNSPECIFIED., .F., .F.,
 ( 4, 4 ),
 ( 2.082079450497559408E-05, 0.0003537660668259436916 ),
 .UNSPECIFIED. ) ;
#16686 = CARTESIAN_POINT ( 'NONE',  ( -16.15304353870583043, 4.010151117816509903, 9.737052958454759377 ) ) ;
#16687 = CARTESIAN_POINT ( 'NONE',  ( -27.99767448711536133, 0.000000000000000000, 7.557179307314289218 ) ) ;
#16688 = CARTESIAN_POINT ( 'NONE',  ( -69.59783862807636012, -0.6008070088998225255, -7.493102809087827332 ) ) ;
#16689 = CARTESIAN_POINT ( 'NONE',  ( -15.06930115867626974, 0.000000000000000000, 4.333802269690326447 ) ) ;
#16690 = VECTOR ( 'NONE', #24211, 999.9999999999998863 ) ;
#16691 = DIRECTION ( 'NONE',  ( -0.5364919789714478471, 0.6444004775717705469, -0.5449076811759709926 ) ) ;
#16692 = ORIENTED_EDGE ( 'NONE', *, *, #7329, .T. ) ;
#16693 = PLANE ( 'NONE',  #50121 ) ;
#16694 = VERTEX_POINT ( 'NONE', #4956 ) ;
#16695 = VECTOR ( 'NONE', #47407, 1000.000000000000114 ) ;
#16696 = ADVANCED_FACE ( 'NONE', ( #22824 ), #9206, .F. ) ;
#16697 = DIRECTION ( 'NONE',  ( 0.3313982828793700097, 0.4028455766673916805, 0.8531650599175528704 ) ) ;
#16698 = CARTESIAN_POINT ( 'NONE',  ( -22.29430420027960125, 4.172053068839010947, 5.208686264645241870 ) ) ;
#16699 = LINE ( 'NONE', #34029, #1448 ) ;
#16700 = CARTESIAN_POINT ( 'NONE',  ( -29.86352658060627618, 0.000000000000000000, 8.481329010720569883 ) ) ;
#16701 = CARTESIAN_POINT ( 'NONE',  ( 2.072287782118878319, 0.000000000000000000, -2.950529333540147015 ) ) ;
#16702 = EDGE_CURVE ( 'NONE', #49293, #8255, #13740, .T. ) ;
#16703 = VECTOR ( 'NONE', #39903, 1000.000000000000227 ) ;
#16704 = CARTESIAN_POINT ( 'NONE',  ( -11.67244013076689946, 0.000000000000000000, 11.50401908778467863 ) ) ;
#16705 = VECTOR ( 'NONE', #55529, 999.9999999999998863 ) ;
#16706 = ORIENTED_EDGE ( 'NONE', *, *, #10188, .T. ) ;
#16707 = CARTESIAN_POINT ( 'NONE',  ( -26.95299377262630003, 15.36490682821995257, 4.679584696907975960 ) ) ;
#16708 = DIRECTION ( 'NONE',  ( 0.5364919789714477361, 0.6444004775717706579, 0.5449076811759711036 ) ) ;
#16709 = LINE ( 'NONE', #7335, #7343 ) ;
#16710 = PLANE ( 'NONE',  #54493 ) ;
#16711 = PLANE ( 'NONE',  #46557 ) ;
#16712 = CARTESIAN_POINT ( 'NONE',  ( -19.79569077582305070, 0.000000000000000000, 14.58012466630350445 ) ) ;
#16713 = DIRECTION ( 'NONE',  ( -0.005961354470445682716, -0.6427876096865404731, 0.7660212471507180654 ) ) ;
#16714 = ORIENTED_EDGE ( 'NONE', *, *, #3072, .F. ) ;
#16715 = AXIS2_PLACEMENT_3D ( 'NONE', #11907, #7668, #52161 ) ;
#16716 = CARTESIAN_POINT ( 'NONE',  ( -9.808144436391993182, 0.000000000000000000, 10.77986332834118777 ) ) ;
#16717 = DIRECTION ( 'NONE',  ( 0.5364919789714477361, 0.6444004775717706579, 0.5449076811759711036 ) ) ;
#16718 = ORIENTED_EDGE ( 'NONE', *, *, #12247, .F. ) ;
#16719 = ORIENTED_EDGE ( 'NONE', *, *, #29084, .F. ) ;
#16720 = DIRECTION ( 'NONE',  ( 0.007781995580012663651, 0.000000000000000000, -0.9999697198139515519 ) ) ;
#16721 = VECTOR ( 'NONE', #50892, 999.9999999999998863 ) ;
#16722 = ORIENTED_EDGE ( 'NONE', *, *, #45221, .T. ) ;
#16723 = EDGE_CURVE ( 'NONE', #45033, #16580, #12516, .T. ) ;
#16724 = ORIENTED_EDGE ( 'NONE', *, *, #9429, .F. ) ;
#16725 = EDGE_LOOP ( 'NONE', ( #14149, #46623, #52135, #31198 ) ) ;
#16726 = VECTOR ( 'NONE', #44413, 1000.000000000000227 ) ;
#16727 = ORIENTED_EDGE ( 'NONE', *, *, #44157, .T. ) ;
#16728 = LINE ( 'NONE', #5304, #26592 ) ;
#16729 = VECTOR ( 'NONE', #12118, 999.9999999999998863 ) ;
#16730 = DIRECTION ( 'NONE',  ( 0.005002170337468016433, -0.7660444431189770143, -0.6427681459581293666 ) ) ;
#16731 = CARTESIAN_POINT ( 'NONE',  ( -33.59211796935609584, 0.000000000000000000, 9.929640529607549837 ) ) ;
#16732 = EDGE_CURVE ( 'NONE', #28952, #41133, #18574, .T. ) ;
#16733 = VECTOR ( 'NONE', #11995, 999.9999999999998863 ) ;
#16734 = ORIENTED_EDGE ( 'NONE', *, *, #47373, .T. ) ;
#16735 = ORIENTED_EDGE ( 'NONE', *, *, #8144, .F. ) ;
#16736 = EDGE_CURVE ( 'NONE', #2673, #39913, #27099, .T. ) ;
#16737 = VECTOR ( 'NONE', #35572, 999.9999999999998863 ) ;
#16738 = AXIS2_PLACEMENT_3D ( 'NONE', #38429, #47513, #46667 ) ;
#16739 = CARTESIAN_POINT ( 'NONE',  ( 2.072287782118878319, 0.000000000000000000, -2.950529333540147015 ) ) ;
#16740 = DIRECTION ( 'NONE',  ( -0.7660212471507179544, -0.6427876096865405842, -0.005961354470445141482 ) ) ;
#16741 = ORIENTED_EDGE ( 'NONE', *, *, #49174, .T. ) ;
#16742 = DIRECTION ( 'NONE',  ( 0.9999697198139515519, 0.000000000000000000, 0.007781995580013368816 ) ) ;
#16743 = CARTESIAN_POINT ( 'NONE',  ( -26.13415699229845757, -0.1191753592594197858, 6.933020519852192365 ) ) ;
#16744 = VERTEX_POINT ( 'NONE', #39618 ) ;
#16745 = CARTESIAN_POINT ( 'NONE',  ( -9.283724637715325301, 0.000000000000000000, 3.101504740954174277 ) ) ;
#16746 = EDGE_LOOP ( 'NONE', ( #18200, #51773, #54929, #47387, #23684 ) ) ;
#16747 = FACE_OUTER_BOUND ( 'NONE', #14592, .T. ) ;
#16748 = EDGE_CURVE ( 'NONE', #22478, #47842, #22285, .T. ) ;
#16749 = EDGE_CURVE ( 'NONE', #19901, #37705, #43839, .T. ) ;
#16750 = VECTOR ( 'NONE', #25796, 1000.000000000000000 ) ;
#16751 = DIRECTION ( 'NONE',  ( -0.5364919789714478471, 0.6444004775717705469, -0.5449076811759709926 ) ) ;
#16752 = ORIENTED_EDGE ( 'NONE', *, *, #3159, .T. ) ;
#16753 = DIRECTION ( 'NONE',  ( -0.6427681459581293666, -0.7660444431189770143, -0.005002170337467561935 ) ) ;
#16754 = LINE ( 'NONE', #47709, #17521 ) ;
#16756 = VECTOR ( 'NONE', #28123, 1000.000000000000114 ) ;
#16755 = LINE ( 'NONE', #251, #48435 ) ;
#16757 = DIRECTION ( 'NONE',  ( 0.5364919789714477361, 0.6444004775717706579, 0.5449076811759711036 ) ) ;
#16758 = ORIENTED_EDGE ( 'NONE', *, *, #4706, .F. ) ;
#16759 = VECTOR ( 'NONE', #53168, 1000.000000000000227 ) ;
#16760 = EDGE_CURVE ( 'NONE', #31029, #38002, #40144, .T. ) ;
#16761 = CARTESIAN_POINT ( 'NONE',  ( -21.47419595591918906, 0.000000000000000000, 5.222628093224860102 ) ) ;
#16762 = DIRECTION ( 'NONE',  ( 0.6427681459581294776, -0.7660444431189769032, 0.005002170337467562802 ) ) ;
#16763 = DIRECTION ( 'NONE',  ( 0.007781995580012663651, 0.000000000000000000, -0.9999697198139515519 ) ) ;
#16764 = VECTOR ( 'NONE', #40910, 999.9999999999998863 ) ;
#16765 = DIRECTION ( 'NONE',  ( 0.007781995580012662783, 0.000000000000000000, -0.9999697198139514409 ) ) ;
#16766 = LINE ( 'NONE', #34103, #16779 ) ;
#16767 = DIRECTION ( 'NONE',  ( 0.007781995580012662783, 0.000000000000000000, -0.9999697198139514409 ) ) ;
#16768 = VECTOR ( 'NONE', #44978, 999.9999999999998863 ) ;
#16769 = DIRECTION ( 'NONE',  ( 0.6427681459581294776, -0.7660444431189769032, 0.005002170337467562802 ) ) ;
#16770 = VECTOR ( 'NONE', #11998, 1000.000000000000227 ) ;
#16771 = ORIENTED_EDGE ( 'NONE', *, *, #37714, .T. ) ;
#16772 =( LENGTH_UNIT ( ) NAMED_UNIT ( * ) SI_UNIT ( .MILLI., .METRE. ) );
#16774 = DIRECTION ( 'NONE',  ( 0.007781995580012663651, -3.146120232559066537E-19, -0.9999697198139514409 ) ) ;
#16773 = AXIS2_PLACEMENT_3D ( 'NONE', #31538, #36084, #22998 ) ;
#16775 = ORIENTED_EDGE ( 'NONE', *, *, #15753, .F. ) ;
#16776 = VECTOR ( 'NONE', #14390, 999.9999999999998863 ) ;
#16777 = CARTESIAN_POINT ( 'NONE',  ( -24.26908309836554878, 0.000000000000000000, 6.108867788427308376 ) ) ;
#16778 = LINE ( 'NONE', #16478, #2744 ) ;
#16779 = VECTOR ( 'NONE', #51422, 1000.000000000000227 ) ;
#16780 = DIRECTION ( 'NONE',  ( 0.007781995580012662783, 0.000000000000000000, -0.9999697198139514409 ) ) ;
#16781 = CARTESIAN_POINT ( 'NONE',  ( -29.86352658060627618, 0.000000000000000000, 8.481329010720569883 ) ) ;
#16782 = CARTESIAN_POINT ( 'NONE',  ( -14.22368343527709200, -0.3560938001956543975, 2.394921545183867462 ) ) ;
#16783 = VERTEX_POINT ( 'NONE', #48688 ) ;
#16784 = VECTOR ( 'NONE', #28105, 999.9999999999998863 ) ;
#16785 = VECTOR ( 'NONE', #34787, 999.9999999999998863 ) ;
#16786 = ORIENTED_EDGE ( 'NONE', *, *, #23774, .T. ) ;
#16787 = PLANE ( 'NONE',  #507 ) ;
#16788 = DIRECTION ( 'NONE',  ( -0.6427681459581293666, -0.7660444431189770143, -0.005002170337467561935 ) ) ;
#16789 = ORIENTED_EDGE ( 'NONE', *, *, #50634, .T. ) ;
#16790 = EDGE_CURVE ( 'NONE', #27945, #607, #40448, .T. ) ;
#16791 = CARTESIAN_POINT ( 'NONE',  ( -9.110551994824897193, 0.000000000000000000, 3.538847790438064411 ) ) ;
#16792 = ORIENTED_EDGE ( 'NONE', *, *, #7091, .F. ) ;
#16793 = CARTESIAN_POINT ( 'NONE',  ( -21.93567689722629765, 19.99370688441071309, -4.657437592157546824 ) ) ;
#16794 = EDGE_CURVE ( 'NONE', #27421, #51703, #19113, .T. ) ;
#16795 = VERTEX_POINT ( 'NONE', #18017 ) ;
#16796 = CARTESIAN_POINT ( 'NONE',  ( 2.072287782118878319, 0.000000000000000000, -2.950529333540147015 ) ) ;
#16797 = AXIS2_PLACEMENT_3D ( 'NONE', #41900, #24326, #46437 ) ;
#16798 = ORIENTED_EDGE ( 'NONE', *, *, #39238, .T. ) ;
#16799 = EDGE_LOOP ( 'NONE', ( #34320, #25133, #17466, #37687 ) ) ;
#16800 = EDGE_LOOP ( 'NONE', ( #35353, #43363, #27233, #33173 ) ) ;
#16801 = VECTOR ( 'NONE', #4191, 1000.000000000000000 ) ;
#16802 = EDGE_CURVE ( 'NONE', #33384, #20003, #36440, .T. ) ;
#16803 = CARTESIAN_POINT ( 'NONE',  ( -1.086233639165236964, 0.000000000000000000, -2.796443541562362078 ) ) ;
#16804 = FACE_OUTER_BOUND ( 'NONE', #9413, .T. ) ;
#16805 = VECTOR ( 'NONE', #52106, 1000.000000000000227 ) ;
#16806 = LINE ( 'NONE', #18185, #46590 ) ;
#16807 = ADVANCED_FACE ( 'NONE', ( #5796 ), #44675, .F. ) ;
#16808 = EDGE_CURVE ( 'NONE', #33246, #10129, #5506, .T. ) ;
#16809 = ADVANCED_FACE ( 'NONE', ( #5254 ), #22561, .F. ) ;
#16810 = DIRECTION ( 'NONE',  ( -0.5364919789714478471, 0.6444004775717705469, -0.5449076811759709926 ) ) ;
#16811 = ORIENTED_EDGE ( 'NONE', *, *, #14681, .T. ) ;
#16812 = VECTOR ( 'NONE', #494, 1000.000000000000227 ) ;
#16813 = ORIENTED_EDGE ( 'NONE', *, *, #25159, .T. ) ;
#16814 = ORIENTED_EDGE ( 'NONE', *, *, #36324, .F. ) ;
#16815 = AXIS2_PLACEMENT_3D ( 'NONE', #11716, #50032, #50335 ) ;
#16816 = DIRECTION ( 'NONE',  ( -0.6427681459581293666, -0.7660444431189770143, -0.005002170337467561935 ) ) ;
#16817 = VECTOR ( 'NONE', #17314, 999.9999999999998863 ) ;
#16818 = CARTESIAN_POINT ( 'NONE',  ( -18.90896079192820167, -3.108426967578159061, 9.128272473059206860 ) ) ;
#16819 = ORIENTED_EDGE ( 'NONE', *, *, #43113, .F. ) ;
#16820 = LINE ( 'NONE', #20787, #28459 ) ;
#16821 = ORIENTED_EDGE ( 'NONE', *, *, #47892, .F. ) ;
#16822 = CARTESIAN_POINT ( 'NONE',  ( -8.609916609573598834, 0.000000000000000000, 10.23519010964256637 ) ) ;
#16823 = CARTESIAN_POINT ( 'NONE',  ( -28.92982233430281980, 0.000000000000000000, 7.919257187036034651 ) ) ;
#16824 = VECTOR ( 'NONE', #29188, 999.9999999999998863 ) ;
#16825 = EDGE_LOOP ( 'NONE', ( #24672, #38196, #47473 ) ) ;
#16826 = VECTOR ( 'NONE', #51464, 999.9999999999998863 ) ;
#16827 = CARTESIAN_POINT ( 'NONE',  ( -18.15781053378047716, 0.000000000000000000, 8.941757669486225524 ) ) ;
#16828 = EDGE_CURVE ( 'NONE', #30507, #29147, #14334, .T. ) ;
#16829 = ORIENTED_EDGE ( 'NONE', *, *, #44562, .F. ) ;
#16830 = AXIS2_PLACEMENT_3D ( 'NONE', #53211, #17412, #48076 ) ;
#16831 = ADVANCED_FACE ( 'NONE', ( #27358 ), #36184, .F. ) ;
#16832 = DIRECTION ( 'NONE',  ( -0.005961354470445682716, -0.6427876096865404731, 0.7660212471507180654 ) ) ;
#16833 = VECTOR ( 'NONE', #28992, 1000.000000000000000 ) ;
#16834 = CARTESIAN_POINT ( 'NONE',  ( -58.00000000000000711, 8.000000000000000000, 7.102951435054649637E-15 ) ) ;
#16835 = EDGE_LOOP ( 'NONE', ( #9024, #48517, #11663, #31815 ) ) ;
#16836 = CARTESIAN_POINT ( 'NONE',  ( -20.54204810873173415, 0.000000000000000000, 4.860550213503115558 ) ) ;
#16837 = DIRECTION ( 'NONE',  ( 0.005961354470445682716, -0.6427876096865404731, -0.7660212471507180654 ) ) ;
#16838 = EDGE_CURVE ( 'NONE', #40865, #22139, #19394, .T. ) ;
#16839 = CARTESIAN_POINT ( 'NONE',  ( -50.27554558092695913, 4.209026340267034705, -5.000000000000000000 ) ) ;
#16840 = FACE_OUTER_BOUND ( 'NONE', #20001, .T. ) ;
#16841 = ORIENTED_EDGE ( 'NONE', *, *, #49514, .T. ) ;
#16842 = ADVANCED_FACE ( 'NONE', ( #11150 ), #36736, .F. ) ;
#16843 = DIRECTION ( 'NONE',  ( -0.9999697198139514409, -0.000000000000000000, -0.007781995580013368816 ) ) ;
#16844 = DIRECTION ( 'NONE',  ( 0.5364919789714477361, 0.6444004775717706579, 0.5449076811759711036 ) ) ;
#16845 = DIRECTION ( 'NONE',  ( -0.9999697198139514409, -0.000000000000000000, -0.007781995580013368816 ) ) ;
#16846 = LINE ( 'NONE', #13432, #35841 ) ;
#16847 = ADVANCED_FACE ( 'NONE', ( #32198 ), #27948, .F. ) ;
#16848 = CARTESIAN_POINT ( 'NONE',  ( -27.06630483948590893, -0.1191753592594197858, 7.295098399573937797 ) ) ;
#16849 = VECTOR ( 'NONE', #24730, 999.9999999999998863 ) ;
#16850 = DIRECTION ( 'NONE',  ( 0.9999697198139515519, 0.000000000000000000, 0.007781995580013368816 ) ) ;
#16851 = ORIENTED_EDGE ( 'NONE', *, *, #22781, .F. ) ;
#16852 = FACE_OUTER_BOUND ( 'NONE', #39372, .T. ) ;
#16853 = VECTOR ( 'NONE', #25988, 1000.000000000000227 ) ;
#16854 = DIRECTION ( 'NONE',  ( -0.005961354470445682716, -0.6427876096865404731, 0.7660212471507180654 ) ) ;
#16855 = DIRECTION ( 'NONE',  ( 0.007781995580012662783, 0.000000000000000000, -0.9999697198139514409 ) ) ;
#16856 = EDGE_LOOP ( 'NONE', ( #45716, #6337, #13410, #11155 ) ) ;
#16857 = DIRECTION ( 'NONE',  ( 0.5364919789714477361, 0.6444004775717706579, 0.5449076811759711036 ) ) ;
#16858 = VECTOR ( 'NONE', #35164, 1000.000000000000114 ) ;
#16859 = ORIENTED_EDGE ( 'NONE', *, *, #8213, .T. ) ;
#16860 = DIRECTION ( 'NONE',  ( 0.9999697198139515519, 0.000000000000000000, 0.007781995580013368816 ) ) ;
#16861 = DIRECTION ( 'NONE',  ( 0.000000000000000000, -1.000000000000000000, 0.000000000000000000 ) ) ;
#16862 = VECTOR ( 'NONE', #32137, 1000.000000000000000 ) ;
#16863 = DIRECTION ( 'NONE',  ( -0.9999697198139514409, -0.000000000000000000, -0.007781995580013368816 ) ) ;
#16864 = CARTESIAN_POINT ( 'NONE',  ( -68.44534682279325466, 1.999999999991179056, -5.350280945793637777 ) ) ;
#16865 = ORIENTED_EDGE ( 'NONE', *, *, #40650, .T. ) ;
#16866 = VECTOR ( 'NONE', #47553, 999.9999999999998863 ) ;
#16867 = ORIENTED_EDGE ( 'NONE', *, *, #48786, .F. ) ;
#16868 = CARTESIAN_POINT ( 'NONE',  ( -68.17347556353657012, -0.6006513931709031029, -5.215119943113104561 ) ) ;
#16869 = DIRECTION ( 'NONE',  ( -0.005961354470445682716, -0.6427876096865404731, 0.7660212471507180654 ) ) ;
#16870 = PLANE ( 'NONE',  #22385 ) ;
#16871 = VECTOR ( 'NONE', #39400, 1000.000000000000227 ) ;
#16872 = VECTOR ( 'NONE', #23145, 1000.000000000000114 ) ;
#16873 = LINE ( 'NONE', #11753, #7800 ) ;
#16875 = DIRECTION ( 'NONE',  ( 0.000000000000000000, -1.000000000000000000, 0.000000000000000000 ) ) ;
#16874 = VECTOR ( 'NONE', #46199, 999.9999999999998863 ) ;
#16876 = CARTESIAN_POINT ( 'NONE',  ( -24.73909490984108928, 18.18270265044663603, 4.490773887887535842 ) ) ;
#16877 = ORIENTED_EDGE ( 'NONE', *, *, #47590, .F. ) ;
#16878 = PLANE ( 'NONE',  #13848 ) ;
#16879 = VECTOR ( 'NONE', #34140, 999.9999999999998863 ) ;
#16880 = VECTOR ( 'NONE', #26022, 999.9999999999998863 ) ;
#16881 = CARTESIAN_POINT ( 'NONE',  ( -58.00000000000000711, -9.999999999999998224, 7.102951435054649637E-15 ) ) ;
#16882 = ORIENTED_EDGE ( 'NONE', *, *, #53498, .T. ) ;
#16883 = LINE ( 'NONE', #51523, #52844 ) ;
#16884 = CARTESIAN_POINT ( 'NONE',  ( -13.69706524180599239, 0.000000000000000000, 7.129811871761492448 ) ) ;
#16885 = CARTESIAN_POINT ( 'NONE',  ( -16.86024456217533185, -0.1191753592594181482, 8.482520529993088587 ) ) ;
#16886 = ADVANCED_FACE ( 'NONE', ( #46335 ), #23653, .F. ) ;
#16887 = ADVANCED_FACE ( 'NONE', ( #6624 ), #23938, .F. ) ;
#16888 = VERTEX_POINT ( 'NONE', #54883 ) ;
#16889 = FACE_OUTER_BOUND ( 'NONE', #4395, .T. ) ;
#16890 = VERTEX_POINT ( 'NONE', #3198 ) ;
#16891 = EDGE_CURVE ( 'NONE', #34545, #30649, #24775, .T. ) ;
#16892 = VECTOR ( 'NONE', #28369, 999.9999999999998863 ) ;
#16893 = ORIENTED_EDGE ( 'NONE', *, *, #38278, .F. ) ;
#16894 = ORIENTED_EDGE ( 'NONE', *, *, #20352, .F. ) ;
#16895 = ORIENTED_EDGE ( 'NONE', *, *, #48519, .T. ) ;
#16896 = DIRECTION ( 'NONE',  ( -0.9999697198139514409, -0.000000000000000000, -0.007781995580013368816 ) ) ;
#16897 = VECTOR ( 'NONE', #15183, 1000.000000000000227 ) ;
#16898 = EDGE_LOOP ( 'NONE', ( #25592, #26639, #40530, #14760 ) ) ;
#16899 = FACE_OUTER_BOUND ( 'NONE', #25909, .T. ) ;
#16900 = EDGE_LOOP ( 'NONE', ( #15528, #16951, #8917, #29636 ) ) ;
#16901 = CARTESIAN_POINT ( 'NONE',  ( -18.55978481983513717, -0.5179957512181551094, 4.741301724224929792 ) ) ;
#16902 = ORIENTED_EDGE ( 'NONE', *, *, #38532, .F. ) ;
#16903 = EDGE_LOOP ( 'NONE', ( #18454, #41622, #35195, #27715 ) ) ;
#16904 = EDGE_CURVE ( 'NONE', #21366, #37937, #20532, .T. ) ;
#16905 = VECTOR ( 'NONE', #20391, 1000.000000000000114 ) ;
#16906 = CARTESIAN_POINT ( 'NONE',  ( -14.11415985828438480, 2.714935509636508204, 6.819411824594130422 ) ) ;
#16907 = LINE ( 'NONE', #8668, #8730 ) ;
#16908 = DIRECTION ( 'NONE',  ( 0.5449076811759707706, 0.6444004775717708799, -0.5364919789714476250 ) ) ;
#16909 = DIRECTION ( 'NONE',  ( 0.8660254037844380415, 0.5000000000000011102, 0.000000000000000000 ) ) ;
#16910 = FACE_OUTER_BOUND ( 'NONE', #12881, .T. ) ;
#16911 = ORIENTED_EDGE ( 'NONE', *, *, #15105, .T. ) ;
#16912 = AXIS2_PLACEMENT_3D ( 'NONE', #32380, #49687, #10781 ) ;
#16914 = ORIENTED_EDGE ( 'NONE', *, *, #21281, .F. ) ;
#16913 = ADVANCED_FACE ( 'NONE', ( #19951 ), #15683, .F. ) ;
#16915 = VECTOR ( 'NONE', #8953, 1000.000000000000227 ) ;
#16916 = DIRECTION ( 'NONE',  ( 0.000000000000000000, -1.000000000000000000, 0.000000000000000000 ) ) ;
#16917 = DIRECTION ( 'NONE',  ( -0.7660212471507179544, -0.6427876096865405842, -0.005961354470445141482 ) ) ;
#16918 = EDGE_CURVE ( 'NONE', #6267, #34530, #10638, .T. ) ;
#16919 = VECTOR ( 'NONE', #5089, 1000.000000000000000 ) ;
#16920 = LINE ( 'NONE', #29964, #27904 ) ;
#16921 = VECTOR ( 'NONE', #55748, 999.9999999999998863 ) ;
#16922 = DIRECTION ( 'NONE',  ( 0.000000000000000000, -1.000000000000000000, 0.000000000000000000 ) ) ;
#16923 = ADVANCED_FACE ( 'NONE', ( #46081 ), #7187, .F. ) ;
#16924 = CARTESIAN_POINT ( 'NONE',  ( -16.77330902089484610, 0.9340140483890038148, 3.167454640934507459 ) ) ;
#16925 = DIRECTION ( 'NONE',  ( -0.005961354470445682716, -0.6427876096865404731, 0.7660212471507180654 ) ) ;
#16926 = ORIENTED_EDGE ( 'NONE', *, *, #44490, .F. ) ;
#16927 = CARTESIAN_POINT ( 'NONE',  ( -18.81669326757378613, 0.000000000000000000, 8.197965952086681440 ) ) ;
#16928 = EDGE_CURVE ( 'NONE', #41874, #35555, #33323, .T. ) ;
#16929 = DIRECTION ( 'NONE',  ( -0.005961354470445682716, -0.6427876096865404731, 0.7660212471507180654 ) ) ;
#16930 = ORIENTED_EDGE ( 'NONE', *, *, #14649, .F. ) ;
#16931 = CARTESIAN_POINT ( 'NONE',  ( -11.20636620717317378, 0.000000000000000000, 11.32298014792380414 ) ) ;
#16932 = LINE ( 'NONE', #18036, #36933 ) ;
#16933 = ADVANCED_FACE ( 'NONE', ( #32484 ), #45248, .F. ) ;
#16934 = FACE_OUTER_BOUND ( 'NONE', #10351, .T. ) ;
#16935 = LINE ( 'NONE', #3304, #27751 ) ;
#16936 = VECTOR ( 'NONE', #34628, 999.9999999999998863 ) ;
#16937 = ORIENTED_EDGE ( 'NONE', *, *, #5168, .F. ) ;
#16938 = ORIENTED_EDGE ( 'NONE', *, *, #31704, .F. ) ;
#16939 = LINE ( 'NONE', #12668, #25747 ) ;
#16940 = CARTESIAN_POINT ( 'NONE',  ( -16.43317633868556626, -0.1191753592594197858, 13.31363028683540151 ) ) ;
#16941 = CARTESIAN_POINT ( 'NONE',  ( -19.60990026154428278, 0.000000000000000000, 4.498472333781370125 ) ) ;
#16942 = FACE_OUTER_BOUND ( 'NONE', #33704, .T. ) ;
#16943 = VECTOR ( 'NONE', #18055, 1000.000000000000227 ) ;
#16944 = CARTESIAN_POINT ( 'NONE',  ( -10.66745676860673342, 0.000000000000000000, 1.782733951914063031 ) ) ;
#16945 = DIRECTION ( 'NONE',  ( -0.9999697198139514409, -0.000000000000000000, -0.007781995580013368816 ) ) ;
#16946 = DIRECTION ( 'NONE',  ( 0.9999697198139515519, 0.000000000000000000, 0.007781995580013368816 ) ) ;
#16948 = VECTOR ( 'NONE', #47078, 1000.000000000000000 ) ;
#16947 = DIRECTION ( 'NONE',  ( 0.9999697198139515519, 0.000000000000000000, 0.007781995580013368816 ) ) ;
#16949 = CARTESIAN_POINT ( 'NONE',  ( -65.78960443026792859, -9.238969346053028886, -0.1846293804859200915 ) ) ;
#16950 = DIRECTION ( 'NONE',  ( 0.000000000000000000, -0.000000000000000000, -1.000000000000000000 ) ) ;
#16951 = ORIENTED_EDGE ( 'NONE', *, *, #55608, .F. ) ;
#16952 = FACE_OUTER_BOUND ( 'NONE', #10846, .T. ) ;
#16953 = EDGE_CURVE ( 'NONE', #36994, #30666, #50342, .T. ) ;
#16954 = VERTEX_POINT ( 'NONE', #50038 ) ;
#16955 = VECTOR ( 'NONE', #18944, 1000.000000000000227 ) ;
#16956 = EDGE_LOOP ( 'NONE', ( #54643, #38300, #6590, #48856 ) ) ;
#16957 = EDGE_CURVE ( 'NONE', #49949, #40825, #10880, .T. ) ;
#16958 = EDGE_CURVE ( 'NONE', #40111, #21299, #11454, .T. ) ;
#16959 = VERTEX_POINT ( 'NONE', #24235 ) ;
#16960 = AXIS2_PLACEMENT_3D ( 'NONE', #3077, #10787, #6799 ) ;
#16961 = ORIENTED_EDGE ( 'NONE', *, *, #29239, .F. ) ;
#16962 = VERTEX_POINT ( 'NONE', #41546 ) ;
#16963 = ORIENTED_EDGE ( 'NONE', *, *, #46221, .F. ) ;
#16964 = DIRECTION ( 'NONE',  ( -0.3620778797217457656, 0.000000000000000000, -0.9321478471874539151 ) ) ;
#16965 = DIRECTION ( 'NONE',  ( 0.000000000000000000, -1.000000000000000000, 0.000000000000000000 ) ) ;
#16966 = FACE_OUTER_BOUND ( 'NONE', #28438, .T. ) ;
#16967 = EDGE_LOOP ( 'NONE', ( #52498, #1774, #23310, #36248 ) ) ;
#16968 = CARTESIAN_POINT ( 'NONE',  ( -23.33693525117809386, 0.000000000000000000, 5.746789908705562944 ) ) ;
#16969 = VERTEX_POINT ( 'NONE', #47191 ) ;
#16970 = CARTESIAN_POINT ( 'NONE',  ( -64.58804046960723610, -11.11428817866989149, -1.324960789524878946 ) ) ;
#16971 = ORIENTED_EDGE ( 'NONE', *, *, #13099, .T. ) ;
#16972 = AXIS2_PLACEMENT_3D ( 'NONE', #27571, #45429, #11368 ) ;
#16973 = ADVANCED_FACE ( 'NONE', ( #38396 ), #21070, .F. ) ;
#16974 = FACE_OUTER_BOUND ( 'NONE', #38511, .T. ) ;
#16975 = CARTESIAN_POINT ( 'NONE',  ( -11.40636015113596180, 0.000000000000000000, 11.32142374880780089 ) ) ;
#16976 = PLANE ( 'NONE',  #531 ) ;
#16977 = ORIENTED_EDGE ( 'NONE', *, *, #18097, .T. ) ;
#16978 = DIRECTION ( 'NONE',  ( 0.5449076811759707706, 0.6444004775717708799, -0.5364919789714476250 ) ) ;
#16979 = ORIENTED_EDGE ( 'NONE', *, *, #12047, .F. ) ;
#16980 = LINE ( 'NONE', #34556, #30954 ) ;
#16981 = VECTOR ( 'NONE', #1765, 1000.000000000000000 ) ;
#16982 = DIRECTION ( 'NONE',  ( -0.9999697198139514409, -0.000000000000000000, -0.007781995580013368816 ) ) ;
#16983 = EDGE_CURVE ( 'NONE', #8639, #21780, #33861, .T. ) ;
#16984 = CARTESIAN_POINT ( 'NONE',  ( -29.86274838104827367, -0.1191753592594197858, 8.381332038739175871 ) ) ;
#16985 = VECTOR ( 'NONE', #11742, 999.9999999999998863 ) ;
#16986 = DIRECTION ( 'NONE',  ( 0.007781995580012662783, 0.000000000000000000, -0.9999697198139514409 ) ) ;
#16987 = LINE ( 'NONE', #34306, #30218 ) ;
#16988 = FACE_OUTER_BOUND ( 'NONE', #469, .T. ) ;
#16989 = LINE ( 'NONE', #9285, #17577 ) ;
#16990 = PLANE ( 'NONE',  #44040 ) ;
#16991 = ORIENTED_EDGE ( 'NONE', *, *, #17543, .T. ) ;
#16992 = DIRECTION ( 'NONE',  ( 0.007781995580012663651, -3.146120232559066537E-19, -0.9999697198139514409 ) ) ;
#16993 = ORIENTED_EDGE ( 'NONE', *, *, #45263, .F. ) ;
#16994 = VECTOR ( 'NONE', #17448, 1000.000000000000114 ) ;
#16995 = CARTESIAN_POINT ( 'NONE',  ( -18.67775241435682432, 0.000000000000000000, 4.136394454059623804 ) ) ;
#16996 = LINE ( 'NONE', #55587, #25097 ) ;
#16997 = PLANE ( 'NONE',  #899 ) ;
#16998 = ADVANCED_FACE ( 'NONE', ( #34167 ), #17366, .T. ) ;
#16999 = CARTESIAN_POINT ( 'NONE',  ( -8.409922665610809034, 0.000000000000000000, 10.23674650875856962 ) ) ;
#17000 = LINE ( 'NONE', #3635, #50380 ) ;
#17001 = LINE ( 'NONE', #47083, #302 ) ;
#17002 = EDGE_LOOP ( 'NONE', ( #45520, #34695 ) ) ;
#17003 = CARTESIAN_POINT ( 'NONE',  ( -19.67298185230172436, 19.56802367012303989, 4.315122289059762473 ) ) ;
#17004 = LINE ( 'NONE', #34322, #32168 ) ;
#17005 = DIRECTION ( 'NONE',  ( -0.9999697198139514409, -0.000000000000000000, -0.007781995580013368816 ) ) ;
#17006 = ADVANCED_FACE ( 'NONE', ( #38967 ), #43498, .F. ) ;
#17007 = CARTESIAN_POINT ( 'NONE',  ( -21.47341775636118655, -0.1191753592594197858, 5.122631121243466090 ) ) ;
#17008 = CARTESIAN_POINT ( 'NONE',  ( -19.53245895536257493, 1.419719901456505395, 6.798393728507462264 ) ) ;
#17009 = EDGE_CURVE ( 'NONE', #40102, #22884, #29891, .T. ) ;
#17010 = DIRECTION ( 'NONE',  ( 0.000000000000000000, -1.000000000000000000, 0.000000000000000000 ) ) ;
#17011 = EDGE_CURVE ( 'NONE', #32502, #29020, #29629, .T. ) ;
#17012 = LINE ( 'NONE', #15869, #4777 ) ;
#17013 = EDGE_LOOP ( 'NONE', ( #7057, #37089, #46037, #31980 ) ) ;
#17014 = FACE_OUTER_BOUND ( 'NONE', #19911, .T. ) ;
#17015 = FACE_OUTER_BOUND ( 'NONE', #10106, .T. ) ;
#17016 = ORIENTED_EDGE ( 'NONE', *, *, #25891, .T. ) ;
#17017 = EDGE_LOOP ( 'NONE', ( #44924, #31716, #3940, #20288 ) ) ;
#17018 = DIRECTION ( 'NONE',  ( -0.005002170337468016433, -0.7660444431189770143, 0.6427681459581293666 ) ) ;
#17019 = EDGE_CURVE ( 'NONE', #20837, #29012, #25615, .T. ) ;
#17020 = EDGE_LOOP ( 'NONE', ( #48071, #11439, #39452, #4647 ) ) ;
#17021 = EDGE_CURVE ( 'NONE', #26517, #2943, #29321, .T. ) ;
#17022 = EDGE_CURVE ( 'NONE', #8862, #3167, #4045, .T. ) ;
#17023 = VECTOR ( 'NONE', #51827, 1000.000000000000227 ) ;
#17024 = VERTEX_POINT ( 'NONE', #34425 ) ;
#17025 = ORIENTED_EDGE ( 'NONE', *, *, #5637, .F. ) ;
#17026 = VERTEX_POINT ( 'NONE', #47479 ) ;
#17027 = CARTESIAN_POINT ( 'NONE',  ( -19.60834386242827776, 0.000000000000000000, 4.298478389818581213 ) ) ;
#17028 = ORIENTED_EDGE ( 'NONE', *, *, #8471, .F. ) ;
#17029 = PLANE ( 'NONE',  #13320 ) ;
#17030 = PLANE ( 'NONE',  #40327 ) ;
#17031 = ADVANCED_FACE ( 'NONE', ( #4346 ), #8592, .F. ) ;
#17032 = VECTOR ( 'NONE', #41558, 1000.000000000000227 ) ;
#17033 = ORIENTED_EDGE ( 'NONE', *, *, #30026, .T. ) ;
#17034 = ORIENTED_EDGE ( 'NONE', *, *, #27090, .F. ) ;
#17035 = EDGE_CURVE ( 'NONE', #3617, #4870, #43251, .T. ) ;
#17036 = DIRECTION ( 'NONE',  ( 0.000000000000000000, -1.000000000000000000, 0.000000000000000000 ) ) ;
#17037 = CARTESIAN_POINT ( 'NONE',  ( -22.40556560354864146, -0.1191753592594197858, 5.484709000965211523 ) ) ;
#17038 = EDGE_LOOP ( 'NONE', ( #39636, #16309, #28690, #26348 ) ) ;
#17039 = DIRECTION ( 'NONE',  ( 0.5364919789714477361, 0.6444004775717706579, 0.5449076811759711036 ) ) ;
#17040 = CARTESIAN_POINT ( 'NONE',  ( -15.96710241509184058, -0.1191753592594218814, 13.13259134697452879 ) ) ;
#17041 = VERTEX_POINT ( 'NONE', #21657 ) ;
#17042 = LINE ( 'NONE', #25277, #36575 ) ;
#17043 = ORIENTED_EDGE ( 'NONE', *, *, #31297, .T. ) ;
#17044 = LINE ( 'NONE', #29548, #34569 ) ;
#17045 = DIRECTION ( 'NONE',  ( -0.5364919789714478471, 0.6444004775717705469, -0.5449076811759709926 ) ) ;
#17046 = ORIENTED_EDGE ( 'NONE', *, *, #26619, .F. ) ;
#17047 = DIRECTION ( 'NONE',  ( 0.7660212471507180654, -0.6427876096865404731, 0.005961354470445141482 ) ) ;
#17048 = CARTESIAN_POINT ( 'NONE',  ( -14.03506048556014285, -0.1191753592594184813, 3.703189858250206079 ) ) ;
#17049 = PLANE ( 'NONE',  #14877 ) ;
#17050 = LINE ( 'NONE', #26673, #6558 ) ;
#17051 = ORIENTED_EDGE ( 'NONE', *, *, #831, .F. ) ;
#17052 = FACE_OUTER_BOUND ( 'NONE', #50109, .T. ) ;
#17053 = DIRECTION ( 'NONE',  ( 0.007781995580012663651, 0.000000000000000000, -0.9999697198139515519 ) ) ;
#17054 = LINE ( 'NONE', #8525, #24909 ) ;
#17055 = DIRECTION ( 'NONE',  ( 0.7660212471507180654, -0.6427876096865404731, 0.005961354470445141482 ) ) ;
#17056 = EDGE_CURVE ( 'NONE', #52307, #18978, #34696, .T. ) ;
#17057 = CARTESIAN_POINT ( 'NONE',  ( -24.26908309836554878, 0.000000000000000000, 6.108867788427308376 ) ) ;
#17058 = DIRECTION ( 'NONE',  ( -0.5449076811759708816, 0.6444004775717707689, 0.5364919789714475140 ) ) ;
#17059 = LINE ( 'NONE', #3432, #728 ) ;
#17060 = DIRECTION ( 'NONE',  ( -0.7660212471507179544, -0.6427876096865405842, -0.005961354470445141482 ) ) ;
#17061 = CARTESIAN_POINT ( 'NONE',  ( -19.37931499696963300, 2.876837460659007473, 9.130285569831087855 ) ) ;
#17062 = ORIENTED_EDGE ( 'NONE', *, *, #48105, .T. ) ;
#17063 =( NAMED_UNIT ( * ) SI_UNIT ( $, .STERADIAN. ) SOLID_ANGLE_UNIT ( ) );
#17064 = DIRECTION ( 'NONE',  ( 0.9999697198139515519, 0.000000000000000000, 0.007781995580013368816 ) ) ;
#17065 = VERTEX_POINT ( 'NONE', #8890 ) ;
#17066 = PLANE ( 'NONE',  #5720 ) ;
#17067 = DIRECTION ( 'NONE',  ( 0.007781995580012663651, -3.146120232559066537E-19, -0.9999697198139514409 ) ) ;
#17068 = ADVANCED_FACE ( 'NONE', ( #25348 ), #26193, .F. ) ;
#17069 = VECTOR ( 'NONE', #55372, 1000.000000000000114 ) ;
#17070 = LINE ( 'NONE', #11681, #14995 ) ;
#17071 = CARTESIAN_POINT ( 'NONE',  ( -14.99020076078985397, -0.1191753592594185784, 7.019745364034069013 ) ) ;
#17072 = ADVANCED_FACE ( 'NONE', ( #46635 ), #21909, .F. ) ;
#17073 = CARTESIAN_POINT ( 'NONE',  ( -14.95190377862070541, 3.200641362704010007, 2.387641711229373520 ) ) ;
#17074 = EDGE_LOOP ( 'NONE', ( #483, #3367, #45490, #40702 ) ) ;
#17075 = ORIENTED_EDGE ( 'NONE', *, *, #32631, .F. ) ;
#17076 = CARTESIAN_POINT ( 'NONE',  ( -14.40754437137767674, 0.000000000000000000, 4.708284283832102624 ) ) ;
#17077 = DIRECTION ( 'NONE',  ( 0.005002170337468016433, -0.7660444431189770143, -0.6427681459581293666 ) ) ;
#17078 = ORIENTED_EDGE ( 'NONE', *, *, #49399, .F. ) ;
#17079 = DIRECTION ( 'NONE',  ( -0.005961354470445682716, -0.6427876096865404731, 0.7660212471507180654 ) ) ;
#17080 = ORIENTED_EDGE ( 'NONE', *, *, #3982, .T. ) ;
#17081 = ADVANCED_FACE ( 'NONE', ( #38115 ), #16529, .F. ) ;
#17082 = FACE_OUTER_BOUND ( 'NONE', #51921, .T. ) ;
#17083 = EDGE_LOOP ( 'NONE', ( #11630, #41098, #27720, #28015, #2962 ) ) ;
#17084 = PLANE ( 'NONE',  #21141 ) ;
#17085 = ADVANCED_FACE ( 'NONE', ( #53426 ), #1163, .F. ) ;
#17086 = ORIENTED_EDGE ( 'NONE', *, *, #10390, .F. ) ;
#17087 = ORIENTED_EDGE ( 'NONE', *, *, #28862, .F. ) ;
#17088 = ORIENTED_EDGE ( 'NONE', *, *, #11490, .F. ) ;
#17089 = DIRECTION ( 'NONE',  ( 0.9321478471874541372, 0.000000000000000000, -0.3620778797217453771 ) ) ;
#17090 = LINE ( 'NONE', #3460, #25967 ) ;
#17091 = LINE ( 'NONE', #55404, #14873 ) ;
#17092 = ADVANCED_FACE ( 'NONE', ( #22499 ), #39544, .F. ) ;
#17093 = DIRECTION ( 'NONE',  ( 0.3535533905932738974, -0.6123724356957929160, 0.7071067811865487940 ) ) ;
#17094 = VERTEX_POINT ( 'NONE', #52848 ) ;
#17095 = ORIENTED_EDGE ( 'NONE', *, *, #38262, .T. ) ;
#17096 = ADVANCED_FACE ( 'NONE', ( #39809 ), #35535, .F. ) ;
#17097 = ORIENTED_EDGE ( 'NONE', *, *, #15076, .T. ) ;
#17098 = PLANE ( 'NONE',  #29464 ) ;
#17099 = EDGE_LOOP ( 'NONE', ( #37875, #16332, #16424, #35534 ) ) ;
#17100 = DIRECTION ( 'NONE',  ( -0.5364919789714478471, 0.6444004775717705469, -0.5449076811759709926 ) ) ;
#17101 = ORIENTED_EDGE ( 'NONE', *, *, #2500, .T. ) ;
#17102 = FACE_OUTER_BOUND ( 'NONE', #17414, .T. ) ;
#17103 = DIRECTION ( 'NONE',  ( 0.005002170337468016433, -0.7660444431189770143, -0.6427681459581293666 ) ) ;
#17104 = AXIS2_PLACEMENT_3D ( 'NONE', #33047, #24257, #2915 ) ;
#17105 = VERTEX_POINT ( 'NONE', #35277 ) ;
#17106 = FACE_OUTER_BOUND ( 'NONE', #35370, .T. ) ;
#17107 = VERTEX_POINT ( 'NONE', #23046 ) ;
#17108 = DIRECTION ( 'NONE',  ( -1.000000000000000000, 0.000000000000000000, 0.000000000000000000 ) ) ;
#17109 = FACE_OUTER_BOUND ( 'NONE', #2683, .T. ) ;
#17110 = VERTEX_POINT ( 'NONE', #31581 ) ;
#17111 = CARTESIAN_POINT ( 'NONE',  ( -19.38983669476062843, -1.489407457353155717, 6.657974164829091990 ) ) ;
#17112 = DIRECTION ( 'NONE',  ( -0.005961354470445682716, -0.6427876096865404731, 0.7660212471507180654 ) ) ;
#17113 = DIRECTION ( 'NONE',  ( 0.007781995580012663651, 0.000000000000000000, -0.9999697198139515519 ) ) ;
#17114 = ORIENTED_EDGE ( 'NONE', *, *, #39639, .T. ) ;
#17115 = CARTESIAN_POINT ( 'NONE',  ( -31.72704407542318350, -0.1191753592594197858, 9.105487798182664960 ) ) ;
#17116 = DIRECTION ( 'NONE',  ( 0.007781995580012663651, -3.146120232559066537E-19, -0.9999697198139514409 ) ) ;
#17117 = EDGE_CURVE ( 'NONE', #43329, #16440, #1465, .T. ) ;
#17118 = CARTESIAN_POINT ( 'NONE',  ( -20.54126990917373519, -0.1191753592594197858, 4.760553241521720658 ) ) ;
#17119 = LINE ( 'NONE', #51741, #14075 ) ;
#17120 = CARTESIAN_POINT ( 'NONE',  ( -14.93495759592298988, 0.000000000000000000, 12.77129166681078409 ) ) ;
#17121 = ADVANCED_FACE ( 'NONE', ( #27292 ), #44068, .F. ) ;
#17122 = DIRECTION ( 'NONE',  ( -0.3583679495452941066, -0.9335804264972041855, 0.000000000000000000 ) ) ;
#17123 = ORIENTED_EDGE ( 'NONE', *, *, #52767, .F. ) ;
#17124 = CARTESIAN_POINT ( 'NONE',  ( -14.53706007796989930, -0.1191753592594181482, 8.500600088833135004 ) ) ;
#17125 = EDGE_CURVE ( 'NONE', #32968, #7585, #9983, .T. ) ;
#17126 = LINE ( 'NONE', #55739, #20427 ) ;
#17127 = LINE ( 'NONE', #37877, #52237 ) ;
#17128 = ORIENTED_EDGE ( 'NONE', *, *, #45225, .T. ) ;
#17129 = PLANE ( 'NONE',  #31133 ) ;
#17130 = PLANE ( 'NONE',  #17749 ) ;
#17131 = ORIENTED_EDGE ( 'NONE', *, *, #30902, .T. ) ;
#17132 = EDGE_CURVE ( 'NONE', #53826, #38778, #52319, .T. ) ;
#17133 = EDGE_CURVE ( 'NONE', #43303, #6876, #31283, .T. ) ;
#17134 = EDGE_CURVE ( 'NONE', #35736, #5331, #9136, .T. ) ;
#17135 = FACE_OUTER_BOUND ( 'NONE', #42386, .T. ) ;
#17136 = CARTESIAN_POINT ( 'NONE',  ( -13.00742402505039585, 1.419719901456506728, 4.263848570455246012 ) ) ;
#17137 = DIRECTION ( 'NONE',  ( 0.7660212471507180654, -0.6427876096865404731, 0.005961354470445141482 ) ) ;
#17138 = CARTESIAN_POINT ( 'NONE',  ( -67.33297928875471428, 0.1329136931077638251, -0.6892805327783358971 ) ) ;
#17139 = ORIENTED_EDGE ( 'NONE', *, *, #21151, .F. ) ;
#17140 = ORIENTED_EDGE ( 'NONE', *, *, #130, .T. ) ;
#17141 = PLANE ( 'NONE',  #49373 ) ;
#17142 = CARTESIAN_POINT ( 'NONE',  ( -13.09716453136212166, -0.1191753592594190225, 2.602492572012935046 ) ) ;
#17143 = DIRECTION ( 'NONE',  ( 0.9999697198139515519, 0.000000000000000000, 0.007781995580013368816 ) ) ;
#17144 = PLANE ( 'NONE',  #3006 ) ;
#17145 = LINE ( 'NONE', #51218, #51868 ) ;
#17146 = EDGE_CURVE ( 'NONE', #17736, #17689, #48889, .T. ) ;
#17147 = CARTESIAN_POINT ( 'NONE',  ( -10.94028622754223967, 0.000000000000000000, 11.14038480894692995 ) ) ;
#17148 = ORIENTED_EDGE ( 'NONE', *, *, #4393, .F. ) ;
#17149 = DIRECTION ( 'NONE',  ( -0.5364919789714478471, 0.6444004775717705469, -0.5449076811759709926 ) ) ;
#17150 = EDGE_CURVE ( 'NONE', #11098, #16694, #27033, .T. ) ;
#17151 = CARTESIAN_POINT ( 'NONE',  ( -10.84028925556084388, -0.1191753592594197858, 11.14116300850493246 ) ) ;
#17152 = ORIENTED_EDGE ( 'NONE', *, *, #6415, .T. ) ;
#17153 = EDGE_CURVE ( 'NONE', #10765, #3186, #26741, .T. ) ;
#17154 = CARTESIAN_POINT ( 'NONE',  ( -27.99923088623136636, 0.000000000000000000, 7.757173251277078130 ) ) ;
#17155 = CARTESIAN_POINT ( 'NONE',  ( -19.15367902479211537, 2.067327705546507133, 7.714097475855159480 ) ) ;
#17156 = CARTESIAN_POINT ( 'NONE',  ( -29.86352658060627618, 0.000000000000000000, 8.481329010720569883 ) ) ;
#17157 = ORIENTED_EDGE ( 'NONE', *, *, #26454, .T. ) ;
#17158 = EDGE_CURVE ( 'NONE', #20365, #41108, #43767, .T. ) ;
#17159 = CARTESIAN_POINT ( 'NONE',  ( -20.63663870328428374, 20.74370693537071020, -4.329125112780540796 ) ) ;
#17160 = ORIENTED_EDGE ( 'NONE', *, *, #25010, .F. ) ;
#17161 = ORIENTED_EDGE ( 'NONE', *, *, #16808, .T. ) ;
#17162 = ORIENTED_EDGE ( 'NONE', *, *, #11282, .T. ) ;
#17163 = ORIENTED_EDGE ( 'NONE', *, *, #15376, .F. ) ;
#17164 = DIRECTION ( 'NONE',  ( -0.5449076811759708816, 0.6444004775717707689, 0.5364919789714475140 ) ) ;
#17165 = ORIENTED_EDGE ( 'NONE', *, *, #29211, .F. ) ;
#17166 = CARTESIAN_POINT ( 'NONE',  ( -11.13054826722768098, 24.50000000000005684, -3.000000000000000000 ) ) ;
#17167 = ORIENTED_EDGE ( 'NONE', *, *, #26055, .T. ) ;
#17168 = CARTESIAN_POINT ( 'NONE',  ( -19.46808184255099405, 2.760183692663749078, 7.523411736767075197 ) ) ;
#17169 = ORIENTED_EDGE ( 'NONE', *, *, #27155, .F. ) ;
#17170 = CARTESIAN_POINT ( 'NONE',  ( -17.33350361953226582, -0.1191753592594149563, 9.586833727998367749 ) ) ;
#17171 = ORIENTED_EDGE ( 'NONE', *, *, #9315, .F. ) ;
#17172 = LINE ( 'NONE', #42459, #24780 ) ;
#17173 = LINE ( 'NONE', #30538, #32318 ) ;
#17174 = DIRECTION ( 'NONE',  ( 0.9321478471874541372, 0.000000000000000000, -0.3620778797217453771 ) ) ;
#17175 = LINE ( 'NONE', #25155, #55905 ) ;
#17176 = DIRECTION ( 'NONE',  ( 0.6427681459581294776, -0.7660444431189769032, 0.005002170337467562802 ) ) ;
#17177 = VERTEX_POINT ( 'NONE', #18802 ) ;
#17178 = ORIENTED_EDGE ( 'NONE', *, *, #30109, .F. ) ;
#17179 = CARTESIAN_POINT ( 'NONE',  ( -15.35274483170226389, 0.000000000000000000, 6.747594920547692610 ) ) ;
#17180 = LINE ( 'NONE', #51806, #45689 ) ;
#17181 = DIRECTION ( 'NONE',  ( -0.5364919789714478471, 0.6444004775717705469, -0.5449076811759709926 ) ) ;
#17182 = CARTESIAN_POINT ( 'NONE',  ( -16.18826075967313116, -2.137015261443160341, 3.101209376544761920 ) ) ;
#17183 = FACE_OUTER_BOUND ( 'NONE', #23619, .T. ) ;
#17184 = LINE ( 'NONE', #3564, #44990 ) ;
#17185 = EDGE_LOOP ( 'NONE', ( #29118, #14773, #10695, #2773 ) ) ;
#17186 = DIRECTION ( 'NONE',  ( 0.000000000000000000, -1.000000000000000000, 0.000000000000000000 ) ) ;
#17187 = CARTESIAN_POINT ( 'NONE',  ( -16.02887188652727701, 0.000000000000000000, 8.219661422694739983 ) ) ;
#17188 = VERTEX_POINT ( 'NONE', #39235 ) ;
#17189 = ADVANCED_FACE ( 'NONE', ( #4882 ), #632, .F. ) ;
#17190 = EDGE_CURVE ( 'NONE', #53080, #1201, #35009, .T. ) ;
#17191 = CARTESIAN_POINT ( 'NONE',  ( -19.63369567569543150, -0.1191753592594164690, 6.614276543096206495 ) ) ;
#17192 = CARTESIAN_POINT ( 'NONE',  ( -20.86483076077407617, 3.524445264749008100, 10.77014507662227594 ) ) ;
#17193 = PLANE ( 'NONE',  #19578 ) ;
#17194 = EDGE_CURVE ( 'NONE', #18056, #30132, #30984, .T. ) ;
#17195 = DIRECTION ( 'NONE',  ( 0.7660212471507180654, -0.6427876096865404731, 0.005961354470445141482 ) ) ;
#17196 = ORIENTED_EDGE ( 'NONE', *, *, #18757, .T. ) ;
#17197 = ORIENTED_EDGE ( 'NONE', *, *, #45354, .F. ) ;
#17198 = CARTESIAN_POINT ( 'NONE',  ( -22.40478740399063895, 0.000000000000000000, 5.384712028983816623 ) ) ;
#17199 = DIRECTION ( 'NONE',  ( 0.000000000000000000, -0.000000000000000000, -1.000000000000000000 ) ) ;
#17200 = CARTESIAN_POINT ( 'NONE',  ( -13.73672976910459909, 0.000000000000000000, 12.22661844811216270 ) ) ;
#17201 = DIRECTION ( 'NONE',  ( 0.9999697198139515519, 0.000000000000000000, 0.007781995580013368816 ) ) ;
#17202 = CARTESIAN_POINT ( 'NONE',  ( -15.78864119349052153, 0.000000000000000000, 3.050881976202041379 ) ) ;
#17203 = FACE_OUTER_BOUND ( 'NONE', #52947, .T. ) ;
#17204 = DIRECTION ( 'NONE',  ( 0.6427681459581294776, -0.7660444431189769032, 0.005002170337467562802 ) ) ;
#17206 = EDGE_CURVE ( 'NONE', #1154, #621, #23338, .T. ) ;
#17205 = ORIENTED_EDGE ( 'NONE', *, *, #33159, .F. ) ;
#17207 = FACE_OUTER_BOUND ( 'NONE', #12490, .T. ) ;
#17208 = CARTESIAN_POINT ( 'NONE',  ( -12.70458494993575194, -0.1191753592594197858, 11.86531876794841978 ) ) ;
#17209 = ADVANCED_FACE ( 'NONE', ( #2568 ), #11660, .T. ) ;
#17210 = VERTEX_POINT ( 'NONE', #15917 ) ;
#17211 = PLANE ( 'NONE',  #29214 ) ;
#17212 = ORIENTED_EDGE ( 'NONE', *, *, #7002, .F. ) ;
#17213 = DIRECTION ( 'NONE',  ( -0.6246952433987893460, -0.7422098413412802076, 0.2426528472758542054 ) ) ;
#17214 = EDGE_LOOP ( 'NONE', ( #31026, #11694, #21675, #47883 ) ) ;
#17215 = EDGE_CURVE ( 'NONE', #27257, #1128, #37206, .T. ) ;
#17216 = ORIENTED_EDGE ( 'NONE', *, *, #11525, .T. ) ;
#17217 = ADVANCED_FACE ( 'NONE', ( #1727 ), #24425, .F. ) ;
#17218 = ORIENTED_EDGE ( 'NONE', *, *, #36040, .F. ) ;
#17219 = VERTEX_POINT ( 'NONE', #32667 ) ;
#17220 = EDGE_LOOP ( 'NONE', ( #8536, #12041, #47368, #25104 ) ) ;
#17221 = ORIENTED_EDGE ( 'NONE', *, *, #4792, .T. ) ;
#17222 = CARTESIAN_POINT ( 'NONE',  ( -13.07991603883496623, 3.686347215771509145, 8.011928505754800867 ) ) ;
#17223 = CARTESIAN_POINT ( 'NONE',  ( -27.06552663992790997, 0.000000000000000000, 7.195101427592543786 ) ) ;
#17224 = LINE ( 'NONE', #9260, #13131 ) ;
#17225 = ORIENTED_EDGE ( 'NONE', *, *, #14231, .F. ) ;
#17226 = CARTESIAN_POINT ( 'NONE',  ( -16.73803336170967526, 0.000000000000000000, 5.628818075470372939 ) ) ;
#17227 = ORIENTED_EDGE ( 'NONE', *, *, #42339, .T. ) ;
#17228 = DIRECTION ( 'NONE',  ( -0.5449076811759708816, 0.6444004775717707689, 0.5364919789714475140 ) ) ;
#17229 = EDGE_LOOP ( 'NONE', ( #1816, #28618, #34649, #18930 ) ) ;
#17230 = PLANE ( 'NONE',  #34857 ) ;
#17231 = CARTESIAN_POINT ( 'NONE',  ( 5.446213544912835935, -1.070058632457643766, -0.6896135826588382089 ) ) ;
#17232 = ORIENTED_EDGE ( 'NONE', *, *, #7300, .T. ) ;
#17233 = DIRECTION ( 'NONE',  ( 0.6427681459581294776, -0.7660444431189769032, 0.005002170337467562802 ) ) ;
#17234 = ORIENTED_EDGE ( 'NONE', *, *, #54597, .T. ) ;
#17235 = FACE_OUTER_BOUND ( 'NONE', #4278, .T. ) ;
#17236 = CARTESIAN_POINT ( 'NONE',  ( -14.66887761629205222, 0.000000000000000000, 12.58869632783390990 ) ) ;
#17237 = AXIS2_PLACEMENT_3D ( 'NONE', #1835, #23173, #10389 ) ;
#17238 = FACE_OUTER_BOUND ( 'NONE', #32102, .T. ) ;
#17239 = CARTESIAN_POINT ( 'NONE',  ( -17.41547807092396027, 0.000000000000000000, 7.270200336912393091 ) ) ;
#17240 = FACE_OUTER_BOUND ( 'NONE', #35291, .T. ) ;
#17241 = FACE_OUTER_BOUND ( 'NONE', #23449, .T. ) ;
#17242 = CARTESIAN_POINT ( 'NONE',  ( -25.20278734466900517, 0.000000000000000000, 6.670939612111840944 ) ) ;
#17243 = CARTESIAN_POINT ( 'NONE',  ( -68.01236371044051054, -8.487308885305189676, 5.059064008999122564 ) ) ;
#17244 = ORIENTED_EDGE ( 'NONE', *, *, #12744, .T. ) ;
#17245 = LINE ( 'NONE', #30323, #9313 ) ;
#17246 = VERTEX_POINT ( 'NONE', #53684 ) ;
#17247 = EDGE_CURVE ( 'NONE', #1327, #42332, #28130, .T. ) ;
#17248 = FACE_OUTER_BOUND ( 'NONE', #1633, .T. ) ;
#17249 = LINE ( 'NONE', #48478, #1494 ) ;
#17250 = CARTESIAN_POINT ( 'NONE',  ( -20.16176772743538237, -0.1191753592594197858, 14.76194180572237968 ) ) ;
#17251 = CARTESIAN_POINT ( 'NONE',  ( -20.18605513093877946, 0.000000000000000000, 5.032646646757750197 ) ) ;
#17252 = FACE_OUTER_BOUND ( 'NONE', #39795, .T. ) ;
#17253 = ADVANCED_FACE ( 'NONE', ( #2290 ), #54510, .F. ) ;
#17254 = ADVANCED_FACE ( 'NONE', ( #32953 ), #2825, .F. ) ;
#17255 = PLANE ( 'NONE',  #10525 ) ;
#17256 = DIRECTION ( 'NONE',  ( 0.000000000000000000, 0.000000000000000000, -1.000000000000000000 ) ) ;
#17257 = ORIENTED_EDGE ( 'NONE', *, *, #51503, .T. ) ;
#17258 = DIRECTION ( 'NONE',  ( 0.007781995580012663651, 0.000000000000000000, -0.9999697198139515519 ) ) ;
#17259 = DIRECTION ( 'NONE',  ( -0.5449076811759708816, 0.6444004775717707689, 0.5364919789714475140 ) ) ;
#17260 = LINE ( 'NONE', #39965, #34548 ) ;
#17261 = CARTESIAN_POINT ( 'NONE',  ( -17.62617585138765008, -3.117730071725258956, 12.26528855537868701 ) ) ;
#17262 = CARTESIAN_POINT ( 'NONE',  ( -17.68742552992882366, 0.000000000000000000, 8.206754174738705387 ) ) ;
#17263 = CARTESIAN_POINT ( 'NONE',  ( -27.99923088623136636, 0.000000000000000000, 7.757173251277078130 ) ) ;
#17264 = LINE ( 'NONE', #51902, #35632 ) ;
#17265 = ORIENTED_EDGE ( 'NONE', *, *, #29279, .F. ) ;
#17266 = DIRECTION ( 'NONE',  ( 0.005002170337468016433, -0.7660444431189770143, -0.6427681459581293666 ) ) ;
#17267 = DIRECTION ( 'NONE',  ( -0.5449076811759708816, 0.6444004775717707689, 0.5364919789714475140 ) ) ;
#17268 = ORIENTED_EDGE ( 'NONE', *, *, #18890, .T. ) ;
#17269 = VERTEX_POINT ( 'NONE', #24170 ) ;
#17270 = DIRECTION ( 'NONE',  ( 0.5449076811759707706, 0.6444004775717708799, -0.5364919789714476250 ) ) ;
#17271 = ORIENTED_EDGE ( 'NONE', *, *, #7102, .T. ) ;
#17272 = ADVANCED_FACE ( 'NONE', ( #41195 ), #15098, .F. ) ;
#17273 = VECTOR ( 'NONE', #47734, 1000.000000000000227 ) ;
#17274 = ORIENTED_EDGE ( 'NONE', *, *, #51964, .T. ) ;
#17275 = ORIENTED_EDGE ( 'NONE', *, *, #40626, .T. ) ;
#17276 = VERTEX_POINT ( 'NONE', #33257 ) ;
#17277 = EDGE_CURVE ( 'NONE', #16077, #20216, #7126, .T. ) ;
#17278 = ORIENTED_EDGE ( 'NONE', *, *, #35052, .F. ) ;
#17279 = DIRECTION ( 'NONE',  ( 0.005002170337468016433, -0.7660444431189770143, -0.6427681459581293666 ) ) ;
#17280 = ADVANCED_FACE ( 'NONE', ( #32126 ), #14802, .F. ) ;
#17281 = DIRECTION ( 'NONE',  ( -0.005961354470445682716, -0.6427876096865404731, 0.7660212471507180654 ) ) ;
#17282 = ORIENTED_EDGE ( 'NONE', *, *, #38223, .T. ) ;
#17283 = EDGE_CURVE ( 'NONE', #9919, #46009, #49448, .T. ) ;
#17284 = CARTESIAN_POINT ( 'NONE',  ( -17.69317363693938816, 0.000000000000000000, 8.945373581254235873 ) ) ;
#17285 = ORIENTED_EDGE ( 'NONE', *, *, #37551, .F. ) ;
#17286 = CARTESIAN_POINT ( 'NONE',  ( -18.19747506107908563, 0.000000000000000000, 14.03856424583689311 ) ) ;
#17287 = DIRECTION ( 'NONE',  ( 0.007781995580012663651, 0.000000000000000000, -0.9999697198139515519 ) ) ;
#17288 = VERTEX_POINT ( 'NONE', #37486 ) ;
#17289 = LINE ( 'NONE', #7968, #29313 ) ;
#17290 = EDGE_LOOP ( 'NONE', ( #6339, #2793, #52826, #42563 ) ) ;
#17291 = VECTOR ( 'NONE', #28118, 1000.000000000000114 ) ;
#17292 = PLANE ( 'NONE',  #35500 ) ;
#17293 = EDGE_CURVE ( 'NONE', #10403, #36742, #19626, .T. ) ;
#17294 = LINE ( 'NONE', #25840, #19136 ) ;
#17295 = VERTEX_POINT ( 'NONE', #54805 ) ;
#17296 = CARTESIAN_POINT ( 'NONE',  ( -70.10219403106212610, -1.000000000000000666, -7.503912900124007912 ) ) ;
#17297 = DIRECTION ( 'NONE',  ( 0.000000000000000000, -1.000000000000000000, 0.000000000000000000 ) ) ;
#17298 = CARTESIAN_POINT ( 'NONE',  ( -27.06552663992790997, 0.000000000000000000, 7.195101427592543786 ) ) ;
#17299 = DIRECTION ( 'NONE',  ( -0.9999697198139514409, -0.000000000000000000, -0.007781995580013368816 ) ) ;
#17300 = EDGE_CURVE ( 'NONE', #7239, #45359, #49972, .T. ) ;
#17301 = ORIENTED_EDGE ( 'NONE', *, *, #30444, .F. ) ;
#17302 = AXIS2_PLACEMENT_3D ( 'NONE', #26737, #13951, #44599 ) ;
#17303 = EDGE_CURVE ( 'NONE', #48501, #24198, #50564, .T. ) ;
#17304 = FACE_OUTER_BOUND ( 'NONE', #29192, .T. ) ;
#17305 = FACE_OUTER_BOUND ( 'NONE', #16290, .T. ) ;
#17306 = DIRECTION ( 'NONE',  ( -0.5364919789714478471, 0.6444004775717705469, -0.5449076811759709926 ) ) ;
#17307 = PLANE ( 'NONE',  #49534 ) ;
#17308 = CARTESIAN_POINT ( 'NONE',  ( -14.24932064311472146, 1.257817950434004350, 2.176720800223820529 ) ) ;
#17309 = LINE ( 'NONE', #47137, #53061 ) ;
#17310 = ADVANCED_FACE ( 'NONE', ( #32423 ), #19327, .F. ) ;
#17311 = DIRECTION ( 'NONE',  ( 0.9321478471874541372, 0.000000000000000000, -0.3620778797217453771 ) ) ;
#17312 = AXIS2_PLACEMENT_3D ( 'NONE', #32009, #14976, #45613 ) ;
#17313 = LINE ( 'NONE', #9087, #17506 ) ;
#17314 = DIRECTION ( 'NONE',  ( 0.9999697198139515519, 0.000000000000000000, 0.007781995580013368816 ) ) ;
#17315 = ORIENTED_EDGE ( 'NONE', *, *, #23614, .F. ) ;
#17316 = SURFACE_STYLE_FILL_AREA ( #42881 ) ;
#17317 = PLANE ( 'NONE',  #22382 ) ;
#17318 = EDGE_LOOP ( 'NONE', ( #30940, #42640, #52000, #53735 ) ) ;
#17319 = DIRECTION ( 'NONE',  ( -0.6427681459581293666, -0.7660444431189770143, -0.005002170337467561935 ) ) ;
#17320 = DIRECTION ( 'NONE',  ( -0.5449076811759708816, 0.6444004775717707689, 0.5364919789714475140 ) ) ;
#17321 = PRODUCT_RELATED_PRODUCT_CATEGORY ( 'part', '', ( #31892 ) ) ;
#17322 = LINE ( 'NONE', #24124, #32734 ) ;
#17323 = CARTESIAN_POINT ( 'NONE',  ( -15.43184522958867788, -0.1191753592594192307, 4.061651826203944715 ) ) ;
#17324 = CARTESIAN_POINT ( 'NONE',  ( -18.30775837356714675, 1.095915999411505526, 3.758321359744400070 ) ) ;
#17325 = ADVANCED_FACE ( 'NONE', ( #29554 ), #25842, .F. ) ;
#17326 = ORIENTED_EDGE ( 'NONE', *, *, #5863, .F. ) ;
#17327 = ORIENTED_EDGE ( 'NONE', *, *, #10690, .F. ) ;
#17328 = DIRECTION ( 'NONE',  ( 0.6427681459581294776, -0.7660444431189769032, 0.005002170337467562802 ) ) ;
#17329 = B_SPLINE_SURFACE_WITH_KNOTS ( 'NONE', 1, 3, ( 
 ( #27765, #44492, #36276, #22650, #18103, #32005, #35715, #18958, #45088, #36023, #5601, #31472, #27461, #22925 ),
 ( #40245, #5899, #48788, #1336, #53329, #18374, #23225, #14426, #35427, #1632, #53574, #31734, #14680, #49038 ) ),
 .UNSPECIFIED., .F., .F., .F.,
 ( 2, 2 ),
 ( 4, 2, 2, 2, 2, 2, 4 ),
 ( 0.000000000000000000, 1.000000000000000000 ),
 ( 0.000000000000000000, 0.1159099261691615840, 0.2318198523383231680, 0.4636397046766463359, 0.6954595570149695316, 0.9272794093532926718, 1.000000000000000000 ),
 .UNSPECIFIED. ) ;
#17330 = PLANE ( 'NONE',  #13200 ) ;
#17332 = VERTEX_POINT ( 'NONE', #7380 ) ;
#17331 = APPLICATION_CONTEXT ( 'automotive_design' ) ;
#17333 = CARTESIAN_POINT ( 'NONE',  ( -15.40103151951671734, 0.000000000000000000, 12.95233060667165681 ) ) ;
#17334 = VECTOR ( 'NONE', #33212, 999.9999999999998863 ) ;
#17335 = VECTOR ( 'NONE', #25837, 1000.000000000000227 ) ;
#17336 = ORIENTED_EDGE ( 'NONE', *, *, #38633, .T. ) ;
#17337 = DIRECTION ( 'NONE',  ( -0.7660212471507179544, -0.6427876096865405842, -0.005961354470445141482 ) ) ;
#17338 = VERTEX_POINT ( 'NONE', #21593 ) ;
#17339 = CARTESIAN_POINT ( 'NONE',  ( -13.63673279712320507, -0.1191753592594197858, 12.22739664767016521 ) ) ;
#17340 = ORIENTED_EDGE ( 'NONE', *, *, #52670, .T. ) ;
#17341 = ORIENTED_EDGE ( 'NONE', *, *, #5613, .T. ) ;
#17342 = EDGE_LOOP ( 'NONE', ( #47060, #16185, #26442, #50535 ) ) ;
#17343 = CARTESIAN_POINT ( 'NONE',  ( -13.97033035520014010, 0.000000000000000000, 8.235681468882781076 ) ) ;
#17344 = PLANE ( 'NONE',  #52261 ) ;
#17345 = PLANE ( 'NONE',  #44788 ) ;
#17346 = DIRECTION ( 'NONE',  ( -0.7660212471507179544, -0.6427876096865405842, -0.005961354470445141482 ) ) ;
#17347 = VERTEX_POINT ( 'NONE', #56209 ) ;
#17348 = ADVANCED_FACE ( 'NONE', ( #34362 ), #46868, .F. ) ;
#17349 = ORIENTED_EDGE ( 'NONE', *, *, #1210, .F. ) ;
#17350 = AXIS2_PLACEMENT_3D ( 'NONE', #53609, #28902, #49900 ) ;
#17351 = ORIENTED_EDGE ( 'NONE', *, *, #27592, .F. ) ;
#17352 = DIRECTION ( 'NONE',  ( 0.6427681459581294776, -0.7660444431189769032, 0.005002170337467562802 ) ) ;
#17353 = VERTEX_POINT ( 'NONE', #43175 ) ;
#17354 = PLANE ( 'NONE',  #31185 ) ;
#17355 = ORIENTED_EDGE ( 'NONE', *, *, #54011, .T. ) ;
#17356 = CARTESIAN_POINT ( 'NONE',  ( -11.67244013076689946, 0.000000000000000000, 11.50401908778467863 ) ) ;
#17357 = PLANE ( 'NONE',  #23088 ) ;
#17358 = EDGE_CURVE ( 'NONE', #26046, #4586, #3970, .T. ) ;
#17359 = ORIENTED_EDGE ( 'NONE', *, *, #14206, .F. ) ;
#17360 = DIRECTION ( 'NONE',  ( 0.000000000000000000, 0.000000000000000000, 1.000000000000000000 ) ) ;
#17361 = VERTEX_POINT ( 'NONE', #12212 ) ;
#17362 = EDGE_CURVE ( 'NONE', #50871, #25675, #29828, .T. ) ;
#17363 = ADVANCED_FACE ( 'NONE', ( #51412 ), #47128, .F. ) ;
#17364 = CARTESIAN_POINT ( 'NONE',  ( -56.20083583094844926, 4.876814673940706335, -3.000000000000007105 ) ) ;
#17365 = ORIENTED_EDGE ( 'NONE', *, *, #13535, .F. ) ;
#17366 = PLANE ( 'NONE',  #25051 ) ;
#17367 = PLANE ( 'NONE',  #50204 ) ;
#17368 = DIRECTION ( 'NONE',  ( 0.6427681459581294776, -0.7660444431189769032, 0.005002170337467562802 ) ) ;
#17369 = EDGE_CURVE ( 'NONE', #50265, #6886, #33515, .T. ) ;
#17370 = EDGE_LOOP ( 'NONE', ( #32570, #35378, #49705, #48778 ) ) ;
#17372 = CARTESIAN_POINT ( 'NONE',  ( -15.73373731979538270, -3.756034771668160577, 8.957742581241667779 ) ) ;
#17371 = VECTOR ( 'NONE', #48419, 999.9999999999998863 ) ;
#17373 = VECTOR ( 'NONE', #50041, 999.9999999999998863 ) ;
#17374 = ADVANCED_FACE ( 'NONE', ( #21294 ), #29242, .F. ) ;
#17375 = CARTESIAN_POINT ( 'NONE',  ( -19.60912206198628027, -0.1191753592594197858, 4.398475361799976113 ) ) ;
#17376 = LINE ( 'NONE', #39243, #50270 ) ;
#17377 = LINE ( 'NONE', #38975, #11372 ) ;
#17378 = PLANE ( 'NONE',  #34012 ) ;
#17379 = EDGE_CURVE ( 'NONE', #54774, #1004, #4279, .T. ) ;
#17380 = DIRECTION ( 'NONE',  ( 0.000000000000000000, 1.000000000000000000, -0.000000000000000000 ) ) ;
#17381 = CARTESIAN_POINT ( 'NONE',  ( -18.67775241435682432, 0.000000000000000000, 4.136394454059623804 ) ) ;
#17382 = VECTOR ( 'NONE', #16536, 999.9999999999998863 ) ;
#17383 = EDGE_LOOP ( 'NONE', ( #35452, #48412, #29494, #27732 ) ) ;
#17384 = CARTESIAN_POINT ( 'NONE',  ( -7.094024697029445825, 2.107956770024262294, 8.730276719704061605 ) ) ;
#17385 = DIRECTION ( 'NONE',  ( 0.9999697198139515519, 0.000000000000000000, 0.007781995580013368816 ) ) ;
#17386 = LINE ( 'NONE', #52031, #36883 ) ;
#17387 = ORIENTED_EDGE ( 'NONE', *, *, #30073, .F. ) ;
#17388 = LINE ( 'NONE', #2990, #7535 ) ;
#17389 = CARTESIAN_POINT ( 'NONE',  ( -27.06708303904391144, 0.000000000000000000, 7.395095371555332697 ) ) ;
#17390 = ORIENTED_EDGE ( 'NONE', *, *, #6453, .T. ) ;
#17391 = ADVANCED_FACE ( 'NONE', ( #24698 ), #20999, .T. ) ;
#17392 = DIRECTION ( 'NONE',  ( 0.000000000000000000, 5.782411586589354681E-16, -1.000000000000000000 ) ) ;
#17393 = CARTESIAN_POINT ( 'NONE',  ( -6.824261881224860993, 4.558205123441750217, -0.5675985080870675770 ) ) ;
#17394 = AXIS2_PLACEMENT_3D ( 'NONE', #18722, #21834, #5376 ) ;
#17395 = DIRECTION ( 'NONE',  ( -0.6427681459581293666, -0.7660444431189770143, -0.005002170337467561935 ) ) ;
#17396 = VECTOR ( 'NONE', #15008, 999.9999999999998863 ) ;
#17397 = CARTESIAN_POINT ( 'NONE',  ( -66.30048190469359781, 1.999999999999976685, 5.092367036307550165 ) ) ;
#17398 = EDGE_CURVE ( 'NONE', #51697, #18162, #46561, .T. ) ;
#17399 = ORIENTED_EDGE ( 'NONE', *, *, #54367, .F. ) ;
#17400 = ORIENTED_EDGE ( 'NONE', *, *, #31507, .F. ) ;
#17401 = LINE ( 'NONE', #13161, #21276 ) ;
#17402 = DIRECTION ( 'NONE',  ( 0.005002170337468016433, -0.7660444431189770143, -0.6427681459581293666 ) ) ;
#17403 = LINE ( 'NONE', #8627, #16002 ) ;
#17404 = LINE ( 'NONE', #47222, #36586 ) ;
#17405 = CARTESIAN_POINT ( 'NONE',  ( -16.28854238969427470, -3.917936722690662954, 3.083341448462168621 ) ) ;
#17406 = DIRECTION ( 'NONE',  ( 0.7660212471507180654, -0.6427876096865404731, 0.005961354470445141482 ) ) ;
#17407 = EDGE_LOOP ( 'NONE', ( #39259, #14555, #16259, #18245 ) ) ;
#17408 = DIRECTION ( 'NONE',  ( 0.007781995580012662783, 0.000000000000000000, -0.9999697198139514409 ) ) ;
#17409 = DIRECTION ( 'NONE',  ( 0.005002170337468016433, -0.7660444431189770143, -0.6427681459581293666 ) ) ;
#17410 = ORIENTED_EDGE ( 'NONE', *, *, #48428, .F. ) ;
#17411 = CARTESIAN_POINT ( 'NONE',  ( -13.03021690632542828, 3.686347215771511365, 1.625696709606834434 ) ) ;
#17412 = DIRECTION ( 'NONE',  ( 0.000000000000000000, -1.000000000000000000, 0.000000000000000000 ) ) ;
#17413 = DIRECTION ( 'NONE',  ( 0.000000000000000000, 0.000000000000000000, 1.000000000000000000 ) ) ;
#17414 = EDGE_LOOP ( 'NONE', ( #28047, #12285, #18293, #20998 ) ) ;
#17415 = VECTOR ( 'NONE', #3088, 1000.000000000000114 ) ;
#17416 = VECTOR ( 'NONE', #31583, 1000.000000000000227 ) ;
#17417 = DIRECTION ( 'NONE',  ( -0.005002170337468016433, -0.7660444431189770143, 0.6427681459581293666 ) ) ;
#17418 = ADVANCED_FACE ( 'NONE', ( #51666 ), #25546, .F. ) ;
#17419 = VERTEX_POINT ( 'NONE', #17296 ) ;
#17420 = ORIENTED_EDGE ( 'NONE', *, *, #36355, .F. ) ;
#17421 = ORIENTED_EDGE ( 'NONE', *, *, #17153, .T. ) ;
#17422 = VECTOR ( 'NONE', #12777, 1000.000000000000227 ) ;
#17423 = ORIENTED_EDGE ( 'NONE', *, *, #10218, .F. ) ;
#17424 = FACE_OUTER_BOUND ( 'NONE', #1602, .T. ) ;
#17426 = ADVANCED_FACE ( 'NONE', ( #13060 ), #37796, .F. ) ;
#17425 = ORIENTED_EDGE ( 'NONE', *, *, #3453, .T. ) ;
#17427 = CARTESIAN_POINT ( 'NONE',  ( -15.34211164085077783, 22.06845275252959127, -3.955769444135373014 ) ) ;
#17428 = EDGE_CURVE ( 'NONE', #33926, #14055, #47405, .T. ) ;
#17429 = VERTEX_POINT ( 'NONE', #20737 ) ;
#17430 = DIRECTION ( 'NONE',  ( 0.007781995580012662783, 0.000000000000000000, -0.9999697198139514409 ) ) ;
#17431 = VERTEX_POINT ( 'NONE', #55361 ) ;
#17433 = AXIS2_PLACEMENT_3D ( 'NONE', #56091, #4670, #52641 ) ;
#17432 = CARTESIAN_POINT ( 'NONE',  ( -14.45241350051485796, -1.165603555308155626, 4.208693952685643502 ) ) ;
#17434 = EDGE_LOOP ( 'NONE', ( #52390, #25197, #21561, #3507 ) ) ;
#17435 = EDGE_CURVE ( 'NONE', #9089, #31401, #16457, .T. ) ;
#17436 = FACE_OUTER_BOUND ( 'NONE', #37667, .T. ) ;
#17437 = CARTESIAN_POINT ( 'NONE',  ( -18.80076660093136809, 0.000000000000000000, 6.151423491835070756 ) ) ;
#17438 = FACE_OUTER_BOUND ( 'NONE', #35324, .T. ) ;
#17439 = DIRECTION ( 'NONE',  ( 0.9999697198139515519, 0.000000000000000000, 0.007781995580013368816 ) ) ;
#17440 = DIRECTION ( 'NONE',  ( 0.007781995580012663651, 0.000000000000000000, -0.9999697198139515519 ) ) ;
#17441 = ORIENTED_EDGE ( 'NONE', *, *, #33891, .F. ) ;
#17442 = VERTEX_POINT ( 'NONE', #13882 ) ;
#17443 = ADVANCED_FACE ( 'NONE', ( #36061 ), #47973, .F. ) ;
#17444 = LINE ( 'NONE', #35088, #27657 ) ;
#17445 = DIRECTION ( 'NONE',  ( -0.005002170337468016433, -0.7660444431189770143, 0.6427681459581293666 ) ) ;
#17446 = AXIS2_PLACEMENT_3D ( 'NONE', #21742, #52114, #22011 ) ;
#17447 = ADVANCED_FACE ( 'NONE', ( #39164 ), #52246, .F. ) ;
#17448 = DIRECTION ( 'NONE',  ( 0.2426528472758541499, 0.7422098413412800966, 0.6246952433987894571 ) ) ;
#17449 = PLANE ( 'NONE',  #48466 ) ;
#17450 = EDGE_CURVE ( 'NONE', #32241, #47466, #14197, .T. ) ;
#17451 = CARTESIAN_POINT ( 'NONE',  ( -19.89959890415981292, 0.7721120973665049902, 4.386977320733340235 ) ) ;
#17452 = DIRECTION ( 'NONE',  ( 0.000000000000000000, -1.000000000000000000, 0.000000000000000000 ) ) ;
#17453 = ORIENTED_EDGE ( 'NONE', *, *, #13387, .F. ) ;
#17455 = CARTESIAN_POINT ( 'NONE',  ( 0.09621548157177391147, -1.683565401097097070, -3.964956190634383340E-16 ) ) ;
#17454 = VECTOR ( 'NONE', #10019, 1000.000000000000227 ) ;
#17456 = DIRECTION ( 'NONE',  ( 0.007781995580012663651, -3.146120232559066537E-19, -0.9999697198139514409 ) ) ;
#17457 = ORIENTED_EDGE ( 'NONE', *, *, #52817, .F. ) ;
#17458 = AXIS2_PLACEMENT_3D ( 'NONE', #3928, #55606, #33480 ) ;
#17459 = EDGE_CURVE ( 'NONE', #20837, #33148, #31518, .T. ) ;
#17460 = VECTOR ( 'NONE', #9596, 1000.000000000000227 ) ;
#17461 = PLANE ( 'NONE',  #36128 ) ;
#17462 = CARTESIAN_POINT ( 'NONE',  ( -19.20472701092309720, 1.581621852479005552, 6.936800195413949766 ) ) ;
#17463 = CARTESIAN_POINT ( 'NONE',  ( -13.17065887352947762, -0.1191753592594197858, 12.04635770780929427 ) ) ;
#17464 = LINE ( 'NONE', #34796, #41361 ) ;
#17465 = CARTESIAN_POINT ( 'NONE',  ( -25.20200914511100265, -0.1191753592594197858, 6.570942640130446932 ) ) ;
#17466 = ORIENTED_EDGE ( 'NONE', *, *, #40263, .T. ) ;
#17467 = AXIS2_PLACEMENT_3D ( 'NONE', #24059, #41389, #9895 ) ;
#17468 = VECTOR ( 'NONE', #23488, 999.9999999999998863 ) ;
#17469 = VERTEX_POINT ( 'NONE', #40003 ) ;
#17470 = CARTESIAN_POINT ( 'NONE',  ( -30.79567442779373110, 0.000000000000000000, 8.843406890442315316 ) ) ;
#17471 = LINE ( 'NONE', #34802, #53077 ) ;
#17472 = CARTESIAN_POINT ( 'NONE',  ( -16.95371522758815885, 0.000000000000000000, 7.643125951938166907 ) ) ;
#17473 = LINE ( 'NONE', #30574, #31896 ) ;
#17474 = VECTOR ( 'NONE', #14729, 1000.000000000000000 ) ;
#17475 = LINE ( 'NONE', #22596, #22221 ) ;
#17477 = AXIS2_PLACEMENT_3D ( 'NONE', #24750, #15969, #15662 ) ;
#17476 = CARTESIAN_POINT ( 'NONE',  ( -11.88054826722767743, 25.79903810567671840, -3.133157401209314852 ) ) ;
#17478 = DIRECTION ( 'NONE',  ( -0.5364919789714478471, 0.6444004775717705469, -0.5449076811759709926 ) ) ;
#17479 = ORIENTED_EDGE ( 'NONE', *, *, #33655, .F. ) ;
#17480 = CARTESIAN_POINT ( 'NONE',  ( -16.97217308376872325, -0.8417996532631553119, 4.656036778316158475 ) ) ;
#17481 = CARTESIAN_POINT ( 'NONE',  ( -26.13493519185646008, 0.000000000000000000, 7.033017491833586377 ) ) ;
#17482 = ORIENTED_EDGE ( 'NONE', *, *, #33646, .F. ) ;
#17483 = LINE ( 'NONE', #30585, #37445 ) ;
#17484 = ORIENTED_EDGE ( 'NONE', *, *, #14484, .T. ) ;
#17485 = CARTESIAN_POINT ( 'NONE',  ( -57.29829478218162109, -10.27834239552269757, 4.211285351864063224E-15 ) ) ;
#17486 = ADVANCED_FACE ( 'NONE', ( #35762 ), #27228, .F. ) ;
#17487 = VECTOR ( 'NONE', #1305, 1000.000000000000000 ) ;
#17488 = CARTESIAN_POINT ( 'NONE',  ( -9.075990533167328067, 0.000000000000000000, 10.41622904950343909 ) ) ;
#17489 = VERTEX_POINT ( 'NONE', #13354 ) ;
#17490 = EDGE_CURVE ( 'NONE', #36296, #24378, #34930, .T. ) ;
#17491 = AXIS2_PLACEMENT_3D ( 'NONE', #41154, #1420, #2246 ) ;
#17492 = ORIENTED_EDGE ( 'NONE', *, *, #18939, .F. ) ;
#17493 = ORIENTED_EDGE ( 'NONE', *, *, #37078, .T. ) ;
#17494 = ORIENTED_EDGE ( 'NONE', *, *, #28815, .F. ) ;
#17495 = ORIENTED_EDGE ( 'NONE', *, *, #217, .F. ) ;
#17496 = EDGE_CURVE ( 'NONE', #31186, #38038, #5646, .T. ) ;
#17497 = ORIENTED_EDGE ( 'NONE', *, *, #30324, .F. ) ;
#17498 = VECTOR ( 'NONE', #37766, 1000.000000000000114 ) ;
#17499 = LINE ( 'NONE', #18852, #54925 ) ;
#17500 = DIRECTION ( 'NONE',  ( -0.005961354470445682716, -0.6427876096865404731, 0.7660212471507180654 ) ) ;
#17501 = LINE ( 'NONE', #26885, #38539 ) ;
#17502 = EDGE_CURVE ( 'NONE', #1004, #29284, #18144, .T. ) ;
#17503 = EDGE_CURVE ( 'NONE', #9004, #34934, #8823, .T. ) ;
#17504 = EDGE_CURVE ( 'NONE', #24424, #25619, #1385, .T. ) ;
#17505 = VECTOR ( 'NONE', #47485, 999.9999999999998863 ) ;
#17506 = VECTOR ( 'NONE', #30938, 999.9999999999998863 ) ;
#17507 = EDGE_LOOP ( 'NONE', ( #29328, #3109, #7930, #47525 ) ) ;
#17508 = CARTESIAN_POINT ( 'NONE',  ( -17.74404816805336793, 0.000000000000000000, 3.574322630375089460 ) ) ;
#17509 = EDGE_LOOP ( 'NONE', ( #19, #2623, #37926, #20813 ) ) ;
#17510 = ADVANCED_FACE ( 'NONE', ( #53081 ), #26128, .F. ) ;
#17511 = ORIENTED_EDGE ( 'NONE', *, *, #31393, .F. ) ;
#17512 = AXIS2_PLACEMENT_3D ( 'NONE', #22604, #53283, #1279 ) ;
#17513 = AXIS2_PLACEMENT_3D ( 'NONE', #34382, #55670, #42606 ) ;
#17514 = DIRECTION ( 'NONE',  ( 0.000000000000000000, -1.000000000000000000, 0.000000000000000000 ) ) ;
#17515 = DIRECTION ( 'NONE',  ( 0.5449076811759707706, 0.6444004775717708799, -0.5364919789714476250 ) ) ;
#17516 = DIRECTION ( 'NONE',  ( 0.005961354470445682716, -0.6427876096865404731, -0.7660212471507180654 ) ) ;
#17517 = ORIENTED_EDGE ( 'NONE', *, *, #48930, .T. ) ;
#17518 = CARTESIAN_POINT ( 'NONE',  ( -23.23471098716119698, 19.24370920290025566, -4.480780584866845828 ) ) ;
#17519 = ORIENTED_EDGE ( 'NONE', *, *, #4717, .F. ) ;
#17520 = DIRECTION ( 'NONE',  ( 0.7660212471507180654, -0.6427876096865404731, 0.005961354470445141482 ) ) ;
#17521 = VECTOR ( 'NONE', #34093, 999.9999999999998863 ) ;
#17522 = EDGE_CURVE ( 'NONE', #17269, #8995, #43693, .T. ) ;
#17523 = DIRECTION ( 'NONE',  ( -0.005961354470445682716, -0.6427876096865404731, 0.7660212471507180654 ) ) ;
#17524 = VECTOR ( 'NONE', #5697, 999.9999999999998863 ) ;
#17525 = ADVANCED_FACE ( 'NONE', ( #17896 ), #249, .F. ) ;
#17526 = PLANE ( 'NONE',  #6108 ) ;
#17527 = PLANE ( 'NONE',  #8678 ) ;
#17528 = CARTESIAN_POINT ( 'NONE',  ( -16.81345671998191449, 0.000000000000000000, 3.412238694616132495 ) ) ;
#17529 = CARTESIAN_POINT ( 'NONE',  ( -15.96710241509184058, -0.1191753592594218814, 13.13259134697452879 ) ) ;
#17530 = ADVANCED_FACE ( 'NONE', ( #22134 ), #9655, .F. ) ;
#17531 = LINE ( 'NONE', #35415, #51128 ) ;
#17532 = CARTESIAN_POINT ( 'NONE',  ( -16.84587429464891173, -0.1191753592594185784, 6.635972013704265926 ) ) ;
#17533 = ORIENTED_EDGE ( 'NONE', *, *, #51011, .F. ) ;
#17534 = CARTESIAN_POINT ( 'NONE',  ( -56.60431429388330571, 6.503145704592061982, -2.370631253071207922 ) ) ;
#17535 = VECTOR ( 'NONE', #28474, 1000.000000000000227 ) ;
#17536 = EDGE_CURVE ( 'NONE', #29764, #37770, #9343, .T. ) ;
#17537 = DIRECTION ( 'NONE',  ( -0.5449076811759708816, 0.6444004775717707689, 0.5364919789714475140 ) ) ;
#17538 = CARTESIAN_POINT ( 'NONE',  ( -25.20278734466900517, 0.000000000000000000, 6.670939612111840944 ) ) ;
#17539 = PLANE ( 'NONE',  #46246 ) ;
#17540 = VECTOR ( 'NONE', #33823, 1000.000000000000114 ) ;
#17541 = CARTESIAN_POINT ( 'NONE',  ( -17.66651931516290475, 20.72645535605904499, -4.173277724953098122 ) ) ;
#17542 = CARTESIAN_POINT ( 'NONE',  ( -16.06709938707323460, 0.000000000000000000, 13.13181314741652628 ) ) ;
#17543 = EDGE_CURVE ( 'NONE', #13476, #17361, #44285, .T. ) ;
#17544 = CARTESIAN_POINT ( 'NONE',  ( -12.10447826170922880, 0.000000000000000000, 7.311531765476501299 ) ) ;
#17545 = CARTESIAN_POINT ( 'NONE',  ( -10.40437021484443569, 0.000000000000000000, 1.984787408528857489 ) ) ;
#17546 = ITEM_DEFINED_TRANSFORMATION ( 'NONE', 'NONE', #53454,  #2610 ) ;
#17547 = ORIENTED_EDGE ( 'NONE', *, *, #30009, .F. ) ;
#17548 = VECTOR ( 'NONE', #27335, 999.9999999999998863 ) ;
#17549 = CARTESIAN_POINT ( 'NONE',  ( -18.35064882566791411, 3.362543313726510164, 3.702664189482756552 ) ) ;
#17550 = LINE ( 'NONE', #56173, #29444 ) ;
#17551 = CARTESIAN_POINT ( 'NONE',  ( -11.60978317542603300, 0.000000000000000000, 3.452734885371889550 ) ) ;
#17552 = VECTOR ( 'NONE', #46936, 999.9999999999998863 ) ;
#17553 = VECTOR ( 'NONE', #44298, 999.9999999999998863 ) ;
#17554 = CARTESIAN_POINT ( 'NONE',  ( -17.30763713798472025, -0.1191753592594164690, 6.263046398678491222 ) ) ;
#17555 = CARTESIAN_POINT ( 'NONE',  ( -15.13495153988577968, 0.000000000000000000, 12.76973526769478084 ) ) ;
#17556 = DIRECTION ( 'NONE',  ( 0.007781995580012663651, -3.146120232559066537E-19, -0.9999697198139514409 ) ) ;
#17557 = CARTESIAN_POINT ( 'NONE',  ( -56.00000000000000711, 3.800000000000001599, -2.749999999999994671 ) ) ;
#17558 = VECTOR ( 'NONE', #2868, 1000.000000000000227 ) ;
#17559 = PLANE ( 'NONE',  #7662 ) ;
#17560 = VECTOR ( 'NONE', #10513, 1000.000000000000227 ) ;
#17561 = CARTESIAN_POINT ( 'NONE',  ( -15.40103151951671734, 0.000000000000000000, 12.95233060667165681 ) ) ;
#17562 = ORIENTED_EDGE ( 'NONE', *, *, #13032, .T. ) ;
#17563 = CARTESIAN_POINT ( 'NONE',  ( -12.68923408260478958, -0.1941918491731554897, 1.804054826373973519 ) ) ;
#17564 = ORIENTED_EDGE ( 'NONE', *, *, #36014, .T. ) ;
#17565 = ORIENTED_EDGE ( 'NONE', *, *, #17117, .F. ) ;
#17566 = VERTEX_POINT ( 'NONE', #54731 ) ;
#17567 = VERTEX_POINT ( 'NONE', #15295 ) ;
#17568 = VECTOR ( 'NONE', #29026, 1000.000000000000000 ) ;
#17569 = ORIENTED_EDGE ( 'NONE', *, *, #10192, .F. ) ;
#17570 = DIRECTION ( 'NONE',  ( 0.9999697198139515519, 0.000000000000000000, 0.007781995580013368816 ) ) ;
#17571 = CARTESIAN_POINT ( 'NONE',  ( -13.49838895223248336, 0.000000000000000000, 7.300684030172472028 ) ) ;
#17572 = AXIS2_PLACEMENT_3D ( 'NONE', #51871, #30613, #39102 ) ;
#17573 = EDGE_CURVE ( 'NONE', #30957, #2911, #39434, .T. ) ;
#17574 = EDGE_CURVE ( 'NONE', #42137, #31963, #41126, .T. ) ;
#17575 = EDGE_LOOP ( 'NONE', ( #7035, #14878, #31958, #30210 ) ) ;
#17576 = ORIENTED_EDGE ( 'NONE', *, *, #21385, .T. ) ;
#17577 = VECTOR ( 'NONE', #9022, 1000.000000000000114 ) ;
#17578 = ADVANCED_FACE ( 'NONE', ( #32355 ), #54196, .F. ) ;
#17579 = CARTESIAN_POINT ( 'NONE',  ( -66.34585003275293502, 4.336808689942017736E-15, -4.508581566067807245 ) ) ;
#17580 = ORIENTED_EDGE ( 'NONE', *, *, #26772, .T. ) ;
#17581 = VECTOR ( 'NONE', #32108, 1000.000000000000000 ) ;
#17582 = CARTESIAN_POINT ( 'NONE',  ( -19.79569077582305070, 0.000000000000000000, 14.58012466630350445 ) ) ;
#17583 = DIRECTION ( 'NONE',  ( 0.000000000000000000, 0.000000000000000000, 1.000000000000000000 ) ) ;
#17584 = ORIENTED_EDGE ( 'NONE', *, *, #30721, .F. ) ;
#17585 = DIRECTION ( 'NONE',  ( 0.000000000000000000, -1.000000000000000000, 0.000000000000000000 ) ) ;
#17586 = VECTOR ( 'NONE', #55955, 999.9999999999998863 ) ;
#17587 = VERTEX_POINT ( 'NONE', #19550 ) ;
#17588 = LINE ( 'NONE', #8513, #12805 ) ;
#17589 = VECTOR ( 'NONE', #39263, 1000.000000000000227 ) ;
#17590 = LINE ( 'NONE', #20997, #21848 ) ;
#17591 = VECTOR ( 'NONE', #40176, 1000.000000000000227 ) ;
#17592 = VERTEX_POINT ( 'NONE', #6775 ) ;
#17593 = CARTESIAN_POINT ( 'NONE',  ( -18.67619601524082285, 0.000000000000000000, 3.936400510096834893 ) ) ;
#17594 = DIRECTION ( 'NONE',  ( -0.6246952433987893460, -0.7422098413412802076, 0.2426528472758542054 ) ) ;
#17595 = PLANE ( 'NONE',  #3058 ) ;
#17596 = ORIENTED_EDGE ( 'NONE', *, *, #22281, .F. ) ;
#17597 = CARTESIAN_POINT ( 'NONE',  ( -10.68338343524914968, 0.000000000000000000, 3.829276412165673715 ) ) ;
#17598 = ORIENTED_EDGE ( 'NONE', *, *, #55504, .F. ) ;
#17599 = CARTESIAN_POINT ( 'NONE',  ( -14.01545677930355183, 0.000000000000000000, 2.126011111488108174 ) ) ;
#17600 = DIRECTION ( 'NONE',  ( 0.007781995580012663651, 0.000000000000000000, -0.9999697198139515519 ) ) ;
#17601 = DIRECTION ( 'NONE',  ( 0.000000000000000000, -0.000000000000000000, -1.000000000000000000 ) ) ;
#17602 = LINE ( 'NONE', #52523, #26877 ) ;
#17603 = FACE_OUTER_BOUND ( 'NONE', #4261, .T. ) ;
#17604 = EDGE_CURVE ( 'NONE', #50472, #6087, #10761, .T. ) ;
#17605 = LINE ( 'NONE', #4290, #28573 ) ;
#17606 = CARTESIAN_POINT ( 'NONE',  ( -15.83175199606975880, 0.000000000000000000, 8.590527525068505810 ) ) ;
#17607 = VECTOR ( 'NONE', #1018, 1000.000000000000227 ) ;
#17608 = DIRECTION ( 'NONE',  ( -0.9999697198139514409, -0.000000000000000000, -0.007781995580013368816 ) ) ;
#17609 = AXIS2_PLACEMENT_3D ( 'NONE', #4328, #38095, #47459 ) ;
#17610 = EDGE_CURVE ( 'NONE', #48860, #3963, #2507, .T. ) ;
#17611 = CARTESIAN_POINT ( 'NONE',  ( -16.25902619734217680, 0.000000000000000000, 3.785885470949557963 ) ) ;
#17612 = ORIENTED_EDGE ( 'NONE', *, *, #33366, .F. ) ;
#17613 = CARTESIAN_POINT ( 'NONE',  ( -12.53043480859235892, 0.000000000000000000, 2.337573952062577121 ) ) ;
#17615 = EDGE_CURVE ( 'NONE', #40689, #6398, #27508, .T. ) ;
#17614 = PLANE ( 'NONE',  #31802 ) ;
#17616 = VECTOR ( 'NONE', #50698, 1000.000000000000114 ) ;
#17617 = DIRECTION ( 'NONE',  ( 0.007781995580012663651, 0.000000000000000000, -0.9999697198139515519 ) ) ;
#17618 = EDGE_CURVE ( 'NONE', #44660, #34834, #40848, .T. ) ;
#17619 = CARTESIAN_POINT ( 'NONE',  ( -18.81451671468552789, -0.1191753592594156363, 9.205976071834351515 ) ) ;
#17620 = VECTOR ( 'NONE', #36813, 999.9999999999998863 ) ;
#17621 = DIRECTION ( 'NONE',  ( 0.9321478471874541372, 0.000000000000000000, -0.3620778797217453771 ) ) ;
#17622 = FACE_OUTER_BOUND ( 'NONE', #6401, .T. ) ;
#17623 = ORIENTED_EDGE ( 'NONE', *, *, #15586, .F. ) ;
#17624 = VERTEX_POINT ( 'NONE', #1924 ) ;
#17625 = CARTESIAN_POINT ( 'NONE',  ( -21.22452843065813965, -4.727446477803159297, 12.68480442045455803 ) ) ;
#17626 = VECTOR ( 'NONE', #56196, 1000.000000000000227 ) ;
#17627 = LINE ( 'NONE', #38658, #18635 ) ;
#17628 = ORIENTED_EDGE ( 'NONE', *, *, #9707, .F. ) ;
#17629 = VECTOR ( 'NONE', #32357, 999.9999999999998863 ) ;
#17630 = CARTESIAN_POINT ( 'NONE',  ( -19.33760068587298164, 21.49370688441072019, -4.657437592157546824 ) ) ;
#17631 = ORIENTED_EDGE ( 'NONE', *, *, #55195, .T. ) ;
#17632 = FACE_OUTER_BOUND ( 'NONE', #11639, .T. ) ;
#17633 = VERTEX_POINT ( 'NONE', #28069 ) ;
#17634 = DIRECTION ( 'NONE',  ( -0.7660212471507179544, -0.6427876096865405842, -0.005961354470445141482 ) ) ;
#17635 = AXIS2_PLACEMENT_3D ( 'NONE', #19791, #6456, #37112 ) ;
#17636 = EDGE_LOOP ( 'NONE', ( #5700, #20566, #46351, #20762 ) ) ;
#17637 = AXIS2_PLACEMENT_3D ( 'NONE', #5214, #22785, #1192 ) ;
#17638 = EDGE_LOOP ( 'NONE', ( #13724, #51067, #20497, #31893 ) ) ;
#17639 = ORIENTED_EDGE ( 'NONE', *, *, #2171, .T. ) ;
#17640 = DIRECTION ( 'NONE',  ( 0.000000000000000000, 1.000000000000000000, 0.000000000000000000 ) ) ;
#17641 = DIRECTION ( 'NONE',  ( 0.6427681459581294776, -0.7660444431189769032, 0.005002170337467562802 ) ) ;
#17642 = LINE ( 'NONE', #34983, #34817 ) ;
#17643 = EDGE_CURVE ( 'NONE', #24619, #55170, #36589, .T. ) ;
#17644 = CARTESIAN_POINT ( 'NONE',  ( -25.20123094555300369, 0.000000000000000000, 6.470945668149052032 ) ) ;
#17645 = ORIENTED_EDGE ( 'NONE', *, *, #8915, .F. ) ;
#17646 = ORIENTED_EDGE ( 'NONE', *, *, #26995, .T. ) ;
#17647 = EDGE_CURVE ( 'NONE', #2654, #51468, #20082, .T. ) ;
#17648 = EDGE_CURVE ( 'NONE', #13341, #41874, #19827, .T. ) ;
#17649 = AXIS2_PLACEMENT_3D ( 'NONE', #21804, #35181, #39126 ) ;
#17650 = ORIENTED_EDGE ( 'NONE', *, *, #28887, .F. ) ;
#17651 = CARTESIAN_POINT ( 'NONE',  ( -11.20636620717317378, 0.000000000000000000, 11.32298014792380414 ) ) ;
#17652 = AXIS2_PLACEMENT_3D ( 'NONE', #9127, #30728, #48030 ) ;
#17653 = VERTEX_POINT ( 'NONE', #6489 ) ;
#17654 = CARTESIAN_POINT ( 'NONE',  ( -10.69200559576499643, 0.000000000000000000, 4.937205521938968111 ) ) ;
#17655 = VERTEX_POINT ( 'NONE', #54445 ) ;
#17656 = CIRCLE ( 'NONE', #52107, 0.5000000000000004441 ) ;
#17657 = CARTESIAN_POINT ( 'NONE',  ( -29.86352658060627618, 0.000000000000000000, 8.481329010720569883 ) ) ;
#17658 = CARTESIAN_POINT ( 'NONE',  ( -22.56675936406184135, 4.495856970884013037, 5.304186063099788129 ) ) ;
#17659 = ORIENTED_EDGE ( 'NONE', *, *, #11979, .T. ) ;
#17660 = DIRECTION ( 'NONE',  ( -0.5449076811759708816, 0.6444004775717707689, 0.5364919789714475140 ) ) ;
#17661 = VECTOR ( 'NONE', #40296, 999.9999999999998863 ) ;
#17662 = ORIENTED_EDGE ( 'NONE', *, *, #29274, .F. ) ;
#17663 = ADVANCED_FACE ( 'NONE', ( #11013 ), #2800, .T. ) ;
#17664 = DIRECTION ( 'NONE',  ( 0.000000000000000000, -1.000000000000000000, 0.000000000000000000 ) ) ;
#17665 = AXIS2_PLACEMENT_3D ( 'NONE', #37874, #16267, #34180 ) ;
#17666 = ORIENTED_EDGE ( 'NONE', *, *, #31775, .F. ) ;
#17667 = DIRECTION ( 'NONE',  ( 0.000000000000000000, -1.000000000000000000, 0.000000000000000000 ) ) ;
#17668 = DIRECTION ( 'NONE',  ( -0.005002170337468016433, -0.7660444431189770143, 0.6427681459581293666 ) ) ;
#17669 = VECTOR ( 'NONE', #31432, 999.9999999999998863 ) ;
#17670 = LINE ( 'NONE', #48305, #26451 ) ;
#17671 = ORIENTED_EDGE ( 'NONE', *, *, #33306, .T. ) ;
#17672 = VECTOR ( 'NONE', #22451, 999.9999999999998863 ) ;
#17673 = LINE ( 'NONE', #17372, #15660 ) ;
#17674 = LINE ( 'NONE', #333, #12855 ) ;
#17675 = CARTESIAN_POINT ( 'NONE',  ( -21.17884633731301136, -1.975113310420658852, 5.044887815787086893 ) ) ;
#17676 = PLANE ( 'NONE',  #52241 ) ;
#17677 = CARTESIAN_POINT ( 'NONE',  ( -15.54256021603320015, 0.000000000000000000, 5.438115467695609162 ) ) ;
#17678 = DIRECTION ( 'NONE',  ( -0.005961354470445682716, -0.6427876096865404731, 0.7660212471507180654 ) ) ;
#17679 = VECTOR ( 'NONE', #41012, 999.9999999999998863 ) ;
#17680 = VECTOR ( 'NONE', #415, 1000.000000000000227 ) ;
#17681 = CARTESIAN_POINT ( 'NONE',  ( -9.751235588061692994, 0.000000000000000000, 3.467198532443927839 ) ) ;
#17682 = ORIENTED_EDGE ( 'NONE', *, *, #11928, .T. ) ;
#17683 = CARTESIAN_POINT ( 'NONE',  ( -16.82862997361721824, -0.1191753592594196748, 4.420113794157683351 ) ) ;
#17684 = CARTESIAN_POINT ( 'NONE',  ( -14.97583049326344096, -0.1191753592594192307, 5.173196847745247240 ) ) ;
#17685 = CARTESIAN_POINT ( 'NONE',  ( -19.22961988024793101, -0.1191753592594177458, 14.39986392600063603 ) ) ;
#17686 = EDGE_LOOP ( 'NONE', ( #26356, #6686, #5238, #4459 ) ) ;
#17687 = PLANE ( 'NONE',  #21155 ) ;
#17688 = CARTESIAN_POINT ( 'NONE',  ( -16.08055152492125828, 1.743523803501506819, 5.988973023155203634 ) ) ;
#17689 = VERTEX_POINT ( 'NONE', #1666 ) ;
#17690 = DIRECTION ( 'NONE',  ( 0.7660212471507180654, -0.6427876096865404731, 0.005961354470445141482 ) ) ;
#17691 = EDGE_CURVE ( 'NONE', #14368, #26120, #18994, .T. ) ;
#17692 = LINE ( 'NONE', #31603, #41142 ) ;
#17693 = DIRECTION ( 'NONE',  ( 0.005961354470445682716, -0.6427876096865404731, -0.7660212471507180654 ) ) ;
#17694 = PLANE ( 'NONE',  #33826 ) ;
#17695 = AXIS2_PLACEMENT_3D ( 'NONE', #5829, #10670, #27694 ) ;
#17696 = ORIENTED_EDGE ( 'NONE', *, *, #29936, .T. ) ;
#17697 = ORIENTED_EDGE ( 'NONE', *, *, #54517, .F. ) ;
#17698 = DIRECTION ( 'NONE',  ( 0.007781995580012663651, 0.000000000000000000, -0.9999697198139515519 ) ) ;
#17699 = FACE_OUTER_BOUND ( 'NONE', #49771, .T. ) ;
#17700 = CARTESIAN_POINT ( 'NONE',  ( -11.62990154996301051, 0.000000000000000000, 6.037902808176242253 ) ) ;
#17701 = VECTOR ( 'NONE', #14736, 999.9999999999998863 ) ;
#17702 = ADVANCED_FACE ( 'NONE', ( #14728 ), #32053, .F. ) ;
#17703 = CARTESIAN_POINT ( 'NONE',  ( -13.12015695940438320, -0.1191753592594174960, 5.556970198075047662 ) ) ;
#17704 = CARTESIAN_POINT ( 'NONE',  ( -12.60458797795435615, 0.000000000000000000, 11.86609696750642229 ) ) ;
#17705 = PLANE ( 'NONE',  #48485 ) ;
#17706 = VECTOR ( 'NONE', #25624, 999.9999999999998863 ) ;
#17708 = ADVANCED_FACE ( 'NONE', ( #7601 ), #20678, .F. ) ;
#17707 = VERTEX_POINT ( 'NONE', #7912 ) ;
#17709 = DIRECTION ( 'NONE',  ( -0.6246952433987893460, -0.7422098413412802076, 0.2426528472758542054 ) ) ;
#17710 = ADVANCED_FACE ( 'NONE', ( #24629 ), #34305, .F. ) ;
#17711 = PLANE ( 'NONE',  #9731 ) ;
#17712 = VECTOR ( 'NONE', #25144, 1000.000000000000114 ) ;
#17714 = ORIENTED_EDGE ( 'NONE', *, *, #1624, .T. ) ;
#17713 = PRESENTATION_LAYER_ASSIGNMENT (  '', '', ( #18602 ) ) ;
#17715 = VECTOR ( 'NONE', #3442, 1000.000000000000000 ) ;
#17716 = CARTESIAN_POINT ( 'NONE',  ( -15.36424104572339289, 0.000000000000000000, 8.224833733578753581 ) ) ;
#17717 = EDGE_CURVE ( 'NONE', #46531, #23582, #55883, .T. ) ;
#17718 = CARTESIAN_POINT ( 'NONE',  ( -9.110551994824897193, -1.000000000000000000, 3.538847790438064411 ) ) ;
#17719 = DIRECTION ( 'NONE',  ( 0.5364919789714477361, 0.6444004775717706579, 0.5449076811759711036 ) ) ;
#17720 = VECTOR ( 'NONE', #9880, 999.9999999999998863 ) ;
#17721 = ORIENTED_EDGE ( 'NONE', *, *, #52374, .T. ) ;
#17722 = VECTOR ( 'NONE', #30377, 999.9999999999998863 ) ;
#17723 = CARTESIAN_POINT ( 'NONE',  ( -20.66714045964585722, 20.62987310936006224, -4.333808234692209105 ) ) ;
#17724 = EDGE_CURVE ( 'NONE', #16052, #28453, #29476, .T. ) ;
#17725 = VERTEX_POINT ( 'NONE', #41944 ) ;
#17726 = ADVANCED_FACE ( 'NONE', ( #37993 ), #38844, .F. ) ;
#17727 = VECTOR ( 'NONE', #51583, 999.9999999999998863 ) ;
#17728 = ORIENTED_EDGE ( 'NONE', *, *, #4489, .F. ) ;
#17729 = AXIS2_PLACEMENT_3D ( 'NONE', #49234, #10352, #27673 ) ;
#17730 = ORIENTED_EDGE ( 'NONE', *, *, #40678, .T. ) ;
#17731 = ORIENTED_EDGE ( 'NONE', *, *, #41453, .T. ) ;
#17732 = LINE ( 'NONE', #38762, #40232 ) ;
#17733 = ORIENTED_EDGE ( 'NONE', *, *, #8388, .T. ) ;
#17734 = CARTESIAN_POINT ( 'NONE',  ( 1.086233639165236964, 0.000000000000000000, 2.796443541562362078 ) ) ;
#17735 = EDGE_CURVE ( 'NONE', #25817, #9694, #50500, .T. ) ;
#17736 = VERTEX_POINT ( 'NONE', #42790 ) ;
#17737 = CARTESIAN_POINT ( 'NONE',  ( -26.26580391614848864, 17.49370688441070953, -4.657437592157546824 ) ) ;
#17738 = ORIENTED_EDGE ( 'NONE', *, *, #23359, .T. ) ;
#17739 = DIRECTION ( 'NONE',  ( -0.6427681459581293666, -0.7660444431189770143, -0.005002170337467561935 ) ) ;
#17740 = EDGE_LOOP ( 'NONE', ( #27708, #44173, #148, #14004 ) ) ;
#17741 = AXIS2_PLACEMENT_3D ( 'NONE', #34453, #13450, #30500 ) ;
#17742 = EDGE_CURVE ( 'NONE', #20003, #16426, #8444, .T. ) ;
#17743 = CARTESIAN_POINT ( 'NONE',  ( -19.77061338776520216, 21.24370688441071664, 4.270755533188014930 ) ) ;
#17744 = AXIS2_PLACEMENT_3D ( 'NONE', #13389, #35249, #858 ) ;
#17745 = LINE ( 'NONE', #34485, #4180 ) ;
#17746 = DIRECTION ( 'NONE',  ( 0.007781995580012663651, 0.000000000000000000, -0.9999697198139515519 ) ) ;
#17747 = LINE ( 'NONE', #9797, #35087 ) ;
#17748 = CARTESIAN_POINT ( 'NONE',  ( -19.37194182085847416, -1.489407457353156827, 4.358521298522645360 ) ) ;
#17749 = AXIS2_PLACEMENT_3D ( 'NONE', #17389, #8056, #43272 ) ;
#17750 = EDGE_LOOP ( 'NONE', ( #28032, #9883, #44271, #30390 ) ) ;
#17751 = VERTEX_POINT ( 'NONE', #33181 ) ;
#17752 = DIRECTION ( 'NONE',  ( 0.007781995580012663651, -3.146120232559066537E-19, -0.9999697198139514409 ) ) ;
#17753 = CARTESIAN_POINT ( 'NONE',  ( -10.23311680593447193, 0.000000000000000000, 5.679440840222505393 ) ) ;
#17754 = VECTOR ( 'NONE', #32675, 1000.000000000000227 ) ;
#17755 = CARTESIAN_POINT ( 'NONE',  ( -13.04747015058856618, -5.051250379848164940, 1.788240284305238070 ) ) ;
#17756 = VECTOR ( 'NONE', #55423, 1000.000000000000000 ) ;
#17757 = AXIS2_PLACEMENT_3D ( 'NONE', #23930, #6344, #15157 ) ;
#17758 = DIRECTION ( 'NONE',  ( -0.9999697198139514409, -0.000000000000000000, -0.007781995580013368816 ) ) ;
#17759 = CARTESIAN_POINT ( 'NONE',  ( -11.40636015113596180, 0.000000000000000000, 11.32142374880780089 ) ) ;
#17760 = DIRECTION ( 'NONE',  ( 0.5449076811759707706, 0.6444004775717708799, -0.5364919789714476250 ) ) ;
#17761 = EDGE_LOOP ( 'NONE', ( #36576, #8990, #43974, #33579, #44151, #28766, #16586, #48595, #5862, #32120 ) ) ;
#17762 = DIRECTION ( 'NONE',  ( 0.000000000000000000, -1.000000000000000000, 0.000000000000000000 ) ) ;
#17763 = PLANE ( 'NONE',  #8628 ) ;
#17764 = VERTEX_POINT ( 'NONE', #51340 ) ;
#17765 = AXIS2_PLACEMENT_3D ( 'NONE', #14895, #36763, #31928 ) ;
#17766 = DIRECTION ( 'NONE',  ( 0.9999697198139515519, 0.000000000000000000, 0.007781995580013368816 ) ) ;
#17767 = CARTESIAN_POINT ( 'NONE',  ( -12.07442007226712199, 0.000000000000000000, 3.449118973603880978 ) ) ;
#17768 = VECTOR ( 'NONE', #47118, 1000.000000000000000 ) ;
#17769 = VECTOR ( 'NONE', #50077, 1000.000000000000114 ) ;
#17770 = EDGE_CURVE ( 'NONE', #30294, #26568, #24933, .T. ) ;
#17771 = LINE ( 'NONE', #17463, #25959 ) ;
#17772 = CARTESIAN_POINT ( 'NONE',  ( -12.66701627658442497, -0.1191753592594181482, 7.037824922874117206 ) ) ;
#17773 = AXIS2_PLACEMENT_3D ( 'NONE', #9465, #4385, #10025 ) ;
#17774 = CARTESIAN_POINT ( 'NONE',  ( -20.54049170961573267, 0.000000000000000000, 4.660556269540326646 ) ) ;
#17775 = VERTEX_POINT ( 'NONE', #3623 ) ;
#17776 = VECTOR ( 'NONE', #15500, 1000.000000000000227 ) ;
#17777 = ORIENTED_EDGE ( 'NONE', *, *, #204, .F. ) ;
#17778 = FACE_OUTER_BOUND ( 'NONE', #47424, .T. ) ;
#17779 = PLANE ( 'NONE',  #24057 ) ;
#17780 = CARTESIAN_POINT ( 'NONE',  ( -20.54126990917373519, -0.1191753592594197858, 4.760553241521720658 ) ) ;
#17781 = CARTESIAN_POINT ( 'NONE',  ( 0.3240706152708093812, -3.670543518250628967, -1.335466778558061241E-15 ) ) ;
#17782 = CARTESIAN_POINT ( 'NONE',  ( -18.64035723371328857, -5.051250379848164940, 3.960707562635710666 ) ) ;
#17783 = DIRECTION ( 'NONE',  ( 0.000000000000000000, -1.000000000000000000, 0.000000000000000000 ) ) ;
#17784 = FACE_OUTER_BOUND ( 'NONE', #47978, .T. ) ;
#17786 = ADVANCED_FACE ( 'NONE', ( #37721 ), #7314, .F. ) ;
#17785 = ORIENTED_EDGE ( 'NONE', *, *, #53040, .T. ) ;
#17787 = AXIS2_PLACEMENT_3D ( 'NONE', #18529, #24454, #12244 ) ;
#17788 = LINE ( 'NONE', #987, #20529 ) ;
#17789 = DIRECTION ( 'NONE',  ( 0.9999697198139515519, 0.000000000000000000, 0.007781995580013368816 ) ) ;
#17790 = VERTEX_POINT ( 'NONE', #43099 ) ;
#17791 = CARTESIAN_POINT ( 'NONE',  ( -10.74029228357944987, 0.000000000000000000, 11.14194120806293320 ) ) ;
#17792 = ORIENTED_EDGE ( 'NONE', *, *, #52367, .F. ) ;
#17793 = PLANE ( 'NONE',  #51328 ) ;
#17794 = VECTOR ( 'NONE', #27373, 1000.000000000000227 ) ;
#17795 = CARTESIAN_POINT ( 'NONE',  ( -18.10035294465630074, -4.889348428825659454, 11.73697724819580657 ) ) ;
#17796 = EDGE_LOOP ( 'NONE', ( #15475, #37880, #5698 ) ) ;
#17797 = ADVANCED_FACE ( 'NONE', ( #28913 ), #12711, .F. ) ;
#17798 = VECTOR ( 'NONE', #40859, 1000.000000000000000 ) ;
#17799 = ORIENTED_EDGE ( 'NONE', *, *, #23243, .F. ) ;
#17800 = EDGE_CURVE ( 'NONE', #7467, #25938, #55577, .T. ) ;
#17801 = ORIENTED_EDGE ( 'NONE', *, *, #36617, .F. ) ;
#17802 = AXIS2_PLACEMENT_3D ( 'NONE', #46807, #47079, #42265 ) ;
#17803 = VERTEX_POINT ( 'NONE', #8173 ) ;
#17804 = AXIS2_PLACEMENT_3D ( 'NONE', #16836, #55721, #16255 ) ;
#17805 = ORIENTED_EDGE ( 'NONE', *, *, #17022, .T. ) ;
#17806 = EDGE_LOOP ( 'NONE', ( #38176, #2686, #6580, #33348 ) ) ;
#17807 = LINE ( 'NONE', #42768, #25916 ) ;
#17808 = DIRECTION ( 'NONE',  ( 0.000000000000000000, -1.000000000000000000, 0.000000000000000000 ) ) ;
#17809 = CARTESIAN_POINT ( 'NONE',  ( 4.848100717410754434, 0.000000000000000000, -2.061810099490656079 ) ) ;
#17810 = AXIS2_PLACEMENT_3D ( 'NONE', #54465, #50218, #11329 ) ;
#17811 = ADVANCED_FACE ( 'NONE', ( #25482 ), #3896, .F. ) ;
#17812 = VECTOR ( 'NONE', #25761, 1000.000000000000227 ) ;
#17813 = EDGE_LOOP ( 'NONE', ( #50122, #34671, #47693, #23003 ) ) ;
#17814 = CARTESIAN_POINT ( 'NONE',  ( -20.61943528392893654, -4.079838673713161334, 4.760441806437299306 ) ) ;
#17815 = EDGE_LOOP ( 'NONE', ( #38884, #34750, #45444, #29862 ) ) ;
#17816 = VERTEX_POINT ( 'NONE', #30029 ) ;
#17817 = AXIS2_PLACEMENT_3D ( 'NONE', #20776, #55143, #42371 ) ;
#17818 = EDGE_CURVE ( 'NONE', #29996, #7048, #38554, .T. ) ;
#17819 = VECTOR ( 'NONE', #46364, 1000.000000000000227 ) ;
#17820 = CARTESIAN_POINT ( 'NONE',  ( -8.875996589204540044, 0.000000000000000000, 10.41778544861944233 ) ) ;
#17821 = DIRECTION ( 'NONE',  ( 0.6427681459581294776, -0.7660444431189769032, 0.005002170337467562802 ) ) ;
#17822 = FACE_OUTER_BOUND ( 'NONE', #16800, .T. ) ;
#17823 = EDGE_LOOP ( 'NONE', ( #9827, #50233, #13075, #2421 ) ) ;
#17824 = DIRECTION ( 'NONE',  ( -0.9999697198139514409, -0.000000000000000000, -0.007781995580013368816 ) ) ;
#17825 = ORIENTED_EDGE ( 'NONE', *, *, #12944, .T. ) ;
#17826 = CARTESIAN_POINT ( 'NONE',  ( -21.70925593905789341, -5.375054281893165253, 5.142441000255496775 ) ) ;
#17827 = CARTESIAN_POINT ( 'NONE',  ( -1.148446742091705719, -6.446785546503744690, 3.664469291707747267 ) ) ;
#17828 = VECTOR ( 'NONE', #14627, 1000.000000000000227 ) ;
#17829 = DIRECTION ( 'NONE',  ( 0.9999697198139515519, 0.000000000000000000, 0.007781995580013368816 ) ) ;
#17830 = FACE_OUTER_BOUND ( 'NONE', #35906, .T. ) ;
#17831 = DIRECTION ( 'NONE',  ( 0.5449076811759707706, 0.6444004775717708799, -0.5364919789714476250 ) ) ;
#17832 = FACE_OUTER_BOUND ( 'NONE', #17074, .T. ) ;
#17833 = CARTESIAN_POINT ( 'NONE',  ( -19.22961988024793101, -0.1191753592594177458, 14.39986392600063603 ) ) ;
#17834 = VERTEX_POINT ( 'NONE', #15840 ) ;
#17835 = LINE ( 'NONE', #52179, #41924 ) ;
#17836 = VECTOR ( 'NONE', #21609, 1000.000000000000227 ) ;
#17837 = EDGE_CURVE ( 'NONE', #54540, #20884, #33450, .T. ) ;
#17838 = DIRECTION ( 'NONE',  ( 0.005002170337468016433, -0.7660444431189770143, -0.6427681459581293666 ) ) ;
#17839 = FACE_OUTER_BOUND ( 'NONE', #29934, .T. ) ;
#17841 = DIRECTION ( 'NONE',  ( -0.005961354470445682716, -0.6427876096865404731, 0.7660212471507180654 ) ) ;
#17840 = VECTOR ( 'NONE', #35569, 999.9999999999998863 ) ;
#17842 = EDGE_CURVE ( 'NONE', #41679, #39446, #35696, .T. ) ;
#17843 = CARTESIAN_POINT ( 'NONE',  ( -21.95272886865376094, 18.25181111654794108, -4.454155209268523485 ) ) ;
#17844 = FACE_OUTER_BOUND ( 'NONE', #36144, .T. ) ;
#17845 = CARTESIAN_POINT ( 'NONE',  ( -17.93139508144814442, 0.000000000000000000, 13.85596890686001537 ) ) ;
#17846 = VECTOR ( 'NONE', #16625, 1000.000000000000114 ) ;
#17847 = DIRECTION ( 'NONE',  ( -0.5449076811759708816, 0.6444004775717707689, 0.5364919789714475140 ) ) ;
#17848 = ADVANCED_FACE ( 'NONE', ( #30866 ), #44227, .F. ) ;
#17849 = VERTEX_POINT ( 'NONE', #9869 ) ;
#17850 = EDGE_CURVE ( 'NONE', #1909, #49895, #22069, .T. ) ;
#17851 = CARTESIAN_POINT ( 'NONE',  ( -14.89673009537702697, 0.000000000000000000, 7.859139942088997799 ) ) ;
#17852 = CARTESIAN_POINT ( 'NONE',  ( -12.97782006657300258, 4.657758921906509642, 9.566523066637216743 ) ) ;
#17853 = PLANE ( 'NONE',  #23681 ) ;
#17854 = ADVANCED_FACE ( 'NONE', ( #17830 ), #39945, .F. ) ;
#17855 = EDGE_CURVE ( 'NONE', #34917, #44182, #26322, .T. ) ;
#17856 = EDGE_CURVE ( 'NONE', #49471, #46628, #22374, .T. ) ;
#17857 = VECTOR ( 'NONE', #23940, 1000.000000000000114 ) ;
#17858 = LINE ( 'NONE', #25798, #34568 ) ;
#17859 = CARTESIAN_POINT ( 'NONE',  ( -2.056461029976381472, 6.659969651376628441, 4.017172877417169552 ) ) ;
#17860 = CARTESIAN_POINT ( 'NONE',  ( -27.06552663992790997, 0.000000000000000000, 7.195101427592543786 ) ) ;
#17861 = CARTESIAN_POINT ( 'NONE',  ( 2.072287782118878319, 0.000000000000000000, -2.950529333540147015 ) ) ;
#17862 = VECTOR ( 'NONE', #45109, 1000.000000000000227 ) ;
#17863 = VECTOR ( 'NONE', #28430, 999.9999999999998863 ) ;
#17864 = DIRECTION ( 'NONE',  ( -0.005002170337468016433, -0.7660444431189770143, 0.6427681459581293666 ) ) ;
#17865 = LINE ( 'NONE', #35730, #35592 ) ;
#17866 = VERTEX_POINT ( 'NONE', #182 ) ;
#17867 = ADVANCED_FACE ( 'NONE', ( #35160 ), #39690, .F. ) ;
#17868 = AXIS2_PLACEMENT_3D ( 'NONE', #46027, #15103, #10576 ) ;
#17869 = EDGE_CURVE ( 'NONE', #17442, #47891, #53014, .T. ) ;
#17870 = VERTEX_POINT ( 'NONE', #769 ) ;
#17871 = EDGE_LOOP ( 'NONE', ( #52931, #33939, #1916, #16372 ) ) ;
#17872 = ORIENTED_EDGE ( 'NONE', *, *, #44141, .T. ) ;
#17873 = EDGE_CURVE ( 'NONE', #13581, #2493, #44478, .T. ) ;
#17874 = ORIENTED_EDGE ( 'NONE', *, *, #43846, .F. ) ;
#17875 = CARTESIAN_POINT ( 'NONE',  ( -11.64230387957660007, -1.165603555308156514, 1.366398462294132532 ) ) ;
#17876 = DIRECTION ( 'NONE',  ( -0.9999697198139514409, -0.000000000000000000, -0.007781995580013368816 ) ) ;
#17877 = ADVANCED_FACE ( 'NONE', ( #22910 ), #17527, .F. ) ;
#17878 = ORIENTED_EDGE ( 'NONE', *, *, #50465, .T. ) ;
#17879 = VECTOR ( 'NONE', #7495, 1000.000000000000000 ) ;
#17880 = ORIENTED_EDGE ( 'NONE', *, *, #41307, .F. ) ;
#17881 = VECTOR ( 'NONE', #39638, 1000.000000000000227 ) ;
#17882 = DIRECTION ( 'NONE',  ( -0.005961354470445682716, -0.6427876096865404731, 0.7660212471507180654 ) ) ;
#17883 = EDGE_LOOP ( 'NONE', ( #40277, #37006, #30604, #53981 ) ) ;
#17884 = CARTESIAN_POINT ( 'NONE',  ( -18.27257916373564228, 1.581621852479005552, 6.574722315692204333 ) ) ;
#17885 = FACE_OUTER_BOUND ( 'NONE', #48939, .T. ) ;
#17886 = EDGE_CURVE ( 'NONE', #46046, #31141, #30618, .T. ) ;
#17887 = ORIENTED_EDGE ( 'NONE', *, *, #9094, .T. ) ;
#17888 = PLANE ( 'NONE',  #24770 ) ;
#17889 = ORIENTED_EDGE ( 'NONE', *, *, #36821, .F. ) ;
#17890 = VECTOR ( 'NONE', #30315, 999.9999999999998863 ) ;
#17891 = CARTESIAN_POINT ( 'NONE',  ( -18.67062061514484483, -0.1191753592594160666, 9.576427974360404605 ) ) ;
#17892 = LINE ( 'NONE', #53620, #35474 ) ;
#17893 = DIRECTION ( 'NONE',  ( 0.7660212471507180654, -0.6427876096865404731, 0.005961354470445141482 ) ) ;
#17894 = VECTOR ( 'NONE', #20828, 999.9999999999998863 ) ;
#17895 = ORIENTED_EDGE ( 'NONE', *, *, #33598, .T. ) ;
#17896 = FACE_OUTER_BOUND ( 'NONE', #31112, .T. ) ;
#17897 = CARTESIAN_POINT ( 'NONE',  ( -14.00280974873554030, 0.000000000000000000, 12.40921378708904044 ) ) ;
#17898 = CARTESIAN_POINT ( 'NONE',  ( -14.93495759592298988, 0.000000000000000000, 12.77129166681078409 ) ) ;
#17899 = ORIENTED_EDGE ( 'NONE', *, *, #55593, .T. ) ;
#17900 = DIRECTION ( 'NONE',  ( -0.3583679495452941621, -0.9335804264972042965, 0.000000000000000000 ) ) ;
#17901 = VERTEX_POINT ( 'NONE', #17239 ) ;
#17902 = LINE ( 'NONE', #22446, #19287 ) ;
#17903 = LINE ( 'NONE', #43701, #40535 ) ;
#17904 = DIRECTION ( 'NONE',  ( -0.005961354470445682716, -0.6427876096865404731, 0.7660212471507180654 ) ) ;
#17905 = CARTESIAN_POINT ( 'NONE',  ( -61.74810725808001877, 6.470640170577544481, 2.999999999999993339 ) ) ;
#17906 = CARTESIAN_POINT ( 'NONE',  ( -11.67244013076689946, 0.000000000000000000, 11.50401908778467863 ) ) ;
#17907 = DIRECTION ( 'NONE',  ( 0.005002170337468016433, -0.7660444431189770143, -0.6427681459581293666 ) ) ;
#17908 = PLANE ( 'NONE',  #47017 ) ;
#17909 = FACE_OUTER_BOUND ( 'NONE', #17434, .T. ) ;
#17910 = DIRECTION ( 'NONE',  ( 0.005002170337468016433, -0.7660444431189770143, -0.6427681459581293666 ) ) ;
#17911 = ORIENTED_EDGE ( 'NONE', *, *, #5531, .T. ) ;
#17912 = FACE_OUTER_BOUND ( 'NONE', #6209, .T. ) ;
#17913 = CARTESIAN_POINT ( 'NONE',  ( -12.60458797795435615, 0.000000000000000000, 11.86609696750642229 ) ) ;
#17914 = LINE ( 'NONE', #52535, #35989 ) ;
#17915 = EDGE_CURVE ( 'NONE', #30544, #36108, #13820, .T. ) ;
#17916 = EDGE_CURVE ( 'NONE', #31662, #29422, #12993, .T. ) ;
#17917 = LINE ( 'NONE', #52801, #995 ) ;
#17918 = ADVANCED_FACE ( 'NONE', ( #43383 ), #4478, .F. ) ;
#17919 = DIRECTION ( 'NONE',  ( 0.007781995580012663651, -3.146120232559066537E-19, -0.9999697198139514409 ) ) ;
#17920 = CARTESIAN_POINT ( 'NONE',  ( 5.577510371788089394, -6.223674869166635482, -2.393421119419574250 ) ) ;
#17921 = VERTEX_POINT ( 'NONE', #52173 ) ;
#17922 = VECTOR ( 'NONE', #33899, 1000.000000000000227 ) ;
#17923 = VERTEX_POINT ( 'NONE', #13289 ) ;
#17924 = DIRECTION ( 'NONE',  ( -0.6427681459581293666, -0.7660444431189770143, -0.005002170337467561935 ) ) ;
#17925 = DIRECTION ( 'NONE',  ( 0.6427681459581294776, -0.7660444431189769032, 0.005002170337467562802 ) ) ;
#17926 = B_SPLINE_CURVE_WITH_KNOTS ( 'NONE', 3,
 ( #10356, #53505, #15186, #5816 ),
 .UNSPECIFIED., .F., .F.,
 ( 4, 4 ),
 ( 0.4250098312019520708, 0.4483797419119410210 ),
 .UNSPECIFIED. ) ;
#17927 = VECTOR ( 'NONE', #50051, 1000.000000000000227 ) ;
#17928 = ORIENTED_EDGE ( 'NONE', *, *, #51577, .F. ) ;
#17929 = CARTESIAN_POINT ( 'NONE',  ( -50.27554558092695913, 4.209026340267034705, -5.000000000000000000 ) ) ;
#17930 = ORIENTED_EDGE ( 'NONE', *, *, #16034, .F. ) ;
#17931 = LINE ( 'NONE', #35254, #27474 ) ;
#17932 = EDGE_CURVE ( 'NONE', #38002, #50731, #47921, .T. ) ;
#17933 = ORIENTED_EDGE ( 'NONE', *, *, #26576, .T. ) ;
#17934 = ORIENTED_EDGE ( 'NONE', *, *, #42322, .T. ) ;
#17935 = EDGE_LOOP ( 'NONE', ( #48636, #52793, #38205, #19238 ) ) ;
#17936 = EDGE_CURVE ( 'NONE', #11344, #30222, #43635, .T. ) ;
#17937 = FACE_OUTER_BOUND ( 'NONE', #11276, .T. ) ;
#17938 = CARTESIAN_POINT ( 'NONE',  ( -28.93137873341882127, 0.000000000000000000, 8.119251130998824451 ) ) ;
#17939 = FACE_OUTER_BOUND ( 'NONE', #14859, .T. ) ;
#17940 = EDGE_CURVE ( 'NONE', #32323, #25140, #3208, .T. ) ;
#17941 = CARTESIAN_POINT ( 'NONE',  ( -12.15193928448664629, -0.1191753592594197858, 1.501852324026012209 ) ) ;
#17942 = ORIENTED_EDGE ( 'NONE', *, *, #37587, .F. ) ;
#17943 = VERTEX_POINT ( 'NONE', #1868 ) ;
#17944 = CARTESIAN_POINT ( 'NONE',  ( -16.96389378722000529, 0.000000000000000000, 8.951049005674249770 ) ) ;
#17945 = ORIENTED_EDGE ( 'NONE', *, *, #46452, .F. ) ;
#17946 = DIRECTION ( 'NONE',  ( 0.005961354470445682716, -0.6427876096865404731, -0.7660212471507180654 ) ) ;
#17947 = EDGE_CURVE ( 'NONE', #34394, #24292, #29332, .T. ) ;
#17948 = ORIENTED_EDGE ( 'NONE', *, *, #14097, .T. ) ;
#17949 = DIRECTION ( 'NONE',  ( -0.5364919789714478471, 0.6444004775717705469, -0.5449076811759709926 ) ) ;
#17950 = ORIENTED_EDGE ( 'NONE', *, *, #21508, .F. ) ;
#17951 = CARTESIAN_POINT ( 'NONE',  ( -12.10724190330752315, -2.784623065533159636, 5.954836501472268395 ) ) ;
#17952 = ORIENTED_EDGE ( 'NONE', *, *, #15636, .T. ) ;
#17953 = CARTESIAN_POINT ( 'NONE',  ( 2.072287782118878319, 0.000000000000000000, -2.950529333540147015 ) ) ;
#17954 = ORIENTED_EDGE ( 'NONE', *, *, #9197, .F. ) ;
#17955 = DIRECTION ( 'NONE',  ( 0.007781995580012663651, 0.000000000000000000, -0.9999697198139515519 ) ) ;
#17956 = CARTESIAN_POINT ( 'NONE',  ( -17.31338524499528830, -0.1191753592594166911, 7.001665805194019043 ) ) ;
#17957 = DIRECTION ( 'NONE',  ( -0.7660212471507179544, -0.6427876096865405842, -0.005961354470445141482 ) ) ;
#17958 = ORIENTED_EDGE ( 'NONE', *, *, #18569, .T. ) ;
#17959 = DIRECTION ( 'NONE',  ( -0.9999697198139514409, -0.000000000000000000, -0.007781995580013368816 ) ) ;
#17960 = VECTOR ( 'NONE', #55176, 1000.000000000000227 ) ;
#17961 = DIRECTION ( 'NONE',  ( 0.7660212471507180654, -0.6427876096865404731, 0.005961354470445141482 ) ) ;
#17962 = CARTESIAN_POINT ( 'NONE',  ( -70.00259797851279586, 0.1329035588801656675, 7.501778215771297553 ) ) ;
#17963 = DIRECTION ( 'NONE',  ( 0.007781995580012663651, 0.000000000000000000, -0.9999697198139515519 ) ) ;
#17964 = DIRECTION ( 'NONE',  ( -0.5364919789714478471, 0.6444004775717705469, -0.5449076811759709926 ) ) ;
#17965 = DIRECTION ( 'NONE',  ( 0.005961354470445682716, -0.6427876096865404731, -0.7660212471507180654 ) ) ;
#17966 = DIRECTION ( 'NONE',  ( 0.007781995580012663651, -3.146120232559066537E-19, -0.9999697198139514409 ) ) ;
#17967 = ORIENTED_EDGE ( 'NONE', *, *, #48078, .F. ) ;
#17968 = DIRECTION ( 'NONE',  ( 0.007781995580012663651, -3.146120232559066537E-19, -0.9999697198139514409 ) ) ;
#17969 = LINE ( 'NONE', #27601, #22269 ) ;
#17970 = CARTESIAN_POINT ( 'NONE',  ( -12.15116108492864377, 0.000000000000000000, 1.401855352044617975 ) ) ;
#17971 = EDGE_LOOP ( 'NONE', ( #26079, #31342, #31967, #55911 ) ) ;
#17972 = DIRECTION ( 'NONE',  ( 0.000000000000000000, -1.000000000000000000, 0.000000000000000000 ) ) ;
#17973 = DIRECTION ( 'NONE',  ( 0.5364919789714477361, 0.6444004775717706579, 0.5449076811759711036 ) ) ;
#17974 = VERTEX_POINT ( 'NONE', #31990 ) ;
#17975 = EDGE_CURVE ( 'NONE', #44387, #41818, #27752, .T. ) ;
#17976 = DIRECTION ( 'NONE',  ( -0.6427681459581293666, -0.7660444431189770143, -0.005002170337467561935 ) ) ;
#17977 = FACE_OUTER_BOUND ( 'NONE', #9798, .T. ) ;
#17978 = EDGE_CURVE ( 'NONE', #29379, #15700, #14665, .T. ) ;
#17979 = EDGE_CURVE ( 'NONE', #6764, #6080, #44768, .T. ) ;
#17980 = PLANE ( 'NONE',  #35996 ) ;
#17981 = CARTESIAN_POINT ( 'NONE',  ( 2.072287782118878319, 0.000000000000000000, -2.950529333540147015 ) ) ;
#17982 = ORIENTED_EDGE ( 'NONE', *, *, #13399, .T. ) ;
#17983 = ORIENTED_EDGE ( 'NONE', *, *, #31276, .T. ) ;
#17984 = CARTESIAN_POINT ( 'NONE',  ( -23.33849165029409889, 0.000000000000000000, 5.946783852668351855 ) ) ;
#17985 = LINE ( 'NONE', #25957, #21386 ) ;
#17986 = CARTESIAN_POINT ( 'NONE',  ( -27.99923088623136636, 0.000000000000000000, 7.757173251277078130 ) ) ;
#17987 = PLANE ( 'NONE',  #54689 ) ;
#17988 = FACE_OUTER_BOUND ( 'NONE', #53481, .T. ) ;
#17989 = DIRECTION ( 'NONE',  ( 0.9999697198139515519, 0.000000000000000000, 0.007781995580013368816 ) ) ;
#17990 = ORIENTED_EDGE ( 'NONE', *, *, #40746, .T. ) ;
#17991 = CARTESIAN_POINT ( 'NONE',  ( -12.80458192191714595, 0.000000000000000000, 11.86454056839041726 ) ) ;
#17992 = LINE ( 'NONE', #35314, #21525 ) ;
#17993 = VERTEX_POINT ( 'NONE', #11463 ) ;
#17994 = LINE ( 'NONE', #35317, #20206 ) ;
#17995 = PLANE ( 'NONE',  #36865 ) ;
#17996 = DIRECTION ( 'NONE',  ( -0.7660212471507179544, -0.6427876096865405842, -0.005961354470445141482 ) ) ;
#17997 = ORIENTED_EDGE ( 'NONE', *, *, #11645, .F. ) ;
#17998 = AXIS2_PLACEMENT_3D ( 'NONE', #22988, #18747, #14475 ) ;
#17999 = PLANE ( 'NONE',  #42076 ) ;
#18000 = EDGE_LOOP ( 'NONE', ( #31694, #35953, #51324, #25354 ) ) ;
#18001 = EDGE_CURVE ( 'NONE', #19601, #24549, #40537, .T. ) ;
#18002 = EDGE_LOOP ( 'NONE', ( #42098, #30789, #21038, #9809 ) ) ;
#18003 = ORIENTED_EDGE ( 'NONE', *, *, #34292, .T. ) ;
#18004 = EDGE_CURVE ( 'NONE', #28250, #7109, #6177, .T. ) ;
#18005 = VERTEX_POINT ( 'NONE', #7462 ) ;
#18006 = CARTESIAN_POINT ( 'NONE',  ( -67.08542992444135677, -8.381013491352103273, 2.158836163547856124 ) ) ;
#18007 = ORIENTED_EDGE ( 'NONE', *, *, #35287, .F. ) ;
#18008 = CARTESIAN_POINT ( 'NONE',  ( -21.41954753101251541, 3.686347215771511365, 4.884397627102543105 ) ) ;
#18009 = ORIENTED_EDGE ( 'NONE', *, *, #10796, .T. ) ;
#18010 = CARTESIAN_POINT ( 'NONE',  ( -19.60834386242827776, 0.000000000000000000, 4.298478389818581213 ) ) ;
#18011 = EDGE_CURVE ( 'NONE', #1435, #22163, #7763, .T. ) ;
#18012 = ORIENTED_EDGE ( 'NONE', *, *, #35250, .F. ) ;
#18013 = PLANE ( 'NONE',  #4775 ) ;
#18014 = EDGE_LOOP ( 'NONE', ( #6191, #7480, #18646, #23341 ) ) ;
#18015 = DIRECTION ( 'NONE',  ( 0.5364919789714477361, 0.6444004775717706579, 0.5449076811759711036 ) ) ;
#18016 = CARTESIAN_POINT ( 'NONE',  ( -14.20280369269832832, 0.000000000000000000, 12.40765738797303719 ) ) ;
#18017 = CARTESIAN_POINT ( 'NONE',  ( -15.79570695489036858, 0.000000000000000000, 3.958817142012544643 ) ) ;
#18018 = CARTESIAN_POINT ( 'NONE',  ( -19.42910703681909368, 21.15220053346460816, 4.255330291687501543 ) ) ;
#18019 = DIRECTION ( 'NONE',  ( -0.005002170337468016433, -0.7660444431189770143, 0.6427681459581293666 ) ) ;
#18020 = CARTESIAN_POINT ( 'NONE',  ( -24.26908309836554878, 0.000000000000000000, 6.108867788427308376 ) ) ;
#18021 = VERTEX_POINT ( 'NONE', #10424 ) ;
#18022 = ORIENTED_EDGE ( 'NONE', *, *, #30731, .T. ) ;
#18023 = FACE_OUTER_BOUND ( 'NONE', #39228, .T. ) ;
#18024 = CARTESIAN_POINT ( 'NONE',  ( 2.072287782118878319, 0.000000000000000000, -2.950529333540147015 ) ) ;
#18025 = EDGE_CURVE ( 'NONE', #16374, #37342, #42102, .T. ) ;
#18026 = FACE_OUTER_BOUND ( 'NONE', #18000, .T. ) ;
#18027 = DIRECTION ( 'NONE',  ( 0.9999697198139515519, 0.000000000000000000, 0.007781995580013368816 ) ) ;
#18028 = LINE ( 'NONE', #16924, #41267 ) ;
#18029 = DIRECTION ( 'NONE',  ( -0.005961354470445682716, -0.6427876096865404731, 0.7660212471507180654 ) ) ;
#18030 = VERTEX_POINT ( 'NONE', #37568 ) ;
#18031 = LINE ( 'NONE', #15185, #33837 ) ;
#18032 = EDGE_CURVE ( 'NONE', #6272, #32386, #24495, .T. ) ;
#18033 = LINE ( 'NONE', #30558, #55800 ) ;
#18034 = ORIENTED_EDGE ( 'NONE', *, *, #50894, .T. ) ;
#18035 = CARTESIAN_POINT ( 'NONE',  ( -17.23428484710887076, 0.000000000000000000, 9.687608899537771379 ) ) ;
#18036 = CARTESIAN_POINT ( 'NONE',  ( -16.99361711142231002, -3.594132820645660420, 9.181413994056926597 ) ) ;
#18037 = EDGE_CURVE ( 'NONE', #14582, #19374, #54584, .T. ) ;
#18038 = FACE_OUTER_BOUND ( 'NONE', #43628, .T. ) ;
#18039 = EDGE_CURVE ( 'NONE', #32268, #40689, #28788, .T. ) ;
#18040 = DIRECTION ( 'NONE',  ( -0.000000000000000000, -1.000000000000000000, -0.000000000000000000 ) ) ;
#18041 = FACE_OUTER_BOUND ( 'NONE', #1610, .T. ) ;
#18042 = ORIENTED_EDGE ( 'NONE', *, *, #23519, .T. ) ;
#18043 = ORIENTED_EDGE ( 'NONE', *, *, #33107, .T. ) ;
#18044 = DIRECTION ( 'NONE',  ( 0.5364919789714477361, 0.6444004775717706579, 0.5449076811759711036 ) ) ;
#18045 = DIRECTION ( 'NONE',  ( -0.1139275668495183386, 0.9934890585767658377, 4.694855797473113547E-16 ) ) ;
#18046 = CARTESIAN_POINT ( 'NONE',  ( -8.926160398992163181, -0.1191753592594191058, 4.013552926324940096 ) ) ;
#18047 = EDGE_CURVE ( 'NONE', #27104, #32512, #29995, .T. ) ;
#18048 = PRODUCT_DEFINITION ( 'UNKNOWN', '', #13574, #6432 ) ;
#18049 = CARTESIAN_POINT ( 'NONE',  ( -16.49063472986307843, 0.000000000000000000, 7.846735807668965279 ) ) ;
#18050 = CARTESIAN_POINT ( 'NONE',  ( -19.65599895527812890, 3.200641362704007786, 9.769176383365808292 ) ) ;
#18051 = CARTESIAN_POINT ( 'NONE',  ( -19.33759994122731385, 21.49370731433205250, -4.239680377485293583 ) ) ;
#18052 = DIRECTION ( 'NONE',  ( 0.9999697198139515519, 0.000000000000000000, 0.007781995580013368816 ) ) ;
#18053 = EDGE_CURVE ( 'NONE', #51694, #55479, #46945, .T. ) ;
#18054 = DIRECTION ( 'NONE',  ( -0.005002170337468016433, -0.7660444431189770143, 0.6427681459581293666 ) ) ;
#18055 = DIRECTION ( 'NONE',  ( -0.9999697198139514409, -0.000000000000000000, -0.007781995580013368816 ) ) ;
#18056 = VERTEX_POINT ( 'NONE', #3758 ) ;
#18057 = DIRECTION ( 'NONE',  ( -0.7660212471507179544, -0.6427876096865405842, -0.005961354470445141482 ) ) ;
#18058 = ORIENTED_EDGE ( 'NONE', *, *, #39584, .F. ) ;
#18059 = CARTESIAN_POINT ( 'NONE',  ( -17.99516527612767192, -2.622721114510662144, 3.787575893809204342 ) ) ;
#18060 = DIRECTION ( 'NONE',  ( 0.5449076811759707706, 0.6444004775717708799, -0.5364919789714476250 ) ) ;
#18061 = ORIENTED_EDGE ( 'NONE', *, *, #38030, .T. ) ;
#18062 = CARTESIAN_POINT ( 'NONE',  ( -14.40179626436711224, 0.000000000000000000, 3.969664877316573914 ) ) ;
#18063 = ORIENTED_EDGE ( 'NONE', *, *, #22890, .F. ) ;
#18064 = ORIENTED_EDGE ( 'NONE', *, *, #44136, .T. ) ;
#18065 = ORIENTED_EDGE ( 'NONE', *, *, #30357, .T. ) ;
#18066 = DIRECTION ( 'NONE',  ( -0.9999697198139514409, -0.000000000000000000, -0.007781995580013368816 ) ) ;
#18067 = ORIENTED_EDGE ( 'NONE', *, *, #3784, .T. ) ;
#18068 = VERTEX_POINT ( 'NONE', #42949 ) ;
#18069 = LINE ( 'NONE', #25460, #50141 ) ;
#18070 = PLANE ( 'NONE',  #51228 ) ;
#18071 = ORIENTED_EDGE ( 'NONE', *, *, #33660, .F. ) ;
#18072 = ORIENTED_EDGE ( 'NONE', *, *, #14279, .F. ) ;
#18073 = DIRECTION ( 'NONE',  ( -0.005002170337468016433, -0.7660444431189770143, 0.6427681459581293666 ) ) ;
#18074 = EDGE_CURVE ( 'NONE', #29764, #48603, #17377, .T. ) ;
#18075 = ORIENTED_EDGE ( 'NONE', *, *, #32208, .F. ) ;
#18076 = ORIENTED_EDGE ( 'NONE', *, *, #22942, .T. ) ;
#18077 = CARTESIAN_POINT ( 'NONE',  ( -13.07066190154808361, 0.000000000000000000, 12.04713590736729678 ) ) ;
#18078 = FACE_OUTER_BOUND ( 'NONE', #38229, .T. ) ;
#18079 = LINE ( 'NONE', #18654, #49499 ) ;
#18080 = ORIENTED_EDGE ( 'NONE', *, *, #44809, .T. ) ;
#18081 = DIRECTION ( 'NONE',  ( 0.000000000000000000, -1.000000000000000000, 0.000000000000000000 ) ) ;
#18082 = ORIENTED_EDGE ( 'NONE', *, *, #24523, .T. ) ;
#18083 = EDGE_CURVE ( 'NONE', #30276, #32205, #12850, .T. ) ;
#18084 = LINE ( 'NONE', #47634, #42042 ) ;
#18085 = EDGE_CURVE ( 'NONE', #36877, #31801, #3496, .T. ) ;
#18086 = EDGE_CURVE ( 'NONE', #24619, #32474, #52327, .T. ) ;
#18087 = CARTESIAN_POINT ( 'NONE',  ( 2.072287782118878319, 0.000000000000000000, -2.950529333540147015 ) ) ;
#18088 = CARTESIAN_POINT ( 'NONE',  ( -13.08330893211609869, 0.000000000000000000, 1.763933231766363630 ) ) ;
#18089 = DIRECTION ( 'NONE',  ( 0.5449076811759707706, 0.6444004775717708799, -0.5364919789714476250 ) ) ;
#18090 = DIRECTION ( 'NONE',  ( 0.000000000000000000, -0.000000000000000000, -1.000000000000000000 ) ) ;
#18091 = CARTESIAN_POINT ( 'NONE',  ( -23.23471500290295921, 19.24370688441070953, 4.657440554554202805 ) ) ;
#18092 = CARTESIAN_POINT ( 'NONE',  ( -12.75629523410269250, 0.000000000000000000, 5.659804882266454840 ) ) ;
#18093 = EDGE_LOOP ( 'NONE', ( #41722, #22806, #6474, #12934 ) ) ;
#18094 = DIRECTION ( 'NONE',  ( -0.5364919789714478471, 0.6444004775717705469, -0.5449076811759709926 ) ) ;
#18095 = DIRECTION ( 'NONE',  ( -0.5364919789714478471, 0.6444004775717705469, -0.5449076811759709926 ) ) ;
#18096 = LINE ( 'NONE', #4487, #55937 ) ;
#18097 = EDGE_CURVE ( 'NONE', #34435, #21097, #47199, .T. ) ;
#18098 = LINE ( 'NONE', #13003, #52586 ) ;
#18099 = CARTESIAN_POINT ( 'NONE',  ( -15.60496230262594608, 21.91669585219702654, -3.983230142812006047 ) ) ;
#18100 = CARTESIAN_POINT ( 'NONE',  ( -16.81190032086591302, 0.000000000000000000, 3.212244750653343583 ) ) ;
#18101 = EDGE_CURVE ( 'NONE', #8803, #15538, #4054, .T. ) ;
#18102 = DIRECTION ( 'NONE',  ( 0.007781995580012662783, 0.000000000000000000, -0.9999697198139514409 ) ) ;
#18103 = CARTESIAN_POINT ( 'NONE',  ( -68.93342745996714882, -0.9999999999999983347, -5.847034362371242189 ) ) ;
#18104 = ORIENTED_EDGE ( 'NONE', *, *, #45168, .T. ) ;
#18105 = CARTESIAN_POINT ( 'NONE',  ( -14.94916102560700821, 0.000000000000000000, 2.688082935172642962 ) ) ;
#18106 = CARTESIAN_POINT ( 'NONE',  ( -19.05103928628325605, 0.000000000000000000, 4.302815462894245435 ) ) ;
#18107 = CARTESIAN_POINT ( 'NONE',  ( -13.73672976910459909, 0.000000000000000000, 12.22661844811216270 ) ) ;
#18108 = EDGE_CURVE ( 'NONE', #21115, #54376, #43259, .T. ) ;
#18109 = LINE ( 'NONE', #17324, #32014 ) ;
#18110 = LINE ( 'NONE', #43125, #49955 ) ;
#18111 = CARTESIAN_POINT ( 'NONE',  ( -19.96464863903120346, -4.889348428825662118, 12.46113300763930098 ) ) ;
#18112 = LINE ( 'NONE', #41309, #22311 ) ;
#18113 = CARTESIAN_POINT ( 'NONE',  ( -14.94916102560700821, 0.000000000000000000, 2.688082935172642962 ) ) ;
#18114 = EDGE_CURVE ( 'NONE', #24756, #16295, #25932, .T. ) ;
#18115 = DIRECTION ( 'NONE',  ( 0.000000000000000000, 1.000000000000000000, 0.000000000000000000 ) ) ;
#18116 = LINE ( 'NONE', #22406, #38296 ) ;
#18117 = ORIENTED_EDGE ( 'NONE', *, *, #9572, .F. ) ;
#18118 = ORIENTED_EDGE ( 'NONE', *, *, #19703, .T. ) ;
#18119 = VERTEX_POINT ( 'NONE', #8305 ) ;
#18120 = ORIENTED_EDGE ( 'NONE', *, *, #27082, .F. ) ;
#18121 = ORIENTED_EDGE ( 'NONE', *, *, #15753, .T. ) ;
#18122 = CARTESIAN_POINT ( 'NONE',  ( 2.072287782118878319, 0.000000000000000000, -2.950529333540147015 ) ) ;
#18123 = CARTESIAN_POINT ( 'NONE',  ( -13.66288791392935664, 1.095915999411505082, 3.987035636642269232 ) ) ;
#18124 = ORIENTED_EDGE ( 'NONE', *, *, #37193, .T. ) ;
#18125 = ORIENTED_EDGE ( 'NONE', *, *, #55945, .F. ) ;
#18126 = ADVANCED_FACE ( 'NONE', ( #21382 ), #56028, .F. ) ;
#18127 = VECTOR ( 'NONE', #31693, 1000.000000000000227 ) ;
#18128 = PLANE ( 'NONE',  #15783 ) ;
#18129 = ORIENTED_EDGE ( 'NONE', *, *, #18404, .T. ) ;
#18130 = CARTESIAN_POINT ( 'NONE',  ( -10.27421835998572064, 0.000000000000000000, 10.96090226820206048 ) ) ;
#18131 = LINE ( 'NONE', #26657, #54970 ) ;
#18132 = ORIENTED_EDGE ( 'NONE', *, *, #26813, .F. ) ;
#18133 = DIRECTION ( 'NONE',  ( 0.6427681459581294776, -0.7660444431189769032, 0.005002170337467562802 ) ) ;
#18134 = EDGE_CURVE ( 'NONE', #9163, #13086, #26202, .T. ) ;
#18135 = EDGE_CURVE ( 'NONE', #48012, #19489, #336, .T. ) ;
#18136 = ADVANCED_FACE ( 'NONE', ( #29900 ), #39245, .F. ) ;
#18137 = VERTEX_POINT ( 'NONE', #8046 ) ;
#18138 = DIRECTION ( 'NONE',  ( 0.9999697198139515519, 0.000000000000000000, 0.007781995580013368816 ) ) ;
#18139 = LINE ( 'NONE', #35462, #6628 ) ;
#18140 = EDGE_CURVE ( 'NONE', #50938, #9324, #4605, .T. ) ;
#18141 = LINE ( 'NONE', #22686, #9173 ) ;
#18142 = LINE ( 'NONE', #53898, #18785 ) ;
#18143 = EDGE_LOOP ( 'NONE', ( #22445, #44035, #54547, #26575, #25537 ) ) ;
#18144 = LINE ( 'NONE', #31210, #49401 ) ;
#18145 = DIRECTION ( 'NONE',  ( 0.005961354470445682716, -0.6427876096865404731, -0.7660212471507180654 ) ) ;
#18146 = DIRECTION ( 'NONE',  ( 0.005961354470445682716, -0.6427876096865404731, -0.7660212471507180654 ) ) ;
#18147 = EDGE_LOOP ( 'NONE', ( #15231, #33732, #38, #42439 ) ) ;
#18148 = DIRECTION ( 'NONE',  ( 0.007781995580012663651, -3.146120232559066537E-19, -0.9999697198139514409 ) ) ;
#18149 = ORIENTED_EDGE ( 'NONE', *, *, #29832, .F. ) ;
#18150 = DIRECTION ( 'NONE',  ( -0.005961354470445682716, -0.6427876096865404731, 0.7660212471507180654 ) ) ;
#18151 = CARTESIAN_POINT ( 'NONE',  ( -14.94760462649100496, 0.000000000000000000, 2.488088991209854051 ) ) ;
#18152 = DIRECTION ( 'NONE',  ( -0.5449076811759708816, 0.6444004775717707689, 0.5364919789714475140 ) ) ;
#18153 = ADVANCED_FACE ( 'NONE', ( #12583 ), #17676, .F. ) ;
#18154 = DIRECTION ( 'NONE',  ( 0.9999697198139515519, 0.000000000000000000, 0.007781995580013368816 ) ) ;
#18155 = DIRECTION ( 'NONE',  ( 0.005961354470445682716, -0.6427876096865404731, -0.7660212471507180654 ) ) ;
#18156 = CARTESIAN_POINT ( 'NONE',  ( -18.67619601524082285, 0.000000000000000000, 3.936400510096834893 ) ) ;
#18157 = CARTESIAN_POINT ( 'NONE',  ( -32.10901097986136676, 0.000000000000000000, 16.76339505873265168 ) ) ;
#18158 = EDGE_CURVE ( 'NONE', #29543, #30294, #13430, .T. ) ;
#18159 = CARTESIAN_POINT ( 'NONE',  ( -15.40103151951671734, 0.000000000000000000, 12.95233060667165681 ) ) ;
#18160 = EDGE_CURVE ( 'NONE', #29959, #38766, #42405, .T. ) ;
#18161 = FACE_OUTER_BOUND ( 'NONE', #44376, .T. ) ;
#18162 = VERTEX_POINT ( 'NONE', #38124 ) ;
#18163 = CARTESIAN_POINT ( 'NONE',  ( -8.509919637592204822, -0.1191753592594197858, 10.23596830920056711 ) ) ;
#18164 = CARTESIAN_POINT ( 'NONE',  ( -15.03495456790438389, -0.1191753592594197858, 12.77051346725278158 ) ) ;
#18165 = CARTESIAN_POINT ( 'NONE',  ( -20.54049170961573267, 0.000000000000000000, 4.660556269540326646 ) ) ;
#18166 = CARTESIAN_POINT ( 'NONE',  ( -9.405935838180976560, -0.1191753592594177180, 5.955207195476888593 ) ) ;
#18167 = EDGE_CURVE ( 'NONE', #17707, #27553, #25357, .T. ) ;
#18168 = CARTESIAN_POINT ( 'NONE',  ( 2.602374448188125350E-16, 0.000000000000000000, 2.125000000000000000 ) ) ;
#18169 = CARTESIAN_POINT ( 'NONE',  ( 4.912750499197526821, -1.131233082521083455, -2.061810099490656079 ) ) ;
#18170 = PLANE ( 'NONE',  #32889 ) ;
#18171 = ORIENTED_EDGE ( 'NONE', *, *, #52909, .F. ) ;
#18172 = AXIS2_PLACEMENT_3D ( 'NONE', #11678, #42607, #12233 ) ;
#18173 = ORIENTED_EDGE ( 'NONE', *, *, #41247, .T. ) ;
#18174 = DIRECTION ( 'NONE',  ( -0.02142857142857158143, 0.000000000000000000, 0.9997703818010067467 ) ) ;
#18175 = DIRECTION ( 'NONE',  ( 0.5364919789714477361, 0.6444004775717706579, 0.5449076811759711036 ) ) ;
#18176 = ORIENTED_EDGE ( 'NONE', *, *, #23411, .F. ) ;
#18177 = PLANE ( 'NONE',  #12289 ) ;
#18178 = ORIENTED_EDGE ( 'NONE', *, *, #7626, .T. ) ;
#18179 = DIRECTION ( 'NONE',  ( -0.9999697198139514409, -0.000000000000000000, -0.007781995580013368816 ) ) ;
#18180 = ORIENTED_EDGE ( 'NONE', *, *, #27748, .T. ) ;
#18181 = VERTEX_POINT ( 'NONE', #19058 ) ;
#18182 = ORIENTED_EDGE ( 'NONE', *, *, #14467, .T. ) ;
#18183 = LINE ( 'NONE', #30963, #53784 ) ;
#18184 = CARTESIAN_POINT ( 'NONE',  ( 5.454592090961233097, -6.230699628392518008, 2.061810099490656079 ) ) ;
#18185 = CARTESIAN_POINT ( 'NONE',  ( -18.58296605579292660, -5.536956232915664522, 3.922918320456664887 ) ) ;
#18186 = EDGE_CURVE ( 'NONE', #2789, #38090, #31589, .T. ) ;
#18187 = DIRECTION ( 'NONE',  ( 0.007781995580012663651, 0.000000000000000000, -0.9999697198139515519 ) ) ;
#18188 = ORIENTED_EDGE ( 'NONE', *, *, #34591, .T. ) ;
#18190 = ORIENTED_EDGE ( 'NONE', *, *, #41391, .T. ) ;
#18189 = EDGE_CURVE ( 'NONE', #50687, #41455, #39816, .T. ) ;
#18191 = DIRECTION ( 'NONE',  ( 0.5364919789714477361, 0.6444004775717706579, 0.5449076811759711036 ) ) ;
#18192 = ORIENTED_EDGE ( 'NONE', *, *, #37397, .T. ) ;
#18193 = LINE ( 'NONE', #44592, #34799 ) ;
#18194 = EDGE_LOOP ( 'NONE', ( #27882, #22667, #33574, #50954 ) ) ;
#18195 = CARTESIAN_POINT ( 'NONE',  ( -18.21966661063519766, -0.1191753592594176486, 4.039956355595887061 ) ) ;
#18196 = DIRECTION ( 'NONE',  ( 0.000000000000000000, -1.000000000000000000, 0.000000000000000000 ) ) ;
#18197 = EDGE_CURVE ( 'NONE', #19901, #51242, #48312, .T. ) ;
#18198 = EDGE_CURVE ( 'NONE', #530, #21098, #26752, .T. ) ;
#18199 = ADVANCED_FACE ( 'NONE', ( #9143 ), #23056, .T. ) ;
#18200 = ORIENTED_EDGE ( 'NONE', *, *, #38717, .T. ) ;
#18201 = AXIS2_PLACEMENT_3D ( 'NONE', #46932, #629, #43249 ) ;
#18202 = LINE ( 'NONE', #19046, #9571 ) ;
#18203 = ORIENTED_EDGE ( 'NONE', *, *, #3852, .T. ) ;
#18204 = EDGE_CURVE ( 'NONE', #33042, #6987, #54958, .T. ) ;
#18205 = VECTOR ( 'NONE', #7934, 999.9999999999998863 ) ;
#18206 = DIRECTION ( 'NONE',  ( 0.005961354470445682716, -0.6427876096865404731, -0.7660212471507180654 ) ) ;
#18207 = ORIENTED_EDGE ( 'NONE', *, *, #21517, .F. ) ;
#18208 = DIRECTION ( 'NONE',  ( 0.007781995580012662783, 0.000000000000000000, -0.9999697198139514409 ) ) ;
#18209 = CARTESIAN_POINT ( 'NONE',  ( -13.81839363928948750, -4.241740624735661491, 9.010884102239385740 ) ) ;
#18210 = LINE ( 'NONE', #39546, #28284 ) ;
#18211 = ORIENTED_EDGE ( 'NONE', *, *, #10609, .T. ) ;
#18212 = CARTESIAN_POINT ( 'NONE',  ( -14.52843791745405255, -0.1191753592594190225, 7.392670979059843717 ) ) ;
#18213 = CARTESIAN_POINT ( 'NONE',  ( -11.40636015113596180, 0.000000000000000000, 11.32142374880780089 ) ) ;
#18214 = DIRECTION ( 'NONE',  ( 0.5449076811759707706, 0.6444004775717708799, -0.5364919789714476250 ) ) ;
#18215 = CARTESIAN_POINT ( 'NONE',  ( -6.110905869600904872, 1.712176620043476140E-14, -3.600000000000000089 ) ) ;
#18216 = DIRECTION ( 'NONE',  ( -0.6427681459581293666, -0.7660444431189770143, -0.005002170337467561935 ) ) ;
#18218 = EDGE_CURVE ( 'NONE', #2911, #42260, #44918, .T. ) ;
#18217 = DIRECTION ( 'NONE',  ( 0.8660254037844380415, 0.5000000000000011102, 0.000000000000000000 ) ) ;
#18219 = ORIENTED_EDGE ( 'NONE', *, *, #30615, .T. ) ;
#18220 = CARTESIAN_POINT ( 'NONE',  ( -15.13495153988577968, 0.000000000000000000, 12.76973526769478084 ) ) ;
#18221 = DIRECTION ( 'NONE',  ( -0.005961354470445682716, -0.6427876096865404731, 0.7660212471507180654 ) ) ;
#18222 = ADVANCED_FACE ( 'NONE', ( #53433 ), #44350, .F. ) ;
#18223 = DIRECTION ( 'NONE',  ( 0.9999697198139515519, 0.000000000000000000, 0.007781995580013368816 ) ) ;
#18224 = VERTEX_POINT ( 'NONE', #4893 ) ;
#18225 = FACE_OUTER_BOUND ( 'NONE', #46431, .T. ) ;
#18226 = DIRECTION ( 'NONE',  ( 0.007781995580012663651, -3.146120232559066537E-19, -0.9999697198139514409 ) ) ;
#18227 = EDGE_LOOP ( 'NONE', ( #24599, #16320, #35984, #21441 ) ) ;
#18228 = DIRECTION ( 'NONE',  ( 0.007781995580012663651, 0.000000000000000000, -0.9999697198139515519 ) ) ;
#18229 = AXIS2_PLACEMENT_3D ( 'NONE', #13841, #51631, #515 ) ;
#18230 = EDGE_CURVE ( 'NONE', #32968, #7355, #52582, .T. ) ;
#18231 = VECTOR ( 'NONE', #32411, 1000.000000000000114 ) ;
#18232 = CARTESIAN_POINT ( 'NONE',  ( -25.85160216376510434, 17.67350346510513148, -4.606045122360801436 ) ) ;
#18233 = DIRECTION ( 'NONE',  ( 0.9999697198139515519, 0.000000000000000000, 0.007781995580013368816 ) ) ;
#18234 = ADVANCED_FACE ( 'NONE', ( #1172 ), #48895, .F. ) ;
#18235 = CARTESIAN_POINT ( 'NONE',  ( -20.32198454194807979, -1.489407457353157049, 7.020052044550838310 ) ) ;
#18236 = ORIENTED_EDGE ( 'NONE', *, *, #50895, .F. ) ;
#18237 = ORIENTED_EDGE ( 'NONE', *, *, #44046, .T. ) ;
#18238 = DIRECTION ( 'NONE',  ( -0.5449076811759708816, 0.6444004775717707689, 0.5364919789714475140 ) ) ;
#18239 = DIRECTION ( 'NONE',  ( -0.005002170337468016433, -0.7660444431189770143, 0.6427681459581293666 ) ) ;
#18240 = DIRECTION ( 'NONE',  ( 0.9999697198139515519, 0.000000000000000000, 0.007781995580013368816 ) ) ;
#18241 = CARTESIAN_POINT ( 'NONE',  ( -14.36410299895545961, 0.2864062442990018553, 2.252299284581917860 ) ) ;
#18242 = DIRECTION ( 'NONE',  ( -0.000000000000000000, -0.000000000000000000, -1.000000000000000000 ) ) ;
#18243 = VECTOR ( 'NONE', #40000, 1000.000000000000227 ) ;
#18244 = DIRECTION ( 'NONE',  ( -0.6427681459581293666, -0.7660444431189770143, -0.005002170337467561935 ) ) ;
#18245 = ORIENTED_EDGE ( 'NONE', *, *, #33434, .T. ) ;
#18246 = DIRECTION ( 'NONE',  ( -0.6427681459581293666, -0.7660444431189770143, -0.005002170337467561935 ) ) ;
#18247 = VECTOR ( 'NONE', #32659, 1000.000000000000000 ) ;
#18248 = LINE ( 'NONE', #1510, #48723 ) ;
#18249 = ORIENTED_EDGE ( 'NONE', *, *, #21749, .T. ) ;
#18250 = FACE_OUTER_BOUND ( 'NONE', #2860, .T. ) ;
#18251 = CARTESIAN_POINT ( 'NONE',  ( -16.25615214383689278, 0.000000000000000000, 3.416575767691794496 ) ) ;
#18252 = CARTESIAN_POINT ( 'NONE',  ( -17.90023334230202323, 0.000000000000000000, 9.851752347948734112 ) ) ;
#18253 = VERTEX_POINT ( 'NONE', #5449 ) ;
#18254 = CARTESIAN_POINT ( 'NONE',  ( -10.37421533196711465, -0.1191753592594197858, 10.96012406864405975 ) ) ;
#18255 = ORIENTED_EDGE ( 'NONE', *, *, #26796, .T. ) ;
#18256 = ORIENTED_EDGE ( 'NONE', *, *, #46167, .T. ) ;
#18257 = ORIENTED_EDGE ( 'NONE', *, *, #33730, .T. ) ;
#18258 = ORIENTED_EDGE ( 'NONE', *, *, #42068, .F. ) ;
#18259 = LINE ( 'NONE', #23643, #54719 ) ;
#18260 = PRODUCT_DEFINITION_SHAPE ( 'NONE', 'NONE',  #35061 ) ;
#18261 = VERTEX_POINT ( 'NONE', #13966 ) ;
#18262 = CARTESIAN_POINT ( 'NONE',  ( -17.55224900710100044, -2.653845599528779520, 12.45560879478165184 ) ) ;
#18263 = CARTESIAN_POINT ( 'NONE',  ( -26.13493519185646008, 0.000000000000000000, 7.033017491833586377 ) ) ;
#18264 = EDGE_CURVE ( 'NONE', #48789, #29854, #42161, .T. ) ;
#18265 = VECTOR ( 'NONE', #33969, 1000.000000000000227 ) ;
#18266 = VECTOR ( 'NONE', #41728, 1000.000000000000227 ) ;
#18267 = ORIENTED_EDGE ( 'NONE', *, *, #11682, .F. ) ;
#18268 = CARTESIAN_POINT ( 'NONE',  ( -15.52974634762279038, 0.000000000000000000, 3.791560895369574080 ) ) ;
#18269 = ORIENTED_EDGE ( 'NONE', *, *, #13393, .T. ) ;
#18270 = DIRECTION ( 'NONE',  ( 0.005002170337468016433, -0.7660444431189770143, -0.6427681459581293666 ) ) ;
#18271 = ORIENTED_EDGE ( 'NONE', *, *, #20451, .F. ) ;
#18272 = ADVANCED_FACE ( 'NONE', ( #9990 ), #22217, .F. ) ;
#18273 = ADVANCED_FACE ( 'NONE', ( #5729 ), #642, .F. ) ;
#18274 = DIRECTION ( 'NONE',  ( 0.000000000000000000, -1.000000000000000000, 0.000000000000000000 ) ) ;
#18275 = CARTESIAN_POINT ( 'NONE',  ( -17.22410628747702077, 0.000000000000000000, 8.379685845801690292 ) ) ;
#18276 = VECTOR ( 'NONE', #19701, 1000.000000000000227 ) ;
#18277 = CARTESIAN_POINT ( 'NONE',  ( -15.18146849030217993, 1.257817950434004350, 2.538798679945565961 ) ) ;
#18278 = FILL_AREA_STYLE ('',( #951 ) ) ;
#18279 = PLANE ( 'NONE',  #8782 ) ;
#18280 = LINE ( 'NONE', #35084, #51922 ) ;
#18281 = ORIENTED_EDGE ( 'NONE', *, *, #46594, .F. ) ;
#18282 = VERTEX_POINT ( 'NONE', #36381 ) ;
#18283 = CARTESIAN_POINT ( 'NONE',  ( -33.59133976979808978, -0.1191753592594197858, 9.829643557626155825 ) ) ;
#18284 = DIRECTION ( 'NONE',  ( 0.007781995580012663651, -3.146120232559066537E-19, -0.9999697198139514409 ) ) ;
#18285 = DIRECTION ( 'NONE',  ( -0.5449076811759708816, 0.6444004775717707689, 0.5364919789714475140 ) ) ;
#18286 = DIRECTION ( 'NONE',  ( -0.5449076811759708816, 0.6444004775717707689, 0.5364919789714475140 ) ) ;
#18287 = ORIENTED_EDGE ( 'NONE', *, *, #38708, .T. ) ;
#18288 = DIRECTION ( 'NONE',  ( 0.7660212471507180654, -0.6427876096865404731, 0.005961354470445141482 ) ) ;
#18289 = LINE ( 'NONE', #44162, #9642 ) ;
#18290 = ORIENTED_EDGE ( 'NONE', *, *, #52139, .F. ) ;
#18291 = PLANE ( 'NONE',  #46508 ) ;
#18292 = CARTESIAN_POINT ( 'NONE',  ( -20.95581447963228783, 20.46320434849166858, 4.352198852484694847 ) ) ;
#18293 = ORIENTED_EDGE ( 'NONE', *, *, #55348, .T. ) ;
#18294 = CARTESIAN_POINT ( 'NONE',  ( -17.19249169891891427, 0.000000000000000000, 4.317279109966281503 ) ) ;
#18295 = CARTESIAN_POINT ( 'NONE',  ( -27.06708303904391144, 0.000000000000000000, 7.395095371555332697 ) ) ;
#18296 = CARTESIAN_POINT ( 'NONE',  ( -19.65553346665874557, 5.467268677019013978, 4.142373939576459385 ) ) ;
#18297 = ADVANCED_FACE ( 'NONE', ( #10269 ), #53694, .F. ) ;
#18298 = FACE_OUTER_BOUND ( 'NONE', #42299, .T. ) ;
#18299 = DIRECTION ( 'NONE',  ( -0.6427681459581293666, -0.7660444431189770143, -0.005002170337467561935 ) ) ;
#18300 = ORIENTED_EDGE ( 'NONE', *, *, #34688, .T. ) ;
#18301 = ADVANCED_FACE ( 'NONE', ( #37802 ), #49733, .F. ) ;
#18302 = EDGE_LOOP ( 'NONE', ( #34442, #8673, #20649, #33296 ) ) ;
#18303 = DIRECTION ( 'NONE',  ( 0.5364919789714477361, 0.6444004775717706579, 0.5449076811759711036 ) ) ;
#18304 = DIRECTION ( 'NONE',  ( -0.9999697198139514409, -0.000000000000000000, -0.007781995580013368816 ) ) ;
#18305 = LINE ( 'NONE', #44177, #50539 ) ;
#18306 = EDGE_CURVE ( 'NONE', #14283, #25334, #23874, .T. ) ;
#18307 = AXIS2_PLACEMENT_3D ( 'NONE', #15725, #20571, #54091 ) ;
#18308 = AXIS2_PLACEMENT_3D ( 'NONE', #44678, #44988, #4742 ) ;
#18309 = PLANE ( 'NONE',  #32781 ) ;
#18310 = ADVANCED_FACE ( 'NONE', ( #24433 ), #10578, .F. ) ;
#18311 = CARTESIAN_POINT ( 'NONE',  ( -46.27156441860520175, 5.366025403784440151, 5.000000000000000000 ) ) ;
#18312 = ORIENTED_EDGE ( 'NONE', *, *, #43315, .F. ) ;
#18313 = CARTESIAN_POINT ( 'NONE',  ( -12.13851405436063047, 0.000000000000000000, 11.68505802764555135 ) ) ;
#18314 = CARTESIAN_POINT ( 'NONE',  ( -27.06552663992790997, 0.000000000000000000, 7.195101427592543786 ) ) ;
#18315 = DIRECTION ( 'NONE',  ( 0.005961354470445682716, -0.6427876096865404731, -0.7660212471507180654 ) ) ;
#18316 = DIRECTION ( 'NONE',  ( 0.007781995580012663651, 0.000000000000000000, -0.9999697198139515519 ) ) ;
#18317 = VECTOR ( 'NONE', #26978, 999.9999999999998863 ) ;
#18318 = VERTEX_POINT ( 'NONE', #49980 ) ;
#18319 = LINE ( 'NONE', #44726, #18394 ) ;
#18320 = ORIENTED_EDGE ( 'NONE', *, *, #48519, .F. ) ;
#18321 = CARTESIAN_POINT ( 'NONE',  ( -29.86352658060627618, 0.000000000000000000, 8.481329010720569883 ) ) ;
#18322 = LINE ( 'NONE', #52976, #297 ) ;
#18323 = ORIENTED_EDGE ( 'NONE', *, *, #34088, .T. ) ;
#18324 = DIRECTION ( 'NONE',  ( -0.5449076811759708816, 0.6444004775717707689, 0.5364919789714475140 ) ) ;
#18325 = AXIS2_PLACEMENT_3D ( 'NONE', #26315, #1023, #30609 ) ;
#18326 = EDGE_LOOP ( 'NONE', ( #42585, #6927, #22268, #52642, #53801, #50329, #30146 ) ) ;
#18327 = AXIS2_PLACEMENT_3D ( 'NONE', #53234, #18274, #48686 ) ;
#18328 = VERTEX_POINT ( 'NONE', #41742 ) ;
#18329 = ORIENTED_EDGE ( 'NONE', *, *, #7074, .T. ) ;
#18330 = PLANE ( 'NONE',  #32992 ) ;
#18331 = VERTEX_POINT ( 'NONE', #15927 ) ;
#18332 = ORIENTED_EDGE ( 'NONE', *, *, #32131, .T. ) ;
#18333 = DIRECTION ( 'NONE',  ( -0.5449076811759708816, 0.6444004775717707689, 0.5364919789714475140 ) ) ;
#18334 = EDGE_CURVE ( 'NONE', #25263, #1167, #15620, .T. ) ;
#18335 = DIRECTION ( 'NONE',  ( 0.5364919789714477361, 0.6444004775717706579, 0.5449076811759711036 ) ) ;
#18336 = ORIENTED_EDGE ( 'NONE', *, *, #50414, .F. ) ;
#18337 = EDGE_CURVE ( 'NONE', #46010, #54122, #53989, .T. ) ;
#18338 = ORIENTED_EDGE ( 'NONE', *, *, #21566, .T. ) ;
#18339 = DIRECTION ( 'NONE',  ( 0.9999697198139515519, 0.000000000000000000, 0.007781995580013368816 ) ) ;
#18340 = VERTEX_POINT ( 'NONE', #27890 ) ;
#18341 = VECTOR ( 'NONE', #33469, 1000.000000000000227 ) ;
#18342 = ORIENTED_EDGE ( 'NONE', *, *, #29565, .T. ) ;
#18343 = EDGE_CURVE ( 'NONE', #42498, #55547, #50274, .T. ) ;
#18344 = EDGE_CURVE ( 'NONE', #15522, #6267, #46280, .T. ) ;
#18345 = PLANE ( 'NONE',  #23055 ) ;
#18346 = CARTESIAN_POINT ( 'NONE',  ( -9.881852802408157999, -0.1159828484229821904, 7.056820793252878588 ) ) ;
#18347 = CARTESIAN_POINT ( 'NONE',  ( -8.926928673813481652, -0.1191753592594179401, 4.112274590956074505 ) ) ;
#18348 = CARTESIAN_POINT ( 'NONE',  ( -24.26908309836554878, 0.000000000000000000, 6.108867788427308376 ) ) ;
#18349 = AXIS2_PLACEMENT_3D ( 'NONE', #9177, #48656, #26226 ) ;
#18350 = EDGE_LOOP ( 'NONE', ( #14463, #50168, #27514, #6834 ) ) ;
#18351 = LINE ( 'NONE', #43629, #34616 ) ;
#18352 = ORIENTED_EDGE ( 'NONE', *, *, #43492, .F. ) ;
#18353 = VECTOR ( 'NONE', #46513, 999.9999999999998863 ) ;
#18354 = VECTOR ( 'NONE', #46274, 1000.000000000000227 ) ;
#18355 = DIRECTION ( 'NONE',  ( -0.005002170337468016433, -0.7660444431189770143, 0.6427681459581293666 ) ) ;
#18356 = ADVANCED_FACE ( 'NONE', ( #11386 ), #45198, .F. ) ;
#18357 = LINE ( 'NONE', #768, #36028 ) ;
#18358 = VECTOR ( 'NONE', #2181, 1000.000000000000114 ) ;
#18359 = VECTOR ( 'NONE', #43644, 999.9999999999998863 ) ;
#18360 = CARTESIAN_POINT ( 'NONE',  ( 2.072287782118878319, 0.000000000000000000, -2.950529333540147015 ) ) ;
#18361 = PLANE ( 'NONE',  #35794 ) ;
#18362 = DIRECTION ( 'NONE',  ( 0.5364919789714477361, 0.6444004775717706579, 0.5449076811759711036 ) ) ;
#18363 = LINE ( 'NONE', #5886, #16682 ) ;
#18364 = FACE_OUTER_BOUND ( 'NONE', #7342, .T. ) ;
#18365 = ORIENTED_EDGE ( 'NONE', *, *, #1132, .F. ) ;
#18366 = DIRECTION ( 'NONE',  ( -0.5364919789714478471, 0.6444004775717705469, -0.5449076811759709926 ) ) ;
#18367 = FACE_OUTER_BOUND ( 'NONE', #42605, .T. ) ;
#18368 = CARTESIAN_POINT ( 'NONE',  ( -16.99924723426068951, 0.000000000000000000, 13.49389102713827171 ) ) ;
#18369 = CARTESIAN_POINT ( 'NONE',  ( -12.72755469904986469, 0.000000000000000000, 1.966707849688810850 ) ) ;
#18370 = VECTOR ( 'NONE', #404, 1000.000000000000114 ) ;
#18371 = PLANE ( 'NONE',  #25862 ) ;
#18372 = DIRECTION ( 'NONE',  ( 0.6427681459581294776, -0.7660444431189769032, 0.005002170337467562802 ) ) ;
#18373 = LINE ( 'NONE', #31470, #52221 ) ;
#18374 = CARTESIAN_POINT ( 'NONE',  ( -67.34283022341989522, -3.900800535205241593E-15, -5.009371237985868142 ) ) ;
#18375 = EDGE_LOOP ( 'NONE', ( #19748, #12986, #28603, #51589 ) ) ;
#18376 = DIRECTION ( 'NONE',  ( 0.9999697198139515519, 0.000000000000000000, 0.007781995580013368816 ) ) ;
#18377 = DIRECTION ( 'NONE',  ( -0.5449076811759708816, 0.6444004775717707689, 0.5364919789714475140 ) ) ;
#18378 = PLANE ( 'NONE',  #21858 ) ;
#18379 = DIRECTION ( 'NONE',  ( 0.005961354470445682716, -0.6427876096865404731, -0.7660212471507180654 ) ) ;
#18380 = ADVANCED_FACE ( 'NONE', ( #6562 ), #46029, .F. ) ;
#18381 = DIRECTION ( 'NONE',  ( -0.9999697198139514409, -0.000000000000000000, -0.007781995580013368816 ) ) ;
#18382 = AXIS2_PLACEMENT_3D ( 'NONE', #24725, #33816, #29581 ) ;
#18383 = LINE ( 'NONE', #792, #54033 ) ;
#18384 = DIRECTION ( 'NONE',  ( 0.000000000000000000, -1.000000000000000000, 0.000000000000000000 ) ) ;
#18385 = CARTESIAN_POINT ( 'NONE',  ( -67.27731269685068582, -9.409571107119717226, -7.454891809856700746 ) ) ;
#18386 = AXIS2_PLACEMENT_3D ( 'NONE', #6966, #37308, #2102 ) ;
#18387 = LINE ( 'NONE', #17563, #1120 ) ;
#18388 = EDGE_CURVE ( 'NONE', #26517, #16557, #28985, .T. ) ;
#18389 = VECTOR ( 'NONE', #44072, 1000.000000000000114 ) ;
#18390 = VECTOR ( 'NONE', #11245, 999.9999999999998863 ) ;
#18391 = ORIENTED_EDGE ( 'NONE', *, *, #51392, .T. ) ;
#18392 = ADVANCED_FACE ( 'NONE', ( #36966 ), #16204, .F. ) ;
#18393 = ADVANCED_FACE ( 'NONE', ( #7389 ), #24707, .F. ) ;
#18394 = VECTOR ( 'NONE', #18622, 999.9999999999998863 ) ;
#18395 = ORIENTED_EDGE ( 'NONE', *, *, #3150, .F. ) ;
#18396 = ORIENTED_EDGE ( 'NONE', *, *, #51491, .F. ) ;
#18397 = VECTOR ( 'NONE', #43271, 1000.000000000000000 ) ;
#18398 = ORIENTED_EDGE ( 'NONE', *, *, #33878, .F. ) ;
#18399 = ORIENTED_EDGE ( 'NONE', *, *, #31867, .F. ) ;
#18400 = PLANE ( 'NONE',  #18749 ) ;
#18401 = ADVANCED_FACE ( 'NONE', ( #45731 ), #20468, .F. ) ;
#18402 = CARTESIAN_POINT ( 'NONE',  ( -10.19678563399013527, -1.000000000000000000, 0.7424042488757021108 ) ) ;
#18404 = EDGE_CURVE ( 'NONE', #19686, #20661, #19897, .T. ) ;
#18403 = ORIENTED_EDGE ( 'NONE', *, *, #2315, .F. ) ;
#18405 = ORIENTED_EDGE ( 'NONE', *, *, #8182, .T. ) ;
#18406 = VECTOR ( 'NONE', #2758, 1000.000000000000227 ) ;
#18407 = AXIS2_PLACEMENT_3D ( 'NONE', #33155, #33693, #51003 ) ;
#18408 = EDGE_CURVE ( 'NONE', #1201, #2866, #1998, .T. ) ;
#18409 = CARTESIAN_POINT ( 'NONE',  ( -15.88130887279446490, 0.000000000000000000, 3.050160814894388839 ) ) ;
#18410 = ORIENTED_EDGE ( 'NONE', *, *, #41913, .F. ) ;
#18411 = DIRECTION ( 'NONE',  ( -0.9999697198139514409, -0.000000000000000000, -0.007781995580013368816 ) ) ;
#18412 = CARTESIAN_POINT ( 'NONE',  ( -23.33849165029409889, 0.000000000000000000, 5.946783852668351855 ) ) ;
#18413 = ORIENTED_EDGE ( 'NONE', *, *, #41312, .F. ) ;
#18414 = FACE_OUTER_BOUND ( 'NONE', #24135, .T. ) ;
#18415 = AXIS2_PLACEMENT_3D ( 'NONE', #16598, #3814, #38178 ) ;
#18416 = ADVANCED_FACE ( 'NONE', ( #12222 ), #56219, .F. ) ;
#18417 = VERTEX_POINT ( 'NONE', #39175 ) ;
#18418 = CARTESIAN_POINT ( 'NONE',  ( -17.89604163440746021, 0.000000000000000000, 9.313126885395993426 ) ) ;
#18420 = AXIS2_PLACEMENT_3D ( 'NONE', #30126, #47748, #25885 ) ;
#18419 = DIRECTION ( 'NONE',  ( 0.005961354470445682716, -0.6427876096865404731, -0.7660212471507180654 ) ) ;
#18421 = EDGE_CURVE ( 'NONE', #4104, #1645, #51949, .T. ) ;
#18422 = LINE ( 'NONE', #39460, #32756 ) ;
#18423 = PLANE ( 'NONE',  #40558 ) ;
#18424 = ORIENTED_EDGE ( 'NONE', *, *, #1512, .F. ) ;
#18425 = CARTESIAN_POINT ( 'NONE',  ( -19.38307830287650191, 5.143464774974014553, 4.046874141121907797 ) ) ;
#18426 = DIRECTION ( 'NONE',  ( 0.9321478471874540261, 0.000000000000000000, -0.3620778797217456546 ) ) ;
#18427 = CARTESIAN_POINT ( 'NONE',  ( -21.31926590099137897, 1.905425754524007642, 4.902265555185135959 ) ) ;
#18428 = VECTOR ( 'NONE', #54232, 1000.000000000000227 ) ;
#18429 = ORIENTED_EDGE ( 'NONE', *, *, #33468, .T. ) ;
#18430 = DIRECTION ( 'NONE',  ( 0.007781995580012663651, 0.000000000000000000, -0.9999697198139515519 ) ) ;
#18431 = ORIENTED_EDGE ( 'NONE', *, *, #6082, .T. ) ;
#18432 = VECTOR ( 'NONE', #19052, 1000.000000000000227 ) ;
#18433 = VECTOR ( 'NONE', #50362, 1000.000000000000000 ) ;
#18434 = LINE ( 'NONE', #1675, #10171 ) ;
#18435 = DIRECTION ( 'NONE',  ( -0.5364919789714478471, 0.6444004775717705469, -0.5449076811759709926 ) ) ;
#18436 = CARTESIAN_POINT ( 'NONE',  ( -12.50746586153157303, -4.889348428825662118, 9.564509969865337524 ) ) ;
#18437 = FACE_OUTER_BOUND ( 'NONE', #41333, .T. ) ;
#18438 = LINE ( 'NONE', #1399, #45871 ) ;
#18439 = FACE_OUTER_BOUND ( 'NONE', #19285, .T. ) ;
#18440 = CARTESIAN_POINT ( 'NONE',  ( -18.59789860346329959, 0.000000000000000000, 5.783670187693309650 ) ) ;
#18441 = VECTOR ( 'NONE', #40636, 1000.000000000000227 ) ;
#18442 = DIRECTION ( 'NONE',  ( -0.1139275668495183524, 0.9934890585767659488, 4.694855797473114533E-16 ) ) ;
#18443 = VECTOR ( 'NONE', #12470, 1000.000000000000227 ) ;
#18444 = LINE ( 'NONE', #35780, #29633 ) ;
#18445 = ORIENTED_EDGE ( 'NONE', *, *, #12822, .F. ) ;
#18446 = LINE ( 'NONE', #35782, #309 ) ;
#18447 = FACE_OUTER_BOUND ( 'NONE', #53370, .T. ) ;
#18448 = CARTESIAN_POINT ( 'NONE',  ( -19.32826701083865117, 3.362543313726507499, 9.907582850272294905 ) ) ;
#18449 = CARTESIAN_POINT ( 'NONE',  ( -22.40556560354864146, -0.1191753592594197858, 5.484709000965211523 ) ) ;
#18450 = DIRECTION ( 'NONE',  ( -0.5449076811759708816, 0.6444004775717707689, 0.5364919789714475140 ) ) ;
#18451 = ADVANCED_FACE ( 'NONE', ( #34102 ), #262, .F. ) ;
#18452 = FACE_OUTER_BOUND ( 'NONE', #7887, .T. ) ;
#18453 = LINE ( 'NONE', #52274, #2070 ) ;
#18454 = ORIENTED_EDGE ( 'NONE', *, *, #13387, .T. ) ;
#18455 = ORIENTED_EDGE ( 'NONE', *, *, #14409, .F. ) ;
#18456 = VECTOR ( 'NONE', #38958, 1000.000000000000000 ) ;
#18457 = DIRECTION ( 'NONE',  ( -0.5449076811759708816, 0.6444004775717707689, 0.5364919789714475140 ) ) ;
#18458 = CARTESIAN_POINT ( 'NONE',  ( -12.40433439172452701, 0.000000000000000000, 1.599891155051114788 ) ) ;
#18459 = VECTOR ( 'NONE', #25480, 999.9999999999998863 ) ;
#18460 = ORIENTED_EDGE ( 'NONE', *, *, #12001, .T. ) ;
#18461 = DIRECTION ( 'NONE',  ( 0.000000000000000000, 0.000000000000000000, -1.000000000000000000 ) ) ;
#18462 = AXIS2_PLACEMENT_3D ( 'NONE', #43638, #4750, #43925 ) ;
#18463 = ORIENTED_EDGE ( 'NONE', *, *, #43039, .T. ) ;
#18464 = CARTESIAN_POINT ( 'NONE',  ( -13.07066190154808361, 0.000000000000000000, 12.04713590736729678 ) ) ;
#18465 = ADVANCED_FACE ( 'NONE', ( #25294 ), #42597, .F. ) ;
#18466 = ORIENTED_EDGE ( 'NONE', *, *, #3131, .T. ) ;
#18467 = ORIENTED_EDGE ( 'NONE', *, *, #7614, .F. ) ;
#18468 = ORIENTED_EDGE ( 'NONE', *, *, #12487, .F. ) ;
#18469 = DIRECTION ( 'NONE',  ( -0.6427681459581293666, -0.7660444431189770143, -0.005002170337467561935 ) ) ;
#18470 = AXIS2_PLACEMENT_3D ( 'NONE', #52681, #993, #44449 ) ;
#18471 = DIRECTION ( 'NONE',  ( 0.005002170337468016433, -0.7660444431189770143, -0.6427681459581293666 ) ) ;
#18472 = FACE_OUTER_BOUND ( 'NONE', #19797, .T. ) ;
#18473 = AXIS2_PLACEMENT_3D ( 'NONE', #15169, #32728, #28476 ) ;
#18474 = LINE ( 'NONE', #25206, #20220 ) ;
#18475 = EDGE_CURVE ( 'NONE', #35585, #6991, #4289, .T. ) ;
#18476 = ORIENTED_EDGE ( 'NONE', *, *, #41190, .F. ) ;
#18477 = ORIENTED_EDGE ( 'NONE', *, *, #48875, .T. ) ;
#18478 = EDGE_CURVE ( 'NONE', #48488, #9624, #13069, .T. ) ;
#18479 = VECTOR ( 'NONE', #45400, 1000.000000000000227 ) ;
#18480 = AXIS2_PLACEMENT_3D ( 'NONE', #54755, #32898, #24951 ) ;
#18481 = LINE ( 'NONE', #17651, #3713 ) ;
#18482 = EDGE_LOOP ( 'NONE', ( #47054, #51769, #26398, #2044 ) ) ;
#18483 = DIRECTION ( 'NONE',  ( 0.005961354470445682716, -0.6427876096865404731, -0.7660212471507180654 ) ) ;
#18484 = VERTEX_POINT ( 'NONE', #30397 ) ;
#18485 = CARTESIAN_POINT ( 'NONE',  ( -9.908141408373387193, -0.1191753592594197858, 10.77908512878318703 ) ) ;
#18486 = CARTESIAN_POINT ( 'NONE',  ( -24.27063949748155380, 0.000000000000000000, 6.308861732390097288 ) ) ;
#18487 = EDGE_CURVE ( 'NONE', #21607, #29890, #46569, .T. ) ;
#18488 = VERTEX_POINT ( 'NONE', #12520 ) ;
#18489 = CARTESIAN_POINT ( 'NONE',  ( -12.02954139919957299, -0.5179957512181571078, 1.537476745106777454 ) ) ;
#18490 = ORIENTED_EDGE ( 'NONE', *, *, #46067, .F. ) ;
#18491 = EDGE_CURVE ( 'NONE', #51394, #20189, #3430, .T. ) ;
#18492 = CARTESIAN_POINT ( 'NONE',  ( -9.342070512798265725, 0.000000000000000000, 10.59882438848031505 ) ) ;
#18493 = VECTOR ( 'NONE', #8275, 1000.000000000000114 ) ;
#18494 = ORIENTED_EDGE ( 'NONE', *, *, #55454, .F. ) ;
#18495 = CARTESIAN_POINT ( 'NONE',  ( -12.80458192191714595, 0.000000000000000000, 11.86454056839041726 ) ) ;
#18496 = DIRECTION ( 'NONE',  ( 0.5364919789714477361, 0.6444004775717706579, 0.5449076811759711036 ) ) ;
#18497 = LINE ( 'NONE', #2292, #24665 ) ;
#18498 = ORIENTED_EDGE ( 'NONE', *, *, #25297, .T. ) ;
#18499 = AXIS2_PLACEMENT_3D ( 'NONE', #49858, #28274, #37345 ) ;
#18500 = DIRECTION ( 'NONE',  ( 0.5449076811759707706, 0.6444004775717708799, -0.5364919789714476250 ) ) ;
#18501 = CARTESIAN_POINT ( 'NONE',  ( -11.14358987946894430, 0.000000000000000000, 3.256356853177110100 ) ) ;
#18502 = VECTOR ( 'NONE', #45959, 1000.000000000000227 ) ;
#18503 = CARTESIAN_POINT ( 'NONE',  ( -56.15823370927599001, 3.811598478745688023, -2.045038383219965894 ) ) ;
#18504 = DIRECTION ( 'NONE',  ( -0.005961354470445682716, -0.6427876096865404731, 0.7660212471507180654 ) ) ;
#18505 = LINE ( 'NONE', #13682, #24283 ) ;
#18506 = CARTESIAN_POINT ( 'NONE',  ( -69.06652772757389869, -9.747969413217129286, 7.053755868282013175 ) ) ;
#18507 = ORIENTED_EDGE ( 'NONE', *, *, #9412, .F. ) ;
#18508 = DIRECTION ( 'NONE',  ( 0.007781995580012663651, -3.146120232559066537E-19, -0.9999697198139514409 ) ) ;
#18509 = DIRECTION ( 'NONE',  ( 0.005002170337468016433, -0.7660444431189770143, -0.6427681459581293666 ) ) ;
#18510 = DIRECTION ( 'NONE',  ( 0.007781995580012662783, 0.000000000000000000, -0.9999697198139514409 ) ) ;
#18511 = ORIENTED_EDGE ( 'NONE', *, *, #37623, .T. ) ;
#18512 = VECTOR ( 'NONE', #8014, 1000.000000000000000 ) ;
#18513 = DIRECTION ( 'NONE',  ( -0.7660212471507179544, -0.6427876096865405842, -0.005961354470445141482 ) ) ;
#18514 = DIRECTION ( 'NONE',  ( 0.6427681459581294776, -0.7660444431189769032, 0.005002170337467562802 ) ) ;
#18515 = ORIENTED_EDGE ( 'NONE', *, *, #49439, .T. ) ;
#18516 = ADVANCED_FACE ( 'NONE', ( #26138 ), #43447, .T. ) ;
#18517 = VECTOR ( 'NONE', #14462, 1000.000000000000000 ) ;
#18518 = CARTESIAN_POINT ( 'NONE',  ( -15.96710241509184058, -0.1191753592594218814, 13.13259134697452879 ) ) ;
#18519 = LINE ( 'NONE', #909, #44796 ) ;
#18520 = EDGE_CURVE ( 'NONE', #51971, #36728, #4544, .T. ) ;
#18521 = CARTESIAN_POINT ( 'NONE',  ( -16.88915937219315921, -0.03739765774599798642, 3.380268248018597266 ) ) ;
#18522 = FACE_OUTER_BOUND ( 'NONE', #55525, .T. ) ;
#18523 = ORIENTED_EDGE ( 'NONE', *, *, #54283, .F. ) ;
#18524 = VECTOR ( 'NONE', #3382, 1000.000000000000227 ) ;
#18525 = VECTOR ( 'NONE', #8395, 1000.000000000000227 ) ;
#18526 = VERTEX_POINT ( 'NONE', #50828 ) ;
#18527 = EDGE_CURVE ( 'NONE', #36877, #46331, #12781, .T. ) ;
#18528 = PLANE ( 'NONE',  #28535 ) ;
#18529 = CARTESIAN_POINT ( 'NONE',  ( -23.33693525117809386, 0.000000000000000000, 5.746789908705562944 ) ) ;
#18530 = DIRECTION ( 'NONE',  ( -0.6427681459581293666, -0.7660444431189770143, -0.005002170337467561935 ) ) ;
#18531 = EDGE_CURVE ( 'NONE', #56226, #31598, #29253, .T. ) ;
#18532 = EDGE_CURVE ( 'NONE', #56039, #18526, #47136, .T. ) ;
#18533 = EDGE_CURVE ( 'NONE', #5817, #9950, #21306, .T. ) ;
#18534 = DIRECTION ( 'NONE',  ( -0.005961354470445682716, -0.6427876096865404731, 0.7660212471507180654 ) ) ;
#18535 = DIRECTION ( 'NONE',  ( 0.5449076811759707706, 0.6444004775717708799, -0.5364919789714476250 ) ) ;
#18536 = CARTESIAN_POINT ( 'NONE',  ( -69.61318730843225921, -8.922530380692753837, -7.503442492476276371 ) ) ;
#18537 = EDGE_LOOP ( 'NONE', ( #13586, #4000, #13810, #33284 ) ) ;
#18538 = PLANE ( 'NONE',  #18349 ) ;
#18539 = AXIS2_PLACEMENT_3D ( 'NONE', #43625, #22056, #26595 ) ;
#18540 = LINE ( 'NONE', #6072, #53274 ) ;
#18541 = ORIENTED_EDGE ( 'NONE', *, *, #55015, .T. ) ;
#18542 = VECTOR ( 'NONE', #52565, 1000.000000000000227 ) ;
#18543 = CARTESIAN_POINT ( 'NONE',  ( -10.94028622754223967, 0.000000000000000000, 11.14038480894692995 ) ) ;
#18544 = DIRECTION ( 'NONE',  ( 0.007781995580012663651, 0.000000000000000000, -0.9999697198139515519 ) ) ;
#18545 = VECTOR ( 'NONE', #33521, 999.9999999999998863 ) ;
#18546 = DIRECTION ( 'NONE',  ( 0.9999697198139515519, 0.000000000000000000, 0.007781995580013368816 ) ) ;
#18547 = ORIENTED_EDGE ( 'NONE', *, *, #34203, .T. ) ;
#18548 = LINE ( 'NONE', #44963, #39386 ) ;
#18549 = EDGE_CURVE ( 'NONE', #34742, #6991, #29566, .T. ) ;
#18550 = ORIENTED_EDGE ( 'NONE', *, *, #2115, .F. ) ;
#18552 = ORIENTED_EDGE ( 'NONE', *, *, #5349, .T. ) ;
#18551 = EDGE_CURVE ( 'NONE', #48671, #55683, #55370, .T. ) ;
#18553 = ORIENTED_EDGE ( 'NONE', *, *, #49664, .F. ) ;
#18554 = VECTOR ( 'NONE', #18286, 1000.000000000000227 ) ;
#18555 = ADVANCED_FACE ( 'NONE', ( #38638 ), #51677, .F. ) ;
#18556 = ORIENTED_EDGE ( 'NONE', *, *, #55272, .T. ) ;
#18557 = VECTOR ( 'NONE', #20131, 1000.000000000000227 ) ;
#18558 = CARTESIAN_POINT ( 'NONE',  ( -13.66676830763716488, 0.000000000000000000, 3.236720895221059102 ) ) ;
#18559 = ORIENTED_EDGE ( 'NONE', *, *, #14413, .F. ) ;
#18560 = CARTESIAN_POINT ( 'NONE',  ( 4.848100717410752658, 0.000000000000000000, 2.061810099490657411 ) ) ;
#18561 = CARTESIAN_POINT ( 'NONE',  ( 5.809281049934954311, -6.210429213608743559, -2.500000000000000444 ) ) ;
#18562 = VECTOR ( 'NONE', #37027, 1000.000000000000227 ) ;
#18563 = EDGE_CURVE ( 'NONE', #9163, #52307, #53377, .T. ) ;
#18564 = EDGE_LOOP ( 'NONE', ( #11269, #26102, #54370, #27921 ) ) ;
#18565 = DIRECTION ( 'NONE',  ( -0.5449076811759708816, 0.6444004775717707689, 0.5364919789714475140 ) ) ;
#18566 = ORIENTED_EDGE ( 'NONE', *, *, #20093, .T. ) ;
#18567 = DIRECTION ( 'NONE',  ( 0.9999697198139515519, 0.000000000000000000, 0.007781995580013368816 ) ) ;
#18568 = ORIENTED_EDGE ( 'NONE', *, *, #13099, .F. ) ;
#18569 = EDGE_CURVE ( 'NONE', #42656, #21969, #13617, .T. ) ;
#18570 = VECTOR ( 'NONE', #55761, 999.9999999999998863 ) ;
#18571 = CARTESIAN_POINT ( 'NONE',  ( -22.40478740399063895, 0.000000000000000000, 5.384712028983816623 ) ) ;
#18572 = AXIS2_PLACEMENT_3D ( 'NONE', #22526, #52605, #47813 ) ;
#18573 = CARTESIAN_POINT ( 'NONE',  ( -12.33850799832341849, 0.000000000000000000, 11.68350162852954632 ) ) ;
#18574 = LINE ( 'NONE', #49220, #53144 ) ;
#18575 = SURFACE_SIDE_STYLE ('',( #35610 ) ) ;
#18576 = LINE ( 'NONE', #31366, #11478 ) ;
#18577 = CARTESIAN_POINT ( 'NONE',  ( -13.08486533123210194, 0.000000000000000000, 1.963927175729152541 ) ) ;
#18578 = ORIENTED_EDGE ( 'NONE', *, *, #17435, .T. ) ;
#18579 = ORIENTED_EDGE ( 'NONE', *, *, #7629, .F. ) ;
#18580 = CARTESIAN_POINT ( 'NONE',  ( -25.83278826518980154, 17.74370858705499288, -4.604226652742015702 ) ) ;
#18581 = PLANE ( 'NONE',  #35742 ) ;
#18582 = CARTESIAN_POINT ( 'NONE',  ( -15.84116117370739119, 0.9340140483890051470, 2.805376761212760250 ) ) ;
#18583 = VECTOR ( 'NONE', #42812, 999.9999999999998863 ) ;
#18584 = DIRECTION ( 'NONE',  ( 0.000000000000000000, 0.000000000000000000, 1.000000000000000000 ) ) ;
#18585 = VERTEX_POINT ( 'NONE', #18744 ) ;
#18586 = VECTOR ( 'NONE', #44210, 999.9999999999998863 ) ;
#18587 = CARTESIAN_POINT ( 'NONE',  ( -13.00081981244401064, 0.000000000000000000, 3.072577446810097701 ) ) ;
#18588 = CARTESIAN_POINT ( 'NONE',  ( -12.17737215012490459, 0.4483081953215047322, 2.347176129851082482 ) ) ;
#18589 = VERTEX_POINT ( 'NONE', #9667 ) ;
#18590 = CARTESIAN_POINT ( 'NONE',  ( -18.32750754357443412, 0.000000000000000000, 5.047110293829786265 ) ) ;
#18591 = CARTESIAN_POINT ( 'NONE',  ( -19.60990026154428278, 0.000000000000000000, 4.498472333781370125 ) ) ;
#18592 = VECTOR ( 'NONE', #29117, 1000.000000000000227 ) ;
#18593 = ORIENTED_EDGE ( 'NONE', *, *, #49383, .F. ) ;
#18594 = CARTESIAN_POINT ( 'NONE',  ( -66.62599605097206279, -8.730077326369423574, -1.335442097082736534 ) ) ;
#18595 = CARTESIAN_POINT ( 'NONE',  ( -17.49593704190832355, -4.727446477803161073, 11.23649290156757452 ) ) ;
#18596 = VECTOR ( 'NONE', #40072, 999.9999999999998863 ) ;
#18597 = LINE ( 'NONE', #14062, #51319 ) ;
#18598 = DIRECTION ( 'NONE',  ( 0.005961354470445682716, -0.6427876096865404731, -0.7660212471507180654 ) ) ;
#18599 = DIRECTION ( 'NONE',  ( 0.9999697198139515519, 0.000000000000000000, 0.007781995580013368816 ) ) ;
#18600 = ORIENTED_EDGE ( 'NONE', *, *, #53265, .F. ) ;
#18601 = VECTOR ( 'NONE', #46072, 1000.000000000000227 ) ;
#18602 = STYLED_ITEM ( 'NONE', ( #9146 ), #3992 ) ;
#18603 = ORIENTED_EDGE ( 'NONE', *, *, #18001, .T. ) ;
#18604 = VECTOR ( 'NONE', #16780, 1000.000000000000227 ) ;
#18605 = LINE ( 'NONE', #43588, #46604 ) ;
#18606 = FACE_OUTER_BOUND ( 'NONE', #49591, .T. ) ;
#18607 = CARTESIAN_POINT ( 'NONE',  ( -16.89925026227929195, -0.1191753592594197858, 13.49466922669627422 ) ) ;
#18608 = AXIS2_PLACEMENT_3D ( 'NONE', #18811, #19059, #18216 ) ;
#18609 = EDGE_CURVE ( 'NONE', #48572, #49125, #27238, .T. ) ;
#18610 = EDGE_CURVE ( 'NONE', #32587, #16370, #14212, .T. ) ;
#18611 = LINE ( 'NONE', #41011, #15539 ) ;
#18612 = LINE ( 'NONE', #31098, #20340 ) ;
#18614 = ADVANCED_FACE ( 'NONE', ( #22986 ), #34943, .F. ) ;
#18613 = ORIENTED_EDGE ( 'NONE', *, *, #36040, .T. ) ;
#18615 = CARTESIAN_POINT ( 'NONE',  ( -11.87108423333901719, 3.362543313726507499, 7.010959812498333221 ) ) ;
#18616 = LINE ( 'NONE', #48986, #34731 ) ;
#18617 = VECTOR ( 'NONE', #48270, 1000.000000000000227 ) ;
#18618 = LINE ( 'NONE', #6139, #49566 ) ;
#18619 = VECTOR ( 'NONE', #2984, 1000.000000000000227 ) ;
#18620 = FACE_OUTER_BOUND ( 'NONE', #21268, .T. ) ;
#18621 = VERTEX_POINT ( 'NONE', #5125 ) ;
#18622 = DIRECTION ( 'NONE',  ( 0.007781995580012663651, 0.000000000000000000, -0.9999697198139515519 ) ) ;
#18623 = ORIENTED_EDGE ( 'NONE', *, *, #45732, .F. ) ;
#18624 = DIRECTION ( 'NONE',  ( 0.000000000000000000, -0.000000000000000000, -1.000000000000000000 ) ) ;
#18625 = LINE ( 'NONE', #48434, #29341 ) ;
#18626 = EDGE_LOOP ( 'NONE', ( #10384, #10798, #36540, #44580 ) ) ;
#18627 = CARTESIAN_POINT ( 'NONE',  ( -16.73228525469910721, 0.000000000000000000, 4.890198668954845118 ) ) ;
#18628 = EDGE_LOOP ( 'NONE', ( #40827, #29599, #46654, #29590 ) ) ;
#18629 = ADVANCED_FACE ( 'NONE', ( #17603 ), #5394, .F. ) ;
#18630 = VECTOR ( 'NONE', #37048, 999.9999999999998863 ) ;
#18631 = VERTEX_POINT ( 'NONE', #43704 ) ;
#18632 = EDGE_LOOP ( 'NONE', ( #44576, #33907, #30658, #42399 ) ) ;
#18633 = LINE ( 'NONE', #35983, #37528 ) ;
#18634 = ORIENTED_EDGE ( 'NONE', *, *, #32427, .T. ) ;
#18635 = VECTOR ( 'NONE', #8854, 999.9999999999998863 ) ;
#18636 = ORIENTED_EDGE ( 'NONE', *, *, #24734, .T. ) ;
#18637 = DIRECTION ( 'NONE',  ( 0.5364919789714477361, 0.6444004775717706579, 0.5449076811759711036 ) ) ;
#18638 = CARTESIAN_POINT ( 'NONE',  ( -20.66063881625015242, 5.467268677019012202, 13.87933419838711124 ) ) ;
#18639 = AXIS2_PLACEMENT_3D ( 'NONE', #32814, #2702, #50436 ) ;
#18640 = VERTEX_POINT ( 'NONE', #30934 ) ;
#18641 = EDGE_CURVE ( 'NONE', #46187, #32158, #35773, .T. ) ;
#18642 = ORIENTED_EDGE ( 'NONE', *, *, #28489, .T. ) ;
#18643 = CARTESIAN_POINT ( 'NONE',  ( -14.75054148647694241, -4.241740624735661491, 9.372961981961132949 ) ) ;
#18644 = ORIENTED_EDGE ( 'NONE', *, *, #54830, .F. ) ;
#18645 = VECTOR ( 'NONE', #5584, 999.9999999999998863 ) ;
#18646 = ORIENTED_EDGE ( 'NONE', *, *, #52477, .T. ) ;
#18647 = EDGE_CURVE ( 'NONE', #28250, #17105, #49094, .T. ) ;
#18648 = AXIS2_PLACEMENT_3D ( 'NONE', #52841, #13949, #31275 ) ;
#18649 = VECTOR ( 'NONE', #8159, 1000.000000000000227 ) ;
#18650 = DIRECTION ( 'NONE',  ( 0.005961354470445682716, -0.6427876096865404731, -0.7660212471507180654 ) ) ;
#18651 = EDGE_CURVE ( 'NONE', #26440, #29351, #18438, .T. ) ;
#18652 = DIRECTION ( 'NONE',  ( -0.6427681459581293666, -0.7660444431189770143, -0.005002170337467561935 ) ) ;
#18653 = CARTESIAN_POINT ( 'NONE',  ( -15.50102849149811135, -0.1191753592594197858, 12.95155240711365430 ) ) ;
#18654 = CARTESIAN_POINT ( 'NONE',  ( -12.27024259289907704, 2.229229656569006401, 1.376986556422233665 ) ) ;
#18655 = ADVANCED_FACE ( 'NONE', ( #52258 ), #40306, .F. ) ;
#18656 = ORIENTED_EDGE ( 'NONE', *, *, #47286, .F. ) ;
#18657 = CARTESIAN_POINT ( 'NONE',  ( -18.39746900504187010, 0.000000000000000000, 14.03700784672088808 ) ) ;
#18658 = VERTEX_POINT ( 'NONE', #9357 ) ;
#18659 = VECTOR ( 'NONE', #5339, 1000.000000000000000 ) ;
#18660 = VECTOR ( 'NONE', #16511, 1000.000000000000227 ) ;
#18661 = EDGE_CURVE ( 'NONE', #50133, #48446, #837, .T. ) ;
#18662 = CARTESIAN_POINT ( 'NONE',  ( -13.07066190154808361, 0.000000000000000000, 12.04713590736729678 ) ) ;
#18663 = AXIS2_PLACEMENT_3D ( 'NONE', #41589, #6671, #54628 ) ;
#18664 = LINE ( 'NONE', #40229, #55947 ) ;
#18665 = VECTOR ( 'NONE', #49468, 1000.000000000000114 ) ;
#18666 = DIRECTION ( 'NONE',  ( 0.2426528472758542054, 0.7422098413412800966, 0.6246952433987894571 ) ) ;
#18667 = DIRECTION ( 'NONE',  ( 0.9999697198139515519, 0.000000000000000000, 0.007781995580013368816 ) ) ;
#18668 = CARTESIAN_POINT ( 'NONE',  ( -19.60990026154428278, 0.000000000000000000, 4.498472333781370125 ) ) ;
#18669 = DIRECTION ( 'NONE',  ( -0.5364919789714478471, 0.6444004775717705469, -0.5449076811759709926 ) ) ;
#18670 = ORIENTED_EDGE ( 'NONE', *, *, #23603, .T. ) ;
#18671 = DIRECTION ( 'NONE',  ( 0.007781995580012662783, 0.000000000000000000, -0.9999697198139514409 ) ) ;
#18672 = ORIENTED_EDGE ( 'NONE', *, *, #28922, .F. ) ;
#18673 = CARTESIAN_POINT ( 'NONE',  ( -22.40634380310664397, 0.000000000000000000, 5.584705972946605534 ) ) ;
#18674 = DIRECTION ( 'NONE',  ( -0.5449076811759708816, 0.6444004775717707689, 0.5364919789714475140 ) ) ;
#18675 = DIRECTION ( 'NONE',  ( -0.005961354470445682716, -0.6427876096865404731, 0.7660212471507180654 ) ) ;
#18676 = PLANE ( 'NONE',  #23156 ) ;
#18677 = CARTESIAN_POINT ( 'NONE',  ( -18.79214444041551957, 0.000000000000000000, 5.043494382061776804 ) ) ;
#18678 = VECTOR ( 'NONE', #27061, 999.9999999999998863 ) ;
#18679 = CARTESIAN_POINT ( 'NONE',  ( -16.06709938707323460, 0.000000000000000000, 13.13181314741652628 ) ) ;
#18680 = AXIS2_PLACEMENT_3D ( 'NONE', #36630, #28949, #11341 ) ;
#18681 = VERTEX_POINT ( 'NONE', #26982 ) ;
#18682 = CARTESIAN_POINT ( 'NONE',  ( -14.56466625899772893, 3.848249166794011522, 2.216563428416727266 ) ) ;
#18683 = CARTESIAN_POINT ( 'NONE',  ( 2.072287782118878319, 0.000000000000000000, -2.950529333540147015 ) ) ;
#18684 = DIRECTION ( 'NONE',  ( 0.9999697198139515519, 0.000000000000000000, 0.007781995580013368816 ) ) ;
#18685 = AXIS2_PLACEMENT_3D ( 'NONE', #29339, #4065, #16012 ) ;
#18686 = ADVANCED_FACE ( 'NONE', ( #27522 ), #13895, .F. ) ;
#18687 = PLANE ( 'NONE',  #1958 ) ;
#18688 = VECTOR ( 'NONE', #17963, 999.9999999999998863 ) ;
#18689 = CARTESIAN_POINT ( 'NONE',  ( -9.850454360485084493, -0.1191753592594188005, 3.366423360904528650 ) ) ;
#18690 = LINE ( 'NONE', #31172, #35001 ) ;
#18691 = EDGE_CURVE ( 'NONE', #51439, #22392, #40014, .T. ) ;
#18692 = ADVANCED_FACE ( 'NONE', ( #30686 ), #44843, .F. ) ;
#18693 = DIRECTION ( 'NONE',  ( -0.9999697198139514409, -0.000000000000000000, -0.007781995580013368816 ) ) ;
#18694 = VECTOR ( 'NONE', #9083, 999.9999999999998863 ) ;
#18695 = VECTOR ( 'NONE', #51253, 999.9999999999998863 ) ;
#18696 = DIRECTION ( 'NONE',  ( 0.9999697198139515519, 0.000000000000000000, 0.007781995580013368816 ) ) ;
#18697 = VECTOR ( 'NONE', #5263, 1000.000000000000227 ) ;
#18698 = LINE ( 'NONE', #32579, #19242 ) ;
#18699 = AXIS2_PLACEMENT_3D ( 'NONE', #8126, #34257, #25430 ) ;
#18700 = ORIENTED_EDGE ( 'NONE', *, *, #30009, .T. ) ;
#18701 = AXIS2_PLACEMENT_3D ( 'NONE', #42780, #56146, #3886 ) ;
#18702 = EDGE_CURVE ( 'NONE', #41663, #17993, #9937, .T. ) ;
#18703 = VECTOR ( 'NONE', #22481, 1000.000000000000227 ) ;
#18704 = ORIENTED_EDGE ( 'NONE', *, *, #766, .T. ) ;
#18705 = VECTOR ( 'NONE', #18102, 1000.000000000000227 ) ;
#18706 = ORIENTED_EDGE ( 'NONE', *, *, #18404, .F. ) ;
#18707 = ORIENTED_EDGE ( 'NONE', *, *, #20854, .T. ) ;
#18708 = ORIENTED_EDGE ( 'NONE', *, *, #36979, .F. ) ;
#18709 = FACE_OUTER_BOUND ( 'NONE', #15613, .T. ) ;
#18710 = CARTESIAN_POINT ( 'NONE',  ( -8.312110554741027002, -0.1191753592594199662, 5.594387526948322531 ) ) ;
#18711 = ORIENTED_EDGE ( 'NONE', *, *, #7877, .F. ) ;
#18712 = EDGE_LOOP ( 'NONE', ( #35012, #50582, #5932, #5842 ) ) ;
#18713 = ORIENTED_EDGE ( 'NONE', *, *, #50667, .F. ) ;
#18714 = ADVANCED_FACE ( 'NONE', ( #15558 ), #24108, .F. ) ;
#18715 = AXIS2_PLACEMENT_3D ( 'NONE', #52969, #43599, #18054 ) ;
#18716 = DIRECTION ( 'NONE',  ( 0.9999697198139515519, 0.000000000000000000, 0.007781995580013368816 ) ) ;
#18717 = CARTESIAN_POINT ( 'NONE',  ( -22.23691302235923573, 4.657758921906512306, 5.170897022466190762 ) ) ;
#18718 = LINE ( 'NONE', #5374, #2338 ) ;
#18719 = EDGE_CURVE ( 'NONE', #7643, #30900, #50512, .T. ) ;
#18720 = ORIENTED_EDGE ( 'NONE', *, *, #7716, .F. ) ;
#18721 = AXIS2_PLACEMENT_3D ( 'NONE', #26144, #47991, #17910 ) ;
#18722 = CARTESIAN_POINT ( 'NONE',  ( -22.40634380310664397, 0.000000000000000000, 5.584705972946605534 ) ) ;
#18723 = ORIENTED_EDGE ( 'NONE', *, *, #4907, .F. ) ;
#18724 = LINE ( 'NONE', #15833, #15540 ) ;
#18725 = VECTOR ( 'NONE', #46832, 999.9999999999998863 ) ;
#18726 = EDGE_CURVE ( 'NONE', #38932, #18937, #20094, .T. ) ;
#18727 = DIRECTION ( 'NONE',  ( 0.000000000000000000, -0.000000000000000000, -1.000000000000000000 ) ) ;
#18728 = CARTESIAN_POINT ( 'NONE',  ( -17.43140473756637476, 0.000000000000000000, 9.316742797164003775 ) ) ;
#18729 = CARTESIAN_POINT ( 'NONE',  ( -20.64971648638756108, -1.327505506330656670, 6.881645577644349920 ) ) ;
#18730 = VECTOR ( 'NONE', #31730, 1000.000000000000227 ) ;
#18731 = DIRECTION ( 'NONE',  ( -0.5449076811759708816, 0.6444004775717707689, 0.5364919789714475140 ) ) ;
#18732 = CARTESIAN_POINT ( 'NONE',  ( -11.81396882728338582, 0.000000000000000000, 3.989803948808627432 ) ) ;
#18733 = CARTESIAN_POINT ( 'NONE',  ( -19.45503627000849889, 0.000000000000000000, 7.556996783084074742 ) ) ;
#18734 = VERTEX_POINT ( 'NONE', #1679 ) ;
#18735 = CARTESIAN_POINT ( 'NONE',  ( -17.21416647257189325, 0.000000000000000000, 7.102440976733420008 ) ) ;
#18736 = ORIENTED_EDGE ( 'NONE', *, *, #24577, .T. ) ;
#18737 = VECTOR ( 'NONE', #44469, 1000.000000000000227 ) ;
#18738 = EDGE_CURVE ( 'NONE', #41032, #20216, #19838, .T. ) ;
#18739 = AXIS2_PLACEMENT_3D ( 'NONE', #25997, #55231, #43319 ) ;
#18740 = PLANE ( 'NONE',  #46433 ) ;
#18741 = FACE_OUTER_BOUND ( 'NONE', #44089, .T. ) ;
#18742 = DIRECTION ( 'NONE',  ( 0.5364919789714477361, 0.6444004775717706579, 0.5449076811759711036 ) ) ;
#18743 = FACE_OUTER_BOUND ( 'NONE', #25708, .T. ) ;
#18744 = CARTESIAN_POINT ( 'NONE',  ( -11.60403506841546850, 0.000000000000000000, 2.714115478856362174 ) ) ;
#18745 = EDGE_CURVE ( 'NONE', #24514, #8995, #45970, .T. ) ;
#18746 = CARTESIAN_POINT ( 'NONE',  ( -12.60458797795435615, 0.000000000000000000, 11.86609696750642229 ) ) ;
#18748 = EDGE_CURVE ( 'NONE', #17790, #8254, #2769, .T. ) ;
#18747 = DIRECTION ( 'NONE',  ( 0.8660254037844378194, 0.5000000000000015543, -0.000000000000000000 ) ) ;
#18749 = AXIS2_PLACEMENT_3D ( 'NONE', #49065, #10164, #40270 ) ;
#18750 = VECTOR ( 'NONE', #35300, 1000.000000000000227 ) ;
#18751 = LINE ( 'NONE', #19570, #26586 ) ;
#18752 = FILL_AREA_STYLE ('',( #49099 ) ) ;
#18753 = CARTESIAN_POINT ( 'NONE',  ( -13.00501152033857544, 0.000000000000000000, 3.611202909362837055 ) ) ;
#18754 = ORIENTED_EDGE ( 'NONE', *, *, #48078, .T. ) ;
#18755 = DIRECTION ( 'NONE',  ( -0.005961354470445682716, -0.6427876096865404731, 0.7660212471507180654 ) ) ;
#18756 = LINE ( 'NONE', #56042, #3359 ) ;
#18757 = EDGE_CURVE ( 'NONE', #44098, #40790, #7327, .T. ) ;
#18758 = LINE ( 'NONE', #15045, #28222 ) ;
#18759 = DIRECTION ( 'NONE',  ( 0.5364919789714477361, 0.6444004775717706579, 0.5449076811759711036 ) ) ;
#18760 = EDGE_CURVE ( 'NONE', #47831, #48336, #36605, .T. ) ;
#18761 = CARTESIAN_POINT ( 'NONE',  ( -9.502280557099082259, 0.000000000000000000, 5.485122320679733043 ) ) ;
#18762 = CARTESIAN_POINT ( 'NONE',  ( -15.56423498968618269, 0.000000000000000000, 8.223277334462750332 ) ) ;
#18763 = ADVANCED_FACE ( 'NONE', ( #54208 ), #50208, .F. ) ;
#18764 = CARTESIAN_POINT ( 'NONE',  ( -13.69419118830071014, 0.000000000000000000, 6.760502168503728093 ) ) ;
#18765 = AXIS2_PLACEMENT_3D ( 'NONE', #9664, #26979, #26387 ) ;
#18766 = ORIENTED_EDGE ( 'NONE', *, *, #35101, .T. ) ;
#18767 = ORIENTED_EDGE ( 'NONE', *, *, #14851, .F. ) ;
#18768 = LINE ( 'NONE', #48858, #2318 ) ;
#18769 = PRODUCT_DEFINITION_SHAPE ( 'NONE', 'NONE',  #56238 ) ;
#18770 = DIRECTION ( 'NONE',  ( 0.5449076811759707706, 0.6444004775717708799, -0.5364919789714476250 ) ) ;
#18771 = EDGE_CURVE ( 'NONE', #56039, #23328, #49920, .T. ) ;
#18772 = EDGE_LOOP ( 'NONE', ( #36219, #37141, #24336, #54567 ) ) ;
#18773 = DIRECTION ( 'NONE',  ( -0.005961354470445682716, -0.6427876096865404731, 0.7660212471507180654 ) ) ;
#18774 = AXIS2_PLACEMENT_3D ( 'NONE', #16294, #45847, #37605 ) ;
#18775 = ORIENTED_EDGE ( 'NONE', *, *, #23792, .F. ) ;
#18776 = DIRECTION ( 'NONE',  ( -0.6427681459581293666, -0.7660444431189770143, -0.005002170337467561935 ) ) ;
#18777 = ADVANCED_FACE ( 'NONE', ( #53632 ), #2518, .F. ) ;
#18778 = VECTOR ( 'NONE', #13762, 1000.000000000000114 ) ;
#18779 = VERTEX_POINT ( 'NONE', #11317 ) ;
#18780 = EDGE_LOOP ( 'NONE', ( #20349, #40724, #16087 ) ) ;
#18781 = ORIENTED_EDGE ( 'NONE', *, *, #35590, .T. ) ;
#18782 = DIRECTION ( 'NONE',  ( 0.9321478471874538041, 0.000000000000000000, -0.3620778797217461542 ) ) ;
#18783 = CARTESIAN_POINT ( 'NONE',  ( -15.09959809284509902, 0.000000000000000000, 8.226893246230758905 ) ) ;
#18784 = LINE ( 'NONE', #19869, #30280 ) ;
#18785 = VECTOR ( 'NONE', #43987, 1000.000000000000227 ) ;
#18786 = FACE_OUTER_BOUND ( 'NONE', #27987, .T. ) ;
#18787 = ORIENTED_EDGE ( 'NONE', *, *, #29882, .T. ) ;
#18788 = ORIENTED_EDGE ( 'NONE', *, *, #36952, .F. ) ;
#18789 = VECTOR ( 'NONE', #38652, 999.9999999999998863 ) ;
#18790 = DIRECTION ( 'NONE',  ( -0.000000000000000000, -0.000000000000000000, 1.000000000000000000 ) ) ;
#18791 = ORIENTED_EDGE ( 'NONE', *, *, #53436, .T. ) ;
#18792 = CARTESIAN_POINT ( 'NONE',  ( -13.38856572258804611, -5.375054281893163477, 10.70388513002829178 ) ) ;
#18793 = ORIENTED_EDGE ( 'NONE', *, *, #15087, .F. ) ;
#18794 = FACE_OUTER_BOUND ( 'NONE', #20443, .T. ) ;
#18795 = CARTESIAN_POINT ( 'NONE',  ( 2.072287782118878319, 0.000000000000000000, -2.950529333540147015 ) ) ;
#18796 = EDGE_LOOP ( 'NONE', ( #15356, #55226, #15945, #4436 ) ) ;
#18797 = CARTESIAN_POINT ( 'NONE',  ( 2.072287782118878319, 0.000000000000000000, -2.950529333540147015 ) ) ;
#18798 = EDGE_CURVE ( 'NONE', #55742, #24350, #28650, .T. ) ;
#18799 = ORIENTED_EDGE ( 'NONE', *, *, #33611, .T. ) ;
#18800 = LINE ( 'NONE', #23043, #53593 ) ;
#18801 = ORIENTED_EDGE ( 'NONE', *, *, #3711, .T. ) ;
#18802 = CARTESIAN_POINT ( 'NONE',  ( -14.41197482399896401, 0.000000000000000000, 5.277587931052655001 ) ) ;
#18803 = DIRECTION ( 'NONE',  ( -0.7660212471507179544, -0.6427876096865405842, -0.005961354470445141482 ) ) ;
#18804 = DIRECTION ( 'NONE',  ( 0.5364919789714477361, 0.6444004775717706579, 0.5449076811759711036 ) ) ;
#18805 = ORIENTED_EDGE ( 'NONE', *, *, #42502, .F. ) ;
#18806 = EDGE_CURVE ( 'NONE', #46599, #31490, #14740, .T. ) ;
#18807 = PLANE ( 'NONE',  #36483 ) ;
#18808 = CARTESIAN_POINT ( 'NONE',  ( -69.87053270868739219, 0.6920041563027308218, 7.498947595741738859 ) ) ;
#18809 = DIRECTION ( 'NONE',  ( 0.000000000000000000, 0.000000000000000000, 1.000000000000000000 ) ) ;
#18810 = ADVANCED_FACE ( 'NONE', ( #45668 ), #49678, .F. ) ;
#18811 = CARTESIAN_POINT ( 'NONE',  ( -16.33317936670417225, 0.000000000000000000, 13.31440848639340224 ) ) ;
#18813 = EDGE_CURVE ( 'NONE', #9942, #19401, #10773, .T. ) ;
#18812 = CARTESIAN_POINT ( 'NONE',  ( -9.914677157360957338, -0.6196009389936254497, 1.468675650391051413 ) ) ;
#18814 = VECTOR ( 'NONE', #9822, 1000.000000000000000 ) ;
#18815 = CARTESIAN_POINT ( 'NONE',  ( -66.78322018952341921, -9.486696200041539129, -0.6892805327663855675 ) ) ;
#18816 = ORIENTED_EDGE ( 'NONE', *, *, #12958, .T. ) ;
#18817 = LINE ( 'NONE', #31595, #29834 ) ;
#18818 = CARTESIAN_POINT ( 'NONE',  ( -17.22698034098230480, 0.000000000000000000, 8.748995549059454646 ) ) ;
#18819 = CARTESIAN_POINT ( 'NONE',  ( -67.81219270629397045, -0.6009186479185966157, 4.328853820094372473 ) ) ;
#18820 = ORIENTED_EDGE ( 'NONE', *, *, #43869, .F. ) ;
#18821 = LINE ( 'NONE', #40675, #54664 ) ;
#18822 = CARTESIAN_POINT ( 'NONE',  ( -19.60834386242827776, 0.000000000000000000, 4.298478389818581213 ) ) ;
#18823 = EDGE_LOOP ( 'NONE', ( #17046, #27213, #39843, #510 ) ) ;
#18824 = EDGE_CURVE ( 'NONE', #49013, #43487, #23544, .T. ) ;
#18825 = DIRECTION ( 'NONE',  ( 0.9999697198139515519, 0.000000000000000000, 0.007781995580013368816 ) ) ;
#18826 = CARTESIAN_POINT ( 'NONE',  ( -19.55390298301616525, 4.172053068839008283, 11.32377094424822772 ) ) ;
#18827 = ADVANCED_FACE ( 'NONE', ( #1937 ), #19269, .F. ) ;
#18828 = CARTESIAN_POINT ( 'NONE',  ( -68.52750228004174460, 2.000000000000000000, -8.849861037685109011 ) ) ;
#18829 = ORIENTED_EDGE ( 'NONE', *, *, #11620, .T. ) ;
#18830 = ORIENTED_EDGE ( 'NONE', *, *, #14508, .T. ) ;
#18831 = DIRECTION ( 'NONE',  ( 0.000000000000000000, -1.000000000000000000, 0.000000000000000000 ) ) ;
#18832 = LINE ( 'NONE', #1758, #15122 ) ;
#18833 = DIRECTION ( 'NONE',  ( -0.5364919789714478471, 0.6444004775717705469, -0.5449076811759709926 ) ) ;
#18834 = EDGE_CURVE ( 'NONE', #50938, #606, #43111, .T. ) ;
#18835 = DIRECTION ( 'NONE',  ( -0.7660212471507179544, -0.6427876096865405842, -0.005961354470445141482 ) ) ;
#18836 = VERTEX_POINT ( 'NONE', #13005 ) ;
#18837 = CARTESIAN_POINT ( 'NONE',  ( -69.56291444385804823, -9.168415021912489138, -7.502972407220386053 ) ) ;
#18838 = ORIENTED_EDGE ( 'NONE', *, *, #19930, .F. ) ;
#18839 = LINE ( 'NONE', #53460, #12059 ) ;
#18840 = ADVANCED_FACE ( 'NONE', ( #47650 ), #12153, .F. ) ;
#18841 = CARTESIAN_POINT ( 'NONE',  ( -16.99924723426068951, 0.000000000000000000, 13.49389102713827171 ) ) ;
#18842 = VERTEX_POINT ( 'NONE', #34573 ) ;
#18843 = FACE_OUTER_BOUND ( 'NONE', #47364, .T. ) ;
#18844 = CARTESIAN_POINT ( 'NONE',  ( -12.23078190322307357, -4.565544526780662693, 8.925619156330617088 ) ) ;
#18845 = CARTESIAN_POINT ( 'NONE',  ( -17.89316758090218329, 0.000000000000000000, 8.943817182138230848 ) ) ;
#18846 = VERTEX_POINT ( 'NONE', #51044 ) ;
#18847 = DIRECTION ( 'NONE',  ( 0.5449076811759707706, 0.6444004775717708799, -0.5364919789714476250 ) ) ;
#18848 = EDGE_LOOP ( 'NONE', ( #22547, #9525, #5417, #991 ) ) ;
#18849 = VERTEX_POINT ( 'NONE', #8770 ) ;
#18850 = VECTOR ( 'NONE', #11629, 1000.000000000000227 ) ;
#18851 = ORIENTED_EDGE ( 'NONE', *, *, #7019, .T. ) ;
#18852 = CARTESIAN_POINT ( 'NONE',  ( -8.875996589204540044, 0.000000000000000000, 10.41778544861944233 ) ) ;
#18853 = ORIENTED_EDGE ( 'NONE', *, *, #43659, .T. ) ;
#18854 = CARTESIAN_POINT ( 'NONE',  ( 2.072287782118878319, 0.000000000000000000, -2.950529333540147015 ) ) ;
#18855 = ORIENTED_EDGE ( 'NONE', *, *, #43055, .F. ) ;
#18856 = DIRECTION ( 'NONE',  ( 0.9321478471874541372, 0.000000000000000000, -0.3620778797217453771 ) ) ;
#18857 = PLANE ( 'NONE',  #9573 ) ;
#18858 = VECTOR ( 'NONE', #8900, 1000.000000000000114 ) ;
#18859 = ORIENTED_EDGE ( 'NONE', *, *, #41523, .T. ) ;
#18860 = LINE ( 'NONE', #40441, #24026 ) ;
#18861 = EDGE_CURVE ( 'NONE', #34678, #34282, #38006, .T. ) ;
#18862 = ORIENTED_EDGE ( 'NONE', *, *, #27613, .T. ) ;
#18863 = CARTESIAN_POINT ( 'NONE',  ( -16.92653109165133429, 0.000000000000000000, 4.150022863323312272 ) ) ;
#18864 = EDGE_CURVE ( 'NONE', #39352, #14416, #16403, .T. ) ;
#18865 = DIRECTION ( 'NONE',  ( 0.6427681459581294776, -0.7660444431189769032, 0.005002170337467562802 ) ) ;
#18866 = DIRECTION ( 'NONE',  ( -0.000000000000000000, -0.000000000000000000, 1.000000000000000000 ) ) ;
#18867 = ADVANCED_FACE ( 'NONE', ( #7925 ), #42267, .F. ) ;
#18868 = DIRECTION ( 'NONE',  ( 1.000000000000000000, 0.000000000000000000, 0.000000000000000000 ) ) ;
#18869 = CARTESIAN_POINT ( 'NONE',  ( -13.46545670928509431, 0.000000000000000000, 3.068961535042087796 ) ) ;
#18870 = DIRECTION ( 'NONE',  ( -0.005961354470445682716, -0.6427876096865404731, 0.7660212471507180654 ) ) ;
#18871 = SURFACE_SIDE_STYLE ('',( #54055 ) ) ;
#18872 = ORIENTED_EDGE ( 'NONE', *, *, #13023, .F. ) ;
#18873 = EDGE_CURVE ( 'NONE', #50295, #8803, #42544, .T. ) ;
#18874 = EDGE_CURVE ( 'NONE', #8988, #30987, #47080, .T. ) ;
#18875 = ADVANCED_FACE ( 'NONE', ( #3372 ), #20691, .F. ) ;
#18876 = ORIENTED_EDGE ( 'NONE', *, *, #44605, .F. ) ;
#18877 = DIRECTION ( 'NONE',  ( 0.007781995580012663651, 0.000000000000000000, -0.9999697198139515519 ) ) ;
#18878 = CARTESIAN_POINT ( 'NONE',  ( -11.31245753787399089, -1.327505506330657781, 1.233109421660533833 ) ) ;
#18879 = PLANE ( 'NONE',  #36056 ) ;
#18880 = CARTESIAN_POINT ( 'NONE',  ( -10.88337737921193948, 0.000000000000000000, 3.827720013049670023 ) ) ;
#18881 = EDGE_LOOP ( 'NONE', ( #19237, #1064, #48376, #51659 ) ) ;
#18882 = CARTESIAN_POINT ( 'NONE',  ( -14.94916102560700821, 0.000000000000000000, 2.688082935172642962 ) ) ;
#18883 = DIRECTION ( 'NONE',  ( -0.9999697198139514409, -0.000000000000000000, -0.007781995580013368816 ) ) ;
#18884 = EDGE_LOOP ( 'NONE', ( #19263, #16363, #21626, #39090 ) ) ;
#18885 = DIRECTION ( 'NONE',  ( 0.000000000000000000, -0.000000000000000000, -1.000000000000000000 ) ) ;
#18886 = DIRECTION ( 'NONE',  ( -0.005961354470445682716, -0.6427876096865404731, 0.7660212471507180654 ) ) ;
#18887 = ORIENTED_EDGE ( 'NONE', *, *, #32404, .T. ) ;
#18888 = CARTESIAN_POINT ( 'NONE',  ( -67.71196402477201559, -8.854389638963908737, 5.199837068550139385 ) ) ;
#18889 = CARTESIAN_POINT ( 'NONE',  ( -11.37769377693735962, 0.000000000000000000, 7.637856226733343412 ) ) ;
#18890 = EDGE_CURVE ( 'NONE', #48904, #34052, #3062, .T. ) ;
#18891 = CARTESIAN_POINT ( 'NONE',  ( -17.46532115785441519, 0.000000000000000000, 13.67492996699914265 ) ) ;
#18892 = DIRECTION ( 'NONE',  ( 0.000000000000000000, -1.000000000000000000, 0.000000000000000000 ) ) ;
#18893 = EDGE_CURVE ( 'NONE', #23668, #50643, #8186, .T. ) ;
#18894 = CARTESIAN_POINT ( 'NONE',  ( -27.99923088623136636, 0.000000000000000000, 7.757173251277078130 ) ) ;
#18895 = ORIENTED_EDGE ( 'NONE', *, *, #6002, .T. ) ;
#18896 = EDGE_LOOP ( 'NONE', ( #45562, #29844, #30527, #6517 ) ) ;
#18897 = EDGE_CURVE ( 'NONE', #25320, #17870, #20392, .T. ) ;
#18898 = DIRECTION ( 'NONE',  ( -0.7660212471507179544, -0.6427876096865405842, -0.005961354470445141482 ) ) ;
#18899 = DIRECTION ( 'NONE',  ( 0.005961354470445682716, -0.6427876096865404731, -0.7660212471507180654 ) ) ;
#18900 = CARTESIAN_POINT ( 'NONE',  ( -14.46888367232926420, 0.000000000000000000, 12.59025272694991315 ) ) ;
#18901 = EDGE_CURVE ( 'NONE', #10313, #25745, #47350, .T. ) ;
#18902 = VECTOR ( 'NONE', #7209, 1000.000000000000227 ) ;
#18903 = DIRECTION ( 'NONE',  ( 0.9999697198139515519, 0.000000000000000000, 0.007781995580013368816 ) ) ;
#18904 = CARTESIAN_POINT ( 'NONE',  ( -8.186969886387416295, 7.982592133067664797, 6.398470710204317236 ) ) ;
#18905 = ORIENTED_EDGE ( 'NONE', *, *, #18189, .T. ) ;
#18906 = DIRECTION ( 'NONE',  ( 0.7660212471507180654, -0.6427876096865404731, 0.005961354470445141482 ) ) ;
#18907 = PLANE ( 'NONE',  #3922 ) ;
#18908 = LINE ( 'NONE', #6394, #7817 ) ;
#18909 = LINE ( 'NONE', #5841, #13337 ) ;
#18910 = VERTEX_POINT ( 'NONE', #7615 ) ;
#18911 = DIRECTION ( 'NONE',  ( -0.005002170337468016433, -0.7660444431189770143, 0.6427681459581293666 ) ) ;
#18912 = VERTEX_POINT ( 'NONE', #42804 ) ;
#18913 = LINE ( 'NONE', #45851, #22314 ) ;
#18914 = CARTESIAN_POINT ( 'NONE',  ( -21.12007069142898885, 1.095915999411505082, 6.883658674416231804 ) ) ;
#18915 = ORIENTED_EDGE ( 'NONE', *, *, #27342, .T. ) ;
#18916 = LINE ( 'NONE', #44732, #6393 ) ;
#18917 = ORIENTED_EDGE ( 'NONE', *, *, #18824, .F. ) ;
#18918 = VERTEX_POINT ( 'NONE', #8459 ) ;
#18919 = ORIENTED_EDGE ( 'NONE', *, *, #12533, .T. ) ;
#18920 = DIRECTION ( 'NONE',  ( -0.5364919789714478471, 0.6444004775717705469, -0.5449076811759709926 ) ) ;
#18921 = VERTEX_POINT ( 'NONE', #38268 ) ;
#18922 = VERTEX_POINT ( 'NONE', #37734 ) ;
#18923 = CARTESIAN_POINT ( 'NONE',  ( -17.46532115785441519, 0.000000000000000000, 13.67492996699914265 ) ) ;
#18924 = CARTESIAN_POINT ( 'NONE',  ( -15.40103151951671734, 0.000000000000000000, 12.95233060667165681 ) ) ;
#18925 = EDGE_LOOP ( 'NONE', ( #13797, #55407, #18707, #14994 ) ) ;
#18926 = ORIENTED_EDGE ( 'NONE', *, *, #51462, .F. ) ;
#18927 = LINE ( 'NONE', #31437, #5015 ) ;
#18928 = ORIENTED_EDGE ( 'NONE', *, *, #21951, .T. ) ;
#18929 = EDGE_CURVE ( 'NONE', #41830, #38527, #55591, .T. ) ;
#18930 = ORIENTED_EDGE ( 'NONE', *, *, #38865, .T. ) ;
#18931 = DIRECTION ( 'NONE',  ( 0.000000000000000000, -0.000000000000000000, -1.000000000000000000 ) ) ;
#18932 = DIRECTION ( 'NONE',  ( 0.7660212471507180654, -0.6427876096865404731, 0.005961354470445141482 ) ) ;
#18933 = DIRECTION ( 'NONE',  ( 0.005002170337468016433, -0.7660444431189770143, -0.6427681459581293666 ) ) ;
#18934 = DIRECTION ( 'NONE',  ( -0.005002170337468016433, -0.7660444431189770143, 0.6427681459581293666 ) ) ;
#18935 = EDGE_LOOP ( 'NONE', ( #47483, #21170, #37471, #17880 ) ) ;
#18936 = CARTESIAN_POINT ( 'NONE',  ( -11.84270936233621008, 0.000000000000000000, 7.682900981386271866 ) ) ;
#18937 = VERTEX_POINT ( 'NONE', #17251 ) ;
#18938 = EDGE_CURVE ( 'NONE', #55190, #52574, #56167, .T. ) ;
#18939 = EDGE_CURVE ( 'NONE', #38452, #165, #12465, .T. ) ;
#18940 = ADVANCED_FACE ( 'NONE', ( #55896 ), #34316, .F. ) ;
#18941 = AXIS2_PLACEMENT_3D ( 'NONE', #39556, #4898, #38981 ) ;
#18942 = DIRECTION ( 'NONE',  ( -0.5449076811759708816, 0.6444004775717707689, 0.5364919789714475140 ) ) ;
#18943 = ADVANCED_FACE ( 'NONE', ( #31467 ), #31158, .F. ) ;
#18944 = DIRECTION ( 'NONE',  ( 0.007781995580012662783, 0.000000000000000000, -0.9999697198139514409 ) ) ;
#18945 = DIRECTION ( 'NONE',  ( -0.9999697198139514409, -0.000000000000000000, -0.007781995580013368816 ) ) ;
#18946 = DIRECTION ( 'NONE',  ( 0.5364919789714477361, 0.6444004775717706579, 0.5449076811759711036 ) ) ;
#18947 = CARTESIAN_POINT ( 'NONE',  ( -28.93060053386082231, -0.1191753592594197858, 8.019254159017428663 ) ) ;
#18948 = CARTESIAN_POINT ( 'NONE',  ( -24.26986129792355129, -0.1191753592594197858, 6.208864760408702388 ) ) ;
#18949 = ORIENTED_EDGE ( 'NONE', *, *, #52297, .F. ) ;
#18950 = DIRECTION ( 'NONE',  ( -0.9999697198139514409, -0.000000000000000000, -0.007781995580013368816 ) ) ;
#18951 = ORIENTED_EDGE ( 'NONE', *, *, #41517, .F. ) ;
#18952 = DIRECTION ( 'NONE',  ( -0.005961354470445682716, -0.6427876096865404731, 0.7660212471507180654 ) ) ;
#18953 = CARTESIAN_POINT ( 'NONE',  ( -21.47341775636118655, -0.1191753592594197858, 5.122631121243466090 ) ) ;
#18954 = PLANE ( 'NONE',  #11806 ) ;
#18955 = FACE_OUTER_BOUND ( 'NONE', #27320, .T. ) ;
#18956 = ADVANCED_FACE ( 'NONE', ( #35173 ), #18371, .F. ) ;
#18957 = CARTESIAN_POINT ( 'NONE',  ( -12.60458797795435615, 0.000000000000000000, 11.86609696750642229 ) ) ;
#18958 = CARTESIAN_POINT ( 'NONE',  ( -67.32595136268157887, -0.9999999999999978906, 0.5932824550257459473 ) ) ;
#18959 = ORIENTED_EDGE ( 'NONE', *, *, #33796, .F. ) ;
#18960 = EDGE_CURVE ( 'NONE', #3752, #18987, #54913, .T. ) ;
#18961 = CARTESIAN_POINT ( 'NONE',  ( -28.28184430289702789, 14.59769461685536740, 4.726375084653139602 ) ) ;
#18962 = FACE_OUTER_BOUND ( 'NONE', #48745, .T. ) ;
#18963 = CARTESIAN_POINT ( 'NONE',  ( -63.00984630926864583, 1.788483511016180305, -3.000000000000007105 ) ) ;
#18964 = ADVANCED_FACE ( 'NONE', ( #16899 ), #34230, .F. ) ;
#18965 = CARTESIAN_POINT ( 'NONE',  ( -14.46888367232926420, 0.000000000000000000, 12.59025272694991315 ) ) ;
#18966 = DIRECTION ( 'NONE',  ( -0.7660212471507179544, -0.6427876096865405842, -0.005961354470445141482 ) ) ;
#18967 = PLANE ( 'NONE',  #39224 ) ;
#18968 = EDGE_CURVE ( 'NONE', #29513, #55994, #12046, .T. ) ;
#18969 = CARTESIAN_POINT ( 'NONE',  ( -16.07347840383240012, -3.108426967578160838, 3.025630892186666809 ) ) ;
#18970 = LINE ( 'NONE', #2479, #32864 ) ;
#18971 = ORIENTED_EDGE ( 'NONE', *, *, #24050, .T. ) ;
#18972 = EDGE_LOOP ( 'NONE', ( #29361, #54339, #17033, #30674 ) ) ;
#18973 = ORIENTED_EDGE ( 'NONE', *, *, #33967, .F. ) ;
#18974 = ORIENTED_EDGE ( 'NONE', *, *, #5465, .T. ) ;
#18975 = ORIENTED_EDGE ( 'NONE', *, *, #43848, .T. ) ;
#18976 = CARTESIAN_POINT ( 'NONE',  ( -33.59056157024009082, 0.000000000000000000, 9.729646585644761814 ) ) ;
#18977 = LINE ( 'NONE', #6750, #53886 ) ;
#18978 = VERTEX_POINT ( 'NONE', #25986 ) ;
#18979 = EDGE_LOOP ( 'NONE', ( #51227, #11084, #34471, #22869 ) ) ;
#18980 = VERTEX_POINT ( 'NONE', #8093 ) ;
#18981 = DIRECTION ( 'NONE',  ( 0.5449076811759707706, 0.6444004775717708799, -0.5364919789714476250 ) ) ;
#18982 = LINE ( 'NONE', #50181, #11953 ) ;
#18983 = DIRECTION ( 'NONE',  ( 0.005002170337468016433, -0.7660444431189770143, -0.6427681459581293666 ) ) ;
#18984 = ORIENTED_EDGE ( 'NONE', *, *, #35132, .F. ) ;
#18985 = DIRECTION ( 'NONE',  ( 0.5364919789714477361, 0.6444004775717706579, 0.5449076811759711036 ) ) ;
#18987 = VERTEX_POINT ( 'NONE', #34760 ) ;
#18986 = EDGE_CURVE ( 'NONE', #345, #33161, #4112, .T. ) ;
#18988 = LINE ( 'NONE', #36306, #32783 ) ;
#18989 = DIRECTION ( 'NONE',  ( 0.007781995580012663651, -3.146120232559066537E-19, -0.9999697198139514409 ) ) ;
#18990 = EDGE_CURVE ( 'NONE', #50596, #39497, #42451, .T. ) ;
#18991 = EDGE_CURVE ( 'NONE', #34361, #30589, #37912, .T. ) ;
#18992 = DIRECTION ( 'NONE',  ( 0.005002170337468016433, -0.7660444431189770143, -0.6427681459581293666 ) ) ;
#18993 = DIRECTION ( 'NONE',  ( -0.005002170337468016433, -0.7660444431189770143, 0.6427681459581293666 ) ) ;
#18994 = LINE ( 'NONE', #36311, #36762 ) ;
#18995 = CARTESIAN_POINT ( 'NONE',  ( 2.072287782118878319, 0.000000000000000000, -2.950529333540147015 ) ) ;
#18996 = PLANE ( 'NONE',  #11296 ) ;
#18997 = VERTEX_POINT ( 'NONE', #3807 ) ;
#18998 = LINE ( 'NONE', #48830, #48256 ) ;
#18999 = VERTEX_POINT ( 'NONE', #43555 ) ;
#19000 =( GEOMETRIC_REPRESENTATION_CONTEXT ( 3 ) GLOBAL_UNCERTAINTY_ASSIGNED_CONTEXT ( ( #3558 ) ) GLOBAL_UNIT_ASSIGNED_CONTEXT ( ( #11031, #40863, #33466 ) ) REPRESENTATION_CONTEXT ( 'NONE', 'WORKASPACE' ) );
#19001 = CARTESIAN_POINT ( 'NONE',  ( -14.00280974873554030, 0.000000000000000000, 12.40921378708904044 ) ) ;
#19002 = CARTESIAN_POINT ( 'NONE',  ( -20.54126990917373519, -0.1191753592594197858, 4.760553241521720658 ) ) ;
#19003 = CARTESIAN_POINT ( 'NONE',  ( -8.956466202847114033, -0.1191753592594181482, 6.697369211722168814 ) ) ;
#19004 = CARTESIAN_POINT ( 'NONE',  ( -14.54398777498582618, 1.581621852479005552, 5.126410796805221715 ) ) ;
#19005 = CARTESIAN_POINT ( 'NONE',  ( -17.70545686808230101, 0.9340140483890051470, 3.529532520656252448 ) ) ;
#19006 = DIRECTION ( 'NONE',  ( 0.9999697198139515519, 0.000000000000000000, 0.007781995580013368816 ) ) ;
#19007 = DIRECTION ( 'NONE',  ( 0.007781995580012663651, -3.146120232559066537E-19, -0.9999697198139514409 ) ) ;
#19008 = CARTESIAN_POINT ( 'NONE',  ( -15.42828644624678169, -0.6798977022406558213, 2.852499223360160929 ) ) ;
#19009 = SHAPE_REPRESENTATION_RELATIONSHIP ( 'NONE' , 'NONE' ,  #12294, #29299 ) ;
#19010 = PLANE ( 'NONE',  #14739 ) ;
#19011 = EDGE_LOOP ( 'NONE', ( #9706, #54369, #45052, #48000 ) ) ;
#19012 = DIRECTION ( 'NONE',  ( 0.005961354470445682716, -0.6427876096865404731, -0.7660212471507180654 ) ) ;
#19013 = LINE ( 'NONE', #19575, #4074 ) ;
#19014 = DIRECTION ( 'NONE',  ( 0.005961354470445682716, -0.6427876096865404731, -0.7660212471507180654 ) ) ;
#19015 = LINE ( 'NONE', #9371, #55769 ) ;
#19016 = CARTESIAN_POINT ( 'NONE',  ( -27.99845268667336384, -0.1191753592594197858, 7.657176279295684118 ) ) ;
#19017 = ADVANCED_FACE ( 'NONE', ( #30228 ), #21130, .F. ) ;
#19018 = LINE ( 'NONE', #23297, #8821 ) ;
#19019 = CARTESIAN_POINT ( 'NONE',  ( -18.04694319155812821, 0.7721120973665051013, 5.158534221716275958 ) ) ;
#19020 = ORIENTED_EDGE ( 'NONE', *, *, #31442, .F. ) ;
#19021 = ORIENTED_EDGE ( 'NONE', *, *, #49041, .T. ) ;
#19022 = ADVANCED_FACE ( 'NONE', ( #7824 ), #46701, .F. ) ;
#19023 = DIRECTION ( 'NONE',  ( 0.6427681459581294776, -0.7660444431189769032, 0.005002170337467562802 ) ) ;
#19024 = LINE ( 'NONE', #26411, #8718 ) ;
#19025 = ORIENTED_EDGE ( 'NONE', *, *, #37680, .F. ) ;
#19026 = LINE ( 'NONE', #9956, #1372 ) ;
#19027 = ADVANCED_FACE ( 'NONE', ( #33923 ), #12629, .F. ) ;
#19028 = ORIENTED_EDGE ( 'NONE', *, *, #13980, .T. ) ;
#19029 = DIRECTION ( 'NONE',  ( 0.7660212471507180654, -0.6427876096865404731, 0.005961354470445141482 ) ) ;
#19030 = ORIENTED_EDGE ( 'NONE', *, *, #55323, .F. ) ;
#19031 = ORIENTED_EDGE ( 'NONE', *, *, #46294, .T. ) ;
#19032 = EDGE_LOOP ( 'NONE', ( #26189, #47494, #12390, #32789 ) ) ;
#19033 = DIRECTION ( 'NONE',  ( 0.005961354470445682716, -0.6427876096865404731, -0.7660212471507180654 ) ) ;
#19034 = DIRECTION ( 'NONE',  ( -0.9999697198139514409, -0.000000000000000000, -0.007781995580013368816 ) ) ;
#19035 = CARTESIAN_POINT ( 'NONE',  ( -21.47419595591918906, 0.000000000000000000, 5.222628093224860102 ) ) ;
#19036 = EDGE_LOOP ( 'NONE', ( #50797, #20017, #39199, #27478 ) ) ;
#19037 = ORIENTED_EDGE ( 'NONE', *, *, #42845, .F. ) ;
#19038 = PLANE ( 'NONE',  #48143 ) ;
#19039 = ORIENTED_EDGE ( 'NONE', *, *, #23325, .F. ) ;
#19040 = CARTESIAN_POINT ( 'NONE',  ( -15.40103151951671734, 0.000000000000000000, 12.95233060667165681 ) ) ;
#19041 = EDGE_CURVE ( 'NONE', #15321, #29206, #38764, .T. ) ;
#19042 = EDGE_LOOP ( 'NONE', ( #31971, #50865, #54481, #2047 ) ) ;
#19043 = LINE ( 'NONE', #28699, #48455 ) ;
#19044 = CARTESIAN_POINT ( 'NONE',  ( 5.385059872733034325, 0.000000000000000000, -0.6896135826588374318 ) ) ;
#19045 = ORIENTED_EDGE ( 'NONE', *, *, #45436, .F. ) ;
#19046 = CARTESIAN_POINT ( 'NONE',  ( -13.07066190154808361, 0.000000000000000000, 12.04713590736729678 ) ) ;
#19047 = EDGE_LOOP ( 'NONE', ( #22841, #28104, #8691, #19478 ) ) ;
#19048 = EDGE_CURVE ( 'NONE', #8803, #3951, #35072, .T. ) ;
#19049 = PLANE ( 'NONE',  #14608 ) ;
#19050 = EDGE_LOOP ( 'NONE', ( #44398, #22107, #4242, #26587 ) ) ;
#19051 = DIRECTION ( 'NONE',  ( -0.6427681459581293666, -0.7660444431189770143, -0.005002170337467561935 ) ) ;
#19052 = DIRECTION ( 'NONE',  ( 0.007781995580012662783, 0.000000000000000000, -0.9999697198139514409 ) ) ;
#19053 = DIRECTION ( 'NONE',  ( -0.6427681459581293666, -0.7660444431189770143, -0.005002170337467561935 ) ) ;
#19054 = VERTEX_POINT ( 'NONE', #27088 ) ;
#19055 = FACE_OUTER_BOUND ( 'NONE', #12923, .T. ) ;
#19056 = CARTESIAN_POINT ( 'NONE',  ( -9.342070512798265725, 0.000000000000000000, 10.59882438848031505 ) ) ;
#19057 = CARTESIAN_POINT ( 'NONE',  ( -21.15203641687357461, -2.460819163488157546, 8.936724485154998732 ) ) ;
#19058 = CARTESIAN_POINT ( 'NONE',  ( -19.18055499287547860, -0.1191753592594166911, 8.095131267895274263 ) ) ;
#19059 = DIRECTION ( 'NONE',  ( 0.7660212471507180654, -0.6427876096865404731, 0.005961354470445141482 ) ) ;
#19060 = PLANE ( 'NONE',  #49697 ) ;
#19061 = EDGE_CURVE ( 'NONE', #45704, #36899, #40131, .T. ) ;
#19062 = VECTOR ( 'NONE', #31731, 1000.000000000000227 ) ;
#19063 = CARTESIAN_POINT ( 'NONE',  ( -67.73318103894531816, -9.595695390205156272, 4.678579668398631597 ) ) ;
#19064 = ORIENTED_EDGE ( 'NONE', *, *, #54626, .T. ) ;
#19065 = DIRECTION ( 'NONE',  ( 0.007781995580012663651, 0.000000000000000000, -0.9999697198139515519 ) ) ;
#19066 = LINE ( 'NONE', #44619, #2303 ) ;
#19067 = CARTESIAN_POINT ( 'NONE',  ( -67.09318657654290519, -0.6008575946992210648, -1.359962337613763950 ) ) ;
#19068 = VERTEX_POINT ( 'NONE', #18560 ) ;
#19069 = CARTESIAN_POINT ( 'NONE',  ( -15.82157343643791236, 0.000000000000000000, 7.282604471332424723 ) ) ;
#19070 = CARTESIAN_POINT ( 'NONE',  ( -14.02358693954004210, -0.1191753592594190225, 2.228863834670655741 ) ) ;
#19071 = DIRECTION ( 'NONE',  ( 0.9999697198139515519, 0.000000000000000000, 0.007781995580013368816 ) ) ;
#19072 = DIRECTION ( 'NONE',  ( -0.9999697198139514409, -0.000000000000000000, -0.007781995580013368816 ) ) ;
#19073 = LINE ( 'NONE', #50000, #41084 ) ;
#19074 = VERTEX_POINT ( 'NONE', #10325 ) ;
#19075 = VERTEX_POINT ( 'NONE', #53479 ) ;
#19076 =( BOUNDED_CURVE ( )  B_SPLINE_CURVE ( 3, ( #6283, #19044, #32416, #19316 ),
 .UNSPECIFIED., .F., .F. ) 
 B_SPLINE_CURVE_WITH_KNOTS ( ( 4, 4 ),
 ( 5.898329122556067894, 6.668041491803113452 ),
 .UNSPECIFIED. ) 
 CURVE ( )  GEOMETRIC_REPRESENTATION_ITEM ( )  RATIONAL_B_SPLINE_CURVE ( ( 1.000000000000000000, 0.9512349561781446861, 0.9512349561781446861, 1.000000000000000000 ) ) 
 REPRESENTATION_ITEM ( '' )  );
#19077 = CARTESIAN_POINT ( 'NONE',  ( 2.072287782118878319, 0.000000000000000000, -2.950529333540147015 ) ) ;
#19078 = DIRECTION ( 'NONE',  ( 0.005961354470445682716, -0.6427876096865404731, -0.7660212471507180654 ) ) ;
#19079 = CARTESIAN_POINT ( 'NONE',  ( -19.84220772623944740, 1.257817950434005683, 4.349188078554292680 ) ) ;
#19080 = ORIENTED_EDGE ( 'NONE', *, *, #20488, .T. ) ;
#19081 = PLANE ( 'NONE',  #43938 ) ;
#19082 = EDGE_CURVE ( 'NONE', #19083, #33225, #52376, .T. ) ;
#19083 = VERTEX_POINT ( 'NONE', #48369 ) ;
#19084 = DIRECTION ( 'NONE',  ( -0.005961354470445682716, -0.6427876096865404731, 0.7660212471507180654 ) ) ;
#19085 = DIRECTION ( 'NONE',  ( -0.5364919789714478471, 0.6444004775717705469, -0.5449076811759709926 ) ) ;
#19086 = ORIENTED_EDGE ( 'NONE', *, *, #13742, .T. ) ;
#19087 = FACE_OUTER_BOUND ( 'NONE', #46100, .T. ) ;
#19088 = DIRECTION ( 'NONE',  ( 0.6427681459581294776, -0.7660444431189769032, 0.005002170337467562802 ) ) ;
#19089 = DIRECTION ( 'NONE',  ( 0.005961354470445682716, -0.6427876096865404731, -0.7660212471507180654 ) ) ;
#19090 = ADVANCED_FACE ( 'NONE', ( #44394 ), #689, .F. ) ;
#19091 = EDGE_LOOP ( 'NONE', ( #4262, #23337, #5521, #23355 ) ) ;
#19092 = DIRECTION ( 'NONE',  ( 0.007781995580012663651, -3.146120232559066537E-19, -0.9999697198139514409 ) ) ;
#19093 = VERTEX_POINT ( 'NONE', #52627 ) ;
#19094 = ADVANCED_FACE ( 'NONE', ( #13475 ), #941, .F. ) ;
#19095 = ADVANCED_FACE ( 'NONE', ( #53224 ), #14579, .F. ) ;
#19096 = AXIS2_PLACEMENT_3D ( 'NONE', #2012, #10589, #24188 ) ;
#19097 = EDGE_LOOP ( 'NONE', ( #45873, #15517, #46640, #15691 ) ) ;
#19098 = VERTEX_POINT ( 'NONE', #48090 ) ;
#19099 = PLANE ( 'NONE',  #51281 ) ;
#19100 = EDGE_LOOP ( 'NONE', ( #9973, #2871, #16865, #38941 ) ) ;
#19101 = CARTESIAN_POINT ( 'NONE',  ( -16.81902912537577777, -2.298917212465658277, 6.987928619639786731 ) ) ;
#19102 = EDGE_CURVE ( 'NONE', #9089, #26894, #9783, .T. ) ;
#19103 = VERTEX_POINT ( 'NONE', #22552 ) ;
#19104 = CARTESIAN_POINT ( 'NONE',  ( -13.45970860227452981, 0.000000000000000000, 2.330342128526559087 ) ) ;
#19105 = CARTESIAN_POINT ( 'NONE',  ( -9.597601843825197321, -1.410310748667299885, 2.284967082322166387 ) ) ;
#19106 = ORIENTED_EDGE ( 'NONE', *, *, #10615, .F. ) ;
#19107 = ADVANCED_FACE ( 'NONE', ( #14324 ), #22812, .F. ) ;
#19108 = CARTESIAN_POINT ( 'NONE',  ( -27.99767448711536133, 0.000000000000000000, 7.557179307314289218 ) ) ;
#19109 = ORIENTED_EDGE ( 'NONE', *, *, #44884, .T. ) ;
#19110 = EDGE_CURVE ( 'NONE', #40075, #15737, #10037, .T. ) ;
#19111 = DIRECTION ( 'NONE',  ( -0.005002170337468016433, -0.7660444431189770143, 0.6427681459581293666 ) ) ;
#19112 = CARTESIAN_POINT ( 'NONE',  ( -9.808144436391993182, 0.000000000000000000, 10.77986332834118777 ) ) ;
#19113 = LINE ( 'NONE', #52926, #1449 ) ;
#19114 = DIRECTION ( 'NONE',  ( 0.000000000000000000, 1.000000000000000000, 0.000000000000000000 ) ) ;
#19115 = CARTESIAN_POINT ( 'NONE',  ( -16.33317936670417225, 0.000000000000000000, 13.31440848639340224 ) ) ;
#19116 = DIRECTION ( 'NONE',  ( 0.9999697198139515519, 0.000000000000000000, 0.007781995580013368816 ) ) ;
#19117 = CARTESIAN_POINT ( 'NONE',  ( -10.47421230394850866, 0.000000000000000000, 10.95934586908605723 ) ) ;
#19118 = ORIENTED_EDGE ( 'NONE', *, *, #51759, .F. ) ;
#19119 = EDGE_CURVE ( 'NONE', #47218, #47771, #4658, .T. ) ;
#19120 = ORIENTED_EDGE ( 'NONE', *, *, #36604, .T. ) ;
#19121 = VECTOR ( 'NONE', #55002, 1000.000000000000114 ) ;
#19122 = FACE_OUTER_BOUND ( 'NONE', #38067, .T. ) ;
#19123 = DIRECTION ( 'NONE',  ( -0.6427681459581293666, -0.7660444431189770143, -0.005002170337467561935 ) ) ;
#19124 = DIRECTION ( 'NONE',  ( 0.5449076811759707706, 0.6444004775717708799, -0.5364919789714476250 ) ) ;
#19125 = EDGE_CURVE ( 'NONE', #36112, #3699, #21971, .T. ) ;
#19126 = FACE_OUTER_BOUND ( 'NONE', #25457, .T. ) ;
#19127 = ORIENTED_EDGE ( 'NONE', *, *, #8971, .T. ) ;
#19128 = LINE ( 'NONE', #31382, #37618 ) ;
#19129 = DIRECTION ( 'NONE',  ( 0.000000000000000000, -1.000000000000000000, 0.000000000000000000 ) ) ;
#19130 = ORIENTED_EDGE ( 'NONE', *, *, #11495, .F. ) ;
#19131 = PLANE ( 'NONE',  #10251 ) ;
#19132 = PLANE ( 'NONE',  #49435 ) ;
#19133 = ORIENTED_EDGE ( 'NONE', *, *, #20953, .T. ) ;
#19134 = CARTESIAN_POINT ( 'NONE',  ( -70.53061787018394568, 1.999999999999998224, -8.307376767094712733 ) ) ;
#19135 = CARTESIAN_POINT ( 'NONE',  ( -10.14379749791080876, 0.000000000000000000, 0.8788190362434851188 ) ) ;
#19136 = VECTOR ( 'NONE', #8515, 999.9999999999998863 ) ;
#19137 = LINE ( 'NONE', #41569, #47715 ) ;
#19138 = CARTESIAN_POINT ( 'NONE',  ( -12.15116108492864377, 0.000000000000000000, 1.401855352044617975 ) ) ;
#19139 = VECTOR ( 'NONE', #41078, 1000.000000000000227 ) ;
#19140 = CARTESIAN_POINT ( 'NONE',  ( -16.81190032086591302, 0.000000000000000000, 3.212244750653343583 ) ) ;
#19141 = VERTEX_POINT ( 'NONE', #40437 ) ;
#19142 = ORIENTED_EDGE ( 'NONE', *, *, #40424, .T. ) ;
#19143 = CARTESIAN_POINT ( 'NONE',  ( 2.072287782118878319, 0.000000000000000000, -2.950529333540147015 ) ) ;
#19144 = FACE_OUTER_BOUND ( 'NONE', #3868, .T. ) ;
#19145 = CARTESIAN_POINT ( 'NONE',  ( -13.04105656151796744, 0.000000000000000000, 8.242913292418799998 ) ) ;
#19146 = PLANE ( 'NONE',  #11006 ) ;
#19147 = DIRECTION ( 'NONE',  ( -0.5364919789714478471, 0.6444004775717705469, -0.5449076811759709926 ) ) ;
#19148 = EDGE_CURVE ( 'NONE', #20170, #27352, #39301, .T. ) ;
#19149 = ORIENTED_EDGE ( 'NONE', *, *, #54714, .T. ) ;
#19150 = FACE_OUTER_BOUND ( 'NONE', #13250, .T. ) ;
#19151 = FACE_OUTER_BOUND ( 'NONE', #28678, .T. ) ;
#19152 = CARTESIAN_POINT ( 'NONE',  ( -20.42931928434034461, 20.86340285770621961, -4.315541546191446365 ) ) ;
#19153 = VERTEX_POINT ( 'NONE', #389 ) ;
#19154 = CARTESIAN_POINT ( 'NONE',  ( -14.64844551421497876, -5.213152330870663320, 10.92755654284354883 ) ) ;
#19155 = VERTEX_POINT ( 'NONE', #39607 ) ;
#19156 = CARTESIAN_POINT ( 'NONE',  ( -22.04727804374295275, 19.65758491770980143, 4.422150965879553475 ) ) ;
#19157 = EDGE_CURVE ( 'NONE', #17736, #33305, #48675, .T. ) ;
#19158 = EDGE_CURVE ( 'NONE', #6150, #56189, #35598, .T. ) ;
#19159 = PLANE ( 'NONE',  #48382 ) ;
#19160 = ORIENTED_EDGE ( 'NONE', *, *, #34088, .F. ) ;
#19161 = VECTOR ( 'NONE', #39187, 1000.000000000000227 ) ;
#19162 = AXIS2_PLACEMENT_3D ( 'NONE', #8751, #17520, #26068 ) ;
#19163 = DIRECTION ( 'NONE',  ( 0.007781995580012663651, 0.000000000000000000, -0.9999697198139515519 ) ) ;
#19164 = VERTEX_POINT ( 'NONE', #31350 ) ;
#19165 = EDGE_CURVE ( 'NONE', #49975, #6581, #11712, .T. ) ;
#19166 = EDGE_LOOP ( 'NONE', ( #53513, #16260, #31066, #50481 ) ) ;
#19167 = ORIENTED_EDGE ( 'NONE', *, *, #29686, .F. ) ;
#19168 = CARTESIAN_POINT ( 'NONE',  ( -29.13153550921558121, 15.83917597772816244, 4.729727457563339676 ) ) ;
#19169 = ORIENTED_EDGE ( 'NONE', *, *, #24229, .F. ) ;
#19170 = VERTEX_POINT ( 'NONE', #2884 ) ;
#19171 = DIRECTION ( 'NONE',  ( 0.000000000000000000, -0.000000000000000000, -1.000000000000000000 ) ) ;
#19172 = DIRECTION ( 'NONE',  ( 0.007781995580012662783, 0.000000000000000000, -0.9999697198139514409 ) ) ;
#19173 = ORIENTED_EDGE ( 'NONE', *, *, #41113, .F. ) ;
#19174 = ORIENTED_EDGE ( 'NONE', *, *, #8336, .F. ) ;
#19175 = CARTESIAN_POINT ( 'NONE',  ( -12.15116108492864377, 0.000000000000000000, 1.401855352044617975 ) ) ;
#19176 = EDGE_CURVE ( 'NONE', #47771, #22086, #41792, .T. ) ;
#19177 = EDGE_LOOP ( 'NONE', ( #10717, #55281, #26306, #40630, #18403, #39406, #989 ) ) ;
#19178 = VERTEX_POINT ( 'NONE', #49511 ) ;
#19179 = VECTOR ( 'NONE', #39154, 1000.000000000000227 ) ;
#19180 = EDGE_CURVE ( 'NONE', #9180, #21025, #27939, .T. ) ;
#19181 = DIRECTION ( 'NONE',  ( -0.9999697198139514409, -0.000000000000000000, -0.007781995580013368816 ) ) ;
#19182 = DIRECTION ( 'NONE',  ( -0.6427681459581293666, -0.7660444431189770143, -0.005002170337467561935 ) ) ;
#19183 = CARTESIAN_POINT ( 'NONE',  ( -9.741057028429843001, 0.000000000000000000, 2.159275478707846307 ) ) ;
#19184 = FACE_OUTER_BOUND ( 'NONE', #38582, .T. ) ;
#19185 = EDGE_LOOP ( 'NONE', ( #17095, #32952, #2122, #12748 ) ) ;
#19186 = FACE_OUTER_BOUND ( 'NONE', #8664, .T. ) ;
#19187 = VERTEX_POINT ( 'NONE', #36725 ) ;
#19188 = EDGE_CURVE ( 'NONE', #33148, #39021, #41259, .T. ) ;
#19189 = DIRECTION ( 'NONE',  ( -0.005961354470445682716, -0.6427876096865404731, 0.7660212471507180654 ) ) ;
#19190 = PLANE ( 'NONE',  #43308 ) ;
#19191 = CARTESIAN_POINT ( 'NONE',  ( -17.73140113748535285, 0.000000000000000000, 13.85752530597602039 ) ) ;
#19192 = CARTESIAN_POINT ( 'NONE',  ( -20.54204810873173415, 0.000000000000000000, 4.860550213503115558 ) ) ;
#19193 = CARTESIAN_POINT ( 'NONE',  ( -11.75708623541733289, -0.1941918491731566832, 1.441976946652226976 ) ) ;
#19194 = CARTESIAN_POINT ( 'NONE',  ( -10.47421230394850866, 0.000000000000000000, 10.95934586908605723 ) ) ;
#19195 = EDGE_LOOP ( 'NONE', ( #8383, #2272, #2555, #44851 ) ) ;
#19196 = CARTESIAN_POINT ( 'NONE',  ( -18.12176549260108160, 0.000000000000000000, 4.310047286430262581 ) ) ;
#19197 = VERTEX_POINT ( 'NONE', #19104 ) ;
#19198 = AXIS2_PLACEMENT_3D ( 'NONE', #27195, #49877, #10732 ) ;
#19199 = VECTOR ( 'NONE', #50345, 999.9999999999998863 ) ;
#19200 = CARTESIAN_POINT ( 'NONE',  ( -19.60912206198628027, -0.1191753592594197858, 4.398475361799976113 ) ) ;
#19201 = CARTESIAN_POINT ( 'NONE',  ( -22.40478740399063895, 0.000000000000000000, 5.384712028983816623 ) ) ;
#19202 = CARTESIAN_POINT ( 'NONE',  ( -15.13495153988577968, 0.000000000000000000, 12.76973526769478084 ) ) ;
#19203 = DIRECTION ( 'NONE',  ( -0.9999697198139514409, -0.000000000000000000, -0.007781995580013368816 ) ) ;
#19204 = CARTESIAN_POINT ( 'NONE',  ( -14.90379585677687224, 0.000000000000000000, 8.767075107899501063 ) ) ;
#19205 = LINE ( 'NONE', #39961, #19359 ) ;
#19206 = VECTOR ( 'NONE', #25191, 1000.000000000000000 ) ;
#19207 = VERTEX_POINT ( 'NONE', #10628 ) ;
#19208 = DIRECTION ( 'NONE',  ( 0.007781995580012663651, 0.000000000000000000, -0.9999697198139515519 ) ) ;
#19209 = PLANE ( 'NONE',  #26721 ) ;
#19210 = CARTESIAN_POINT ( 'NONE',  ( -18.67775241435682432, 0.000000000000000000, 4.136394454059623804 ) ) ;
#19211 = EDGE_CURVE ( 'NONE', #41396, #55875, #15156, .T. ) ;
#19212 = CARTESIAN_POINT ( 'NONE',  ( -69.85990692124715906, 0.6786957477238007019, -7.498719848001561772 ) ) ;
#19213 = AXIS2_PLACEMENT_3D ( 'NONE', #37140, #14721, #6479 ) ;
#19214 = CARTESIAN_POINT ( 'NONE',  ( -19.22961988024793101, -0.1191753592594177458, 14.39986392600063603 ) ) ;
#19215 = EDGE_CURVE ( 'NONE', #21025, #30222, #50330, .T. ) ;
#19216 = DIRECTION ( 'NONE',  ( -0.6427681459581293666, -0.7660444431189770143, -0.005002170337467561935 ) ) ;
#19217 = DIRECTION ( 'NONE',  ( -0.7660212471507179544, -0.6427876096865405842, -0.005961354470445141482 ) ) ;
#19218 = VECTOR ( 'NONE', #10878, 1000.000000000000227 ) ;
#19219 = CARTESIAN_POINT ( 'NONE',  ( -27.06708303904391144, 0.000000000000000000, 7.395095371555332697 ) ) ;
#19220 = ADVANCED_FACE ( 'NONE', ( #54563 ), #10872, .F. ) ;
#19221 = DIRECTION ( 'NONE',  ( 0.8531650599175527594, 0.4028455766673922356, -0.3313982828793700652 ) ) ;
#19222 = ORIENTED_EDGE ( 'NONE', *, *, #16613, .T. ) ;
#19223 = EDGE_CURVE ( 'NONE', #883, #3308, #2351, .T. ) ;
#19224 = ADVANCED_FACE ( 'NONE', ( #32475 ), #11445, .F. ) ;
#19225 = EDGE_CURVE ( 'NONE', #34036, #13341, #41538, .T. ) ;
#19226 = VERTEX_POINT ( 'NONE', #50617 ) ;
#19227 = EDGE_CURVE ( 'NONE', #26641, #49112, #20214, .T. ) ;
#19228 = ORIENTED_EDGE ( 'NONE', *, *, #35542, .F. ) ;
#19229 = ORIENTED_EDGE ( 'NONE', *, *, #10474, .F. ) ;
#19230 = ORIENTED_EDGE ( 'NONE', *, *, #43039, .F. ) ;
#19231 = ORIENTED_EDGE ( 'NONE', *, *, #11071, .F. ) ;
#19232 = AXIS2_PLACEMENT_3D ( 'NONE', #56170, #51357, #30879 ) ;
#19233 = LINE ( 'NONE', #5621, #47767 ) ;
#19234 = DIRECTION ( 'NONE',  ( 0.9999697198139515519, 0.000000000000000000, 0.007781995580013368816 ) ) ;
#19235 = VECTOR ( 'NONE', #43288, 1000.000000000000114 ) ;
#19236 = VECTOR ( 'NONE', #47409, 1000.000000000000227 ) ;
#19237 = ORIENTED_EDGE ( 'NONE', *, *, #45793, .T. ) ;
#19238 = ORIENTED_EDGE ( 'NONE', *, *, #36471, .T. ) ;
#19239 = EDGE_CURVE ( 'NONE', #695, #29014, #50027, .T. ) ;
#19240 = ORIENTED_EDGE ( 'NONE', *, *, #39120, .T. ) ;
#19241 = EDGE_CURVE ( 'NONE', #27276, #23644, #7180, .T. ) ;
#19242 = VECTOR ( 'NONE', #19221, 999.9999999999998863 ) ;
#19243 = VECTOR ( 'NONE', #24704, 999.9999999999998863 ) ;
#19244 = DIRECTION ( 'NONE',  ( 0.6427681459581294776, -0.7660444431189769032, 0.005002170337467562802 ) ) ;
#19245 = EDGE_CURVE ( 'NONE', #26740, #9909, #33314, .T. ) ;
#19246 = LINE ( 'NONE', #2746, #35563 ) ;
#19247 = CARTESIAN_POINT ( 'NONE',  ( -13.57512723388990850, 4.333955019861511992, 1.816696306515934278 ) ) ;
#19248 = EDGE_LOOP ( 'NONE', ( #21802, #34196, #31399, #4013 ) ) ;
#19249 = DIRECTION ( 'NONE',  ( 0.9999697198139515519, 0.000000000000000000, 0.007781995580013368816 ) ) ;
#19250 = ORIENTED_EDGE ( 'NONE', *, *, #45178, .F. ) ;
#19251 = ADVANCED_FACE ( 'NONE', ( #54870 ), #6912, .F. ) ;
#19252 = CARTESIAN_POINT ( 'NONE',  ( -26.13337879274045505, 0.000000000000000000, 6.833023547870798353 ) ) ;
#19253 = PLANE ( 'NONE',  #15735 ) ;
#19254 = ADVANCED_FACE ( 'NONE', ( #15983 ), #37262, .F. ) ;
#19255 = CARTESIAN_POINT ( 'NONE',  ( -22.40478740399063895, 0.000000000000000000, 5.384712028983816623 ) ) ;
#19256 = DIRECTION ( 'NONE',  ( -0.005002170337468016433, -0.7660444431189770143, 0.6427681459581293666 ) ) ;
#19257 = DIRECTION ( 'NONE',  ( 0.007781995580012662783, 0.000000000000000000, -0.9999697198139514409 ) ) ;
#19258 = LINE ( 'NONE', #24630, #43774 ) ;
#19259 = FACE_OUTER_BOUND ( 'NONE', #25047, .T. ) ;
#19260 = DIRECTION ( 'NONE',  ( -0.9999697198139514409, -0.000000000000000000, -0.007781995580013368816 ) ) ;
#19261 = ORIENTED_EDGE ( 'NONE', *, *, #26133, .T. ) ;
#19262 = CARTESIAN_POINT ( 'NONE',  ( -21.76664711697825894, -4.889348428825664783, 5.180230242434543442 ) ) ;
#19263 = ORIENTED_EDGE ( 'NONE', *, *, #7547, .T. ) ;
#19264 = DIRECTION ( 'NONE',  ( 0.7660212471507180654, -0.6427876096865404731, 0.005961354470445141482 ) ) ;
#19265 = FACE_OUTER_BOUND ( 'NONE', #47043, .T. ) ;
#19266 = CARTESIAN_POINT ( 'NONE',  ( -11.63277560346829453, 0.000000000000000000, 6.407212511434006608 ) ) ;
#19267 = CARTESIAN_POINT ( 'NONE',  ( -22.40478740399063895, 0.000000000000000000, 5.384712028983816623 ) ) ;
#19268 = VECTOR ( 'NONE', #49683, 999.9999999999998863 ) ;
#19269 = PLANE ( 'NONE',  #49532 ) ;
#19270 = LINE ( 'NONE', #49679, #52167 ) ;
#19271 = DIRECTION ( 'NONE',  ( -0.5364919789714478471, 0.6444004775717705469, -0.5449076811759709926 ) ) ;
#19272 = LINE ( 'NONE', #40862, #2083 ) ;
#19273 = CARTESIAN_POINT ( 'NONE',  ( -13.93428531402074633, 0.000000000000000000, 3.603971085826818133 ) ) ;
#19274 = VECTOR ( 'NONE', #2329, 1000.000000000000227 ) ;
#19275 = CARTESIAN_POINT ( 'NONE',  ( -14.00280974873554030, 0.000000000000000000, 12.40921378708904044 ) ) ;
#19276 = LINE ( 'NONE', #6248, #14045 ) ;
#19277 = CARTESIAN_POINT ( 'NONE',  ( -69.96872419296560963, -1.000000000000000888, -7.341494710781372390 ) ) ;
#19278 = CARTESIAN_POINT ( 'NONE',  ( -4.360905869600901319, 1.733607939028554791E-14, 2.600000000000000089 ) ) ;
#19279 = CIRCLE ( 'NONE', #27436, 1.000000000000000222 ) ;
#19280 = VECTOR ( 'NONE', #28281, 1000.000000000000000 ) ;
#19281 = CARTESIAN_POINT ( 'NONE',  ( -18.81226281495249708, 0.000000000000000000, 7.628662304866128174 ) ) ;
#19282 = LINE ( 'NONE', #28095, #18479 ) ;
#19283 = DIRECTION ( 'NONE',  ( 0.005961354470445682716, -0.6427876096865404731, -0.7660212471507180654 ) ) ;
#19284 = CARTESIAN_POINT ( 'NONE',  ( -17.74404816805336793, 0.000000000000000000, 3.574322630375089460 ) ) ;
#19285 = EDGE_LOOP ( 'NONE', ( #16172, #19427, #37388, #25434 ) ) ;
#19286 = AXIS2_PLACEMENT_3D ( 'NONE', #48992, #2108, #14630 ) ;
#19287 = VECTOR ( 'NONE', #7324, 999.9999999999998863 ) ;
#19288 = VERTEX_POINT ( 'NONE', #40964 ) ;
#19289 = DIRECTION ( 'NONE',  ( -0.5449076811759708816, 0.6444004775717707689, 0.5364919789714475140 ) ) ;
#19290 = DIRECTION ( 'NONE',  ( 0.5449076811759707706, 0.6444004775717708799, -0.5364919789714476250 ) ) ;
#19291 = EDGE_CURVE ( 'NONE', #51712, #47765, #2050, .T. ) ;
#19292 = ADVANCED_FACE ( 'NONE', ( #44670 ), #14583, .F. ) ;
#19293 = ORIENTED_EDGE ( 'NONE', *, *, #44682, .T. ) ;
#19294 = PLANE ( 'NONE',  #9542 ) ;
#19295 = AXIS2_PLACEMENT_3D ( 'NONE', #19828, #15296, #15021 ) ;
#19296 = ORIENTED_EDGE ( 'NONE', *, *, #6060, .T. ) ;
#19297 = CARTESIAN_POINT ( 'NONE',  ( -12.80458192191714595, 0.000000000000000000, 11.86454056839041726 ) ) ;
#19298 = EDGE_CURVE ( 'NONE', #36530, #50929, #19389, .T. ) ;
#19299 = VECTOR ( 'NONE', #22045, 1000.000000000000227 ) ;
#19300 = ORIENTED_EDGE ( 'NONE', *, *, #6742, .F. ) ;
#19301 = ORIENTED_EDGE ( 'NONE', *, *, #38882, .T. ) ;
#19302 = ORIENTED_EDGE ( 'NONE', *, *, #30894, .T. ) ;
#19303 = LINE ( 'NONE', #41173, #11184 ) ;
#19304 = DIRECTION ( 'NONE',  ( 0.007781995580012663651, 0.000000000000000000, -0.9999697198139515519 ) ) ;
#19305 = CARTESIAN_POINT ( 'NONE',  ( -13.53223678178913936, 2.067327705546508021, 1.872353476777575798 ) ) ;
#19306 = VECTOR ( 'NONE', #25471, 1000.000000000000227 ) ;
#19307 = ORIENTED_EDGE ( 'NONE', *, *, #53485, .T. ) ;
#19308 = ORIENTED_EDGE ( 'NONE', *, *, #1486, .T. ) ;
#19309 = VECTOR ( 'NONE', #46585, 999.9999999999998863 ) ;
#19310 = CARTESIAN_POINT ( 'NONE',  ( -20.49857661154221589, 0.1903768112243051092, 4.870464582990948088 ) ) ;
#19311 = ORIENTED_EDGE ( 'NONE', *, *, #37806, .F. ) ;
#19312 = VECTOR ( 'NONE', #48010, 1000.000000000000000 ) ;
#19313 = CARTESIAN_POINT ( 'NONE',  ( -26.25138199253913385, 17.50203338588876179, 4.621929860192643069 ) ) ;
#19314 = ORIENTED_EDGE ( 'NONE', *, *, #35156, .F. ) ;
#19315 = LINE ( 'NONE', #15345, #25805 ) ;
#19316 = CARTESIAN_POINT ( 'NONE',  ( 4.866417447938704122, 0.000000000000000000, 1.967953638241001002 ) ) ;
#19317 = AXIS2_PLACEMENT_3D ( 'NONE', #7031, #24332, #17204 ) ;
#19318 = VECTOR ( 'NONE', #8964, 999.9999999999998863 ) ;
#19319 = ORIENTED_EDGE ( 'NONE', *, *, #4194, .T. ) ;
#19320 = CARTESIAN_POINT ( 'NONE',  ( 2.072287782118878319, 0.000000000000000000, -2.950529333540147015 ) ) ;
#19321 = EDGE_CURVE ( 'NONE', #50536, #25204, #27652, .T. ) ;
#19322 = VECTOR ( 'NONE', #38034, 999.9999999999998863 ) ;
#19323 = CARTESIAN_POINT ( 'NONE',  ( -17.27030106973081303, -3.917936722690659401, 9.820304807591645258 ) ) ;
#19324 = VECTOR ( 'NONE', #35295, 1000.000000000000227 ) ;
#19326 = ADVANCED_FACE ( 'NONE', ( #49516 ), #9790, .F. ) ;
#19325 = ORIENTED_EDGE ( 'NONE', *, *, #16683, .F. ) ;
#19327 = PLANE ( 'NONE',  #41245 ) ;
#19328 = CARTESIAN_POINT ( 'NONE',  ( -16.63391944153825008, 2.391131607591507446, 7.266754650224643619 ) ) ;
#19329 = DIRECTION ( 'NONE',  ( 0.007781995580012663651, -3.146120232559066537E-19, -0.9999697198139514409 ) ) ;
#19330 = ADVANCED_FACE ( 'NONE', ( #27944 ), #1783, .F. ) ;
#19331 = ORIENTED_EDGE ( 'NONE', *, *, #9046, .F. ) ;
#19332 = LINE ( 'NONE', #11665, #39193 ) ;
#19333 = FACE_OUTER_BOUND ( 'NONE', #4610, .T. ) ;
#19334 = EDGE_CURVE ( 'NONE', #44511, #7820, #23397, .T. ) ;
#19335 = LINE ( 'NONE', #49457, #5878 ) ;
#19336 = DIRECTION ( 'NONE',  ( 0.5449076811759707706, 0.6444004775717708799, -0.5364919789714476250 ) ) ;
#19337 = AXIS2_PLACEMENT_3D ( 'NONE', #17223, #9259, #30598 ) ;
#19338 = DIRECTION ( 'NONE',  ( -0.005961354470445682716, -0.6427876096865404731, 0.7660212471507180654 ) ) ;
#19339 = CARTESIAN_POINT ( 'NONE',  ( -20.54204810873173415, 0.000000000000000000, 4.860550213503115558 ) ) ;
#19340 = CARTESIAN_POINT ( 'NONE',  ( -66.44695135234023553, -11.32745730419861374, -0.6963329337552829346 ) ) ;
#19341 = ORIENTED_EDGE ( 'NONE', *, *, #42694, .T. ) ;
#19342 = CARTESIAN_POINT ( 'NONE',  ( -14.53990499995960306, -0.1191753592594190225, 8.866166454900344718 ) ) ;
#19343 = CARTESIAN_POINT ( 'NONE',  ( -24.26986129792355129, -0.1191753592594197858, 6.208864760408702388 ) ) ;
#19344 = CARTESIAN_POINT ( 'NONE',  ( -66.47616155185831133, 5.898059818321144121E-14, 4.837977870783337409 ) ) ;
#19345 = ORIENTED_EDGE ( 'NONE', *, *, #50994, .F. ) ;
#19346 = CARTESIAN_POINT ( 'NONE',  ( -30.79567442779373110, 0.000000000000000000, 8.843406890442315316 ) ) ;
#19347 = LINE ( 'NONE', #40676, #8205 ) ;
#19348 = AXIS2_PLACEMENT_3D ( 'NONE', #2359, #19692, #45247 ) ;
#19349 = FACE_OUTER_BOUND ( 'NONE', #20421, .T. ) ;
#19350 = VECTOR ( 'NONE', #29005, 999.9999999999998863 ) ;
#19351 = LINE ( 'NONE', #18826, #26048 ) ;
#19352 = CARTESIAN_POINT ( 'NONE',  ( -55.84725198092744591, 6.793269954351565332, 1.721684726214605998 ) ) ;
#19353 = ORIENTED_EDGE ( 'NONE', *, *, #28804, .F. ) ;
#19354 = EDGE_LOOP ( 'NONE', ( #9099, #9474, #11951, #32787 ) ) ;
#19355 = CARTESIAN_POINT ( 'NONE',  ( -18.78077679739165973, 4.981562823951513508, 3.818085302033760620 ) ) ;
#19356 = VECTOR ( 'NONE', #20582, 999.9999999999998863 ) ;
#19357 = STYLED_ITEM ( 'NONE', ( #50343 ), #41257 ) ;
#19358 = DIRECTION ( 'NONE',  ( 0.5364919789714477361, 0.6444004775717706579, 0.5449076811759711036 ) ) ;
#19359 = VECTOR ( 'NONE', #1046, 999.9999999999998863 ) ;
#19360 = EDGE_CURVE ( 'NONE', #28890, #1495, #18860, .T. ) ;
#19361 = EDGE_LOOP ( 'NONE', ( #53813, #26114, #35235, #19936 ) ) ;
#19362 = CARTESIAN_POINT ( 'NONE',  ( -69.43561177275644525, -9.791245164465275153, -7.501782499249458169 ) ) ;
#19363 = EDGE_LOOP ( 'NONE', ( #27387, #3327, #6591, #2740 ) ) ;
#19364 = DIRECTION ( 'NONE',  ( -0.7051023234936394379, -0.7091055728196409280, 0.000000000000000000 ) ) ;
#19365 = EDGE_CURVE ( 'NONE', #17633, #24207, #23932, .T. ) ;
#19366 = ADVANCED_FACE ( 'NONE', ( #41263 ), #6346, .F. ) ;
#19367 = VECTOR ( 'NONE', #18920, 1000.000000000000000 ) ;
#19368 = ORIENTED_EDGE ( 'NONE', *, *, #17873, .T. ) ;
#19369 = AXIS2_PLACEMENT_3D ( 'NONE', #40554, #10445, #40248 ) ;
#19370 = VERTEX_POINT ( 'NONE', #31642 ) ;
#19371 = CARTESIAN_POINT ( 'NONE',  ( -14.60334660744590174, 0.000000000000000000, 4.168102422163359577 ) ) ;
#19372 = DIRECTION ( 'NONE',  ( -0.005961354470445682716, -0.6427876096865404731, 0.7660212471507180654 ) ) ;
#19373 = CARTESIAN_POINT ( 'NONE',  ( -12.88979734264706067, -3.756034771668162797, 1.768318970208784924 ) ) ;
#19374 = VERTEX_POINT ( 'NONE', #1531 ) ;
#19375 = LINE ( 'NONE', #37250, #7508 ) ;
#19376 = ORIENTED_EDGE ( 'NONE', *, *, #31549, .T. ) ;
#19377 = ADVANCED_FACE ( 'NONE', ( #54046 ), #36730, .F. ) ;
#19378 = VERTEX_POINT ( 'NONE', #32479 ) ;
#19379 = EDGE_LOOP ( 'NONE', ( #27859, #41110, #24400, #43619, #7884 ) ) ;
#19380 = DIRECTION ( 'NONE',  ( 0.6427681459581294776, -0.7660444431189769032, 0.005002170337467562802 ) ) ;
#19381 = VECTOR ( 'NONE', #10870, 999.9999999999998863 ) ;
#19382 = ORIENTED_EDGE ( 'NONE', *, *, #3078, .F. ) ;
#19383 = DIRECTION ( 'NONE',  ( 0.005961354470445682716, -0.6427876096865404731, -0.7660212471507180654 ) ) ;
#19384 = EDGE_LOOP ( 'NONE', ( #52690, #43734, #49584, #9435 ) ) ;
#19385 = VECTOR ( 'NONE', #44765, 1000.000000000000227 ) ;
#19386 = CARTESIAN_POINT ( 'NONE',  ( -10.00813838035478298, 0.000000000000000000, 10.77830692922518452 ) ) ;
#19387 = LINE ( 'NONE', #19942, #29512 ) ;
#19388 = ORIENTED_EDGE ( 'NONE', *, *, #30289, .F. ) ;
#19389 = LINE ( 'NONE', #40712, #20413 ) ;
#19390 = VECTOR ( 'NONE', #55094, 1000.000000000000000 ) ;
#19391 = VERTEX_POINT ( 'NONE', #32192 ) ;
#19392 = FACE_OUTER_BOUND ( 'NONE', #1804, .T. ) ;
#19393 = CARTESIAN_POINT ( 'NONE',  ( -24.26908309836554878, 0.000000000000000000, 6.108867788427308376 ) ) ;
#19394 = LINE ( 'NONE', #2629, #40461 ) ;
#19395 = CARTESIAN_POINT ( 'NONE',  ( -24.26908309836554878, 0.000000000000000000, 6.108867788427308376 ) ) ;
#19396 = FACE_OUTER_BOUND ( 'NONE', #27267, .T. ) ;
#19397 = VECTOR ( 'NONE', #23382, 1000.000000000000227 ) ;
#19398 = LINE ( 'NONE', #30861, #29167 ) ;
#19399 = DIRECTION ( 'NONE',  ( 0.5364919789714477361, 0.6444004775717706579, 0.5449076811759711036 ) ) ;
#19400 = ORIENTED_EDGE ( 'NONE', *, *, #43951, .T. ) ;
#19401 = VERTEX_POINT ( 'NONE', #35909 ) ;
#19402 = CARTESIAN_POINT ( 'NONE',  ( -18.39746900504187010, 0.000000000000000000, 14.03700784672088808 ) ) ;
#19403 = EDGE_CURVE ( 'NONE', #31783, #5918, #32274, .T. ) ;
#19404 = CARTESIAN_POINT ( 'NONE',  ( -11.30636317915456779, -0.1191753592594197858, 11.32220194836580340 ) ) ;
#19405 = LINE ( 'NONE', #39692, #30325 ) ;
#19406 = CARTESIAN_POINT ( 'NONE',  ( -13.73672976910459909, 0.000000000000000000, 12.22661844811216270 ) ) ;
#19407 = AXIS2_PLACEMENT_3D ( 'NONE', #37369, #15261, #28038 ) ;
#19408 = VECTOR ( 'NONE', #4696, 999.9999999999998863 ) ;
#19409 = PLANE ( 'NONE',  #49406 ) ;
#19410 = ORIENTED_EDGE ( 'NONE', *, *, #33046, .T. ) ;
#19411 = PLANE ( 'NONE',  #39499 ) ;
#19412 = CARTESIAN_POINT ( 'NONE',  ( 2.072287782118878319, 0.000000000000000000, -2.950529333540147015 ) ) ;
#19413 = ORIENTED_EDGE ( 'NONE', *, *, #10469, .T. ) ;
#19414 = CARTESIAN_POINT ( 'NONE',  ( -29.86197018149027116, 0.000000000000000000, 8.281335066757780083 ) ) ;
#19415 = CARTESIAN_POINT ( 'NONE',  ( -4.360905869600901319, 1.733607939028554791E-14, 2.600000000000000089 ) ) ;
#19416 = EDGE_LOOP ( 'NONE', ( #24743, #23012, #17982, #49313 ) ) ;
#19417 = EDGE_CURVE ( 'NONE', #14383, #28433, #45498, .T. ) ;
#19418 = DIRECTION ( 'NONE',  ( 0.005002170337468016433, -0.7660444431189770143, -0.6427681459581293666 ) ) ;
#19419 = CARTESIAN_POINT ( 'NONE',  ( -15.08654547970796500, 0.000000000000000000, 6.549660489236909910 ) ) ;
#19420 = CARTESIAN_POINT ( 'NONE',  ( -16.56378919472086864, -4.727446477803161073, 10.87441502184582909 ) ) ;
#19421 = EDGE_CURVE ( 'NONE', #12571, #4309, #14028, .T. ) ;
#19422 = EDGE_CURVE ( 'NONE', #3167, #2376, #27094, .T. ) ;
#19423 = CARTESIAN_POINT ( 'NONE',  ( -21.74939387271512103, 3.524445264749011208, 5.017686667736141359 ) ) ;
#19424 = LINE ( 'NONE', #36766, #52787 ) ;
#19425 = VECTOR ( 'NONE', #44216, 1000.000000000000000 ) ;
#19426 = ORIENTED_EDGE ( 'NONE', *, *, #26045, .T. ) ;
#19427 = ORIENTED_EDGE ( 'NONE', *, *, #43307, .T. ) ;
#19428 = DIRECTION ( 'NONE',  ( -0.005002170337468016433, -0.7660444431189770143, 0.6427681459581293666 ) ) ;
#19429 = LINE ( 'NONE', #41305, #3212 ) ;
#19430 = DIRECTION ( 'NONE',  ( 0.8531650599175527594, 0.4028455766673922356, -0.3313982828793700652 ) ) ;
#19431 = ADVANCED_FACE ( 'NONE', ( #22819 ), #40137, .F. ) ;
#19432 = VECTOR ( 'NONE', #31655, 1000.000000000000227 ) ;
#19433 = CARTESIAN_POINT ( 'NONE',  ( -13.31717279592726833, 1.257817950434005683, 1.814642920502075540 ) ) ;
#19434 = EDGE_CURVE ( 'NONE', #54860, #6825, #33854, .T. ) ;
#19435 = DIRECTION ( 'NONE',  ( 0.007781995580012663651, -3.146120232559066537E-19, -0.9999697198139514409 ) ) ;
#19436 = ORIENTED_EDGE ( 'NONE', *, *, #41783, .F. ) ;
#19437 = CARTESIAN_POINT ( 'NONE',  ( 5.343330229674628562, -1.064751996674356826, -2.421220660758175658 ) ) ;
#19438 = EDGE_CURVE ( 'NONE', #20292, #3728, #20792, .T. ) ;
#19439 = LINE ( 'NONE', #41584, #21431 ) ;
#19440 = LINE ( 'NONE', #45549, #19649 ) ;
#19441 = ORIENTED_EDGE ( 'NONE', *, *, #32016, .F. ) ;
#19442 = VECTOR ( 'NONE', #38303, 1000.000000000000000 ) ;
#19443 = ADVANCED_FACE ( 'NONE', ( #8030 ), #19944, .F. ) ;
#19444 = CARTESIAN_POINT ( 'NONE',  ( -13.08486533123210194, 0.000000000000000000, 1.963927175729152541 ) ) ;
#19445 = VERTEX_POINT ( 'NONE', #37013 ) ;
#19446 = CARTESIAN_POINT ( 'NONE',  ( -25.20278734466900517, 0.000000000000000000, 6.670939612111840944 ) ) ;
#19447 = CARTESIAN_POINT ( 'NONE',  ( -8.975993561185934055, -0.1191753592594197858, 10.41700724906143982 ) ) ;
#19448 = AXIS2_PLACEMENT_3D ( 'NONE', #51489, #51192, #12584 ) ;
#19449 = EDGE_CURVE ( 'NONE', #28956, #18999, #33569, .T. ) ;
#19450 = VERTEX_POINT ( 'NONE', #19688 ) ;
#19451 = DIRECTION ( 'NONE',  ( -0.005002170337468016433, -0.7660444431189770143, 0.6427681459581293666 ) ) ;
#19452 = ORIENTED_EDGE ( 'NONE', *, *, #27797, .F. ) ;
#19453 = ADVANCED_FACE ( 'NONE', ( #46928 ), #32723, .F. ) ;
#19454 = VECTOR ( 'NONE', #11115, 1000.000000000000114 ) ;
#19455 = ORIENTED_EDGE ( 'NONE', *, *, #37314, .T. ) ;
#19456 = ORIENTED_EDGE ( 'NONE', *, *, #50697, .T. ) ;
#19457 = DIRECTION ( 'NONE',  ( 0.005002170337468016433, -0.7660444431189770143, -0.6427681459581293666 ) ) ;
#19458 = AXIS2_PLACEMENT_3D ( 'NONE', #12738, #25806, #43132 ) ;
#19459 = EDGE_LOOP ( 'NONE', ( #16735, #9743, #15670, #40894 ) ) ;
#19460 = ORIENTED_EDGE ( 'NONE', *, *, #48211, .T. ) ;
#19461 = LINE ( 'NONE', #36801, #8442 ) ;
#19462 = ORIENTED_EDGE ( 'NONE', *, *, #21354, .F. ) ;
#19463 = ORIENTED_EDGE ( 'NONE', *, *, #12440, .T. ) ;
#19464 = DIRECTION ( 'NONE',  ( 0.5364919789714477361, 0.6444004775717706579, 0.5449076811759711036 ) ) ;
#19465 = ORIENTED_EDGE ( 'NONE', *, *, #33874, .T. ) ;
#19466 = ORIENTED_EDGE ( 'NONE', *, *, #27649, .F. ) ;
#19467 = ORIENTED_EDGE ( 'NONE', *, *, #12255, .F. ) ;
#19468 = AXIS2_PLACEMENT_3D ( 'NONE', #18683, #50148, #15503 ) ;
#19469 = CARTESIAN_POINT ( 'NONE',  ( -10.37421533196711465, -0.1191753592594197858, 10.96012406864405975 ) ) ;
#19470 = VECTOR ( 'NONE', #38961, 999.9999999999998863 ) ;
#19471 = CARTESIAN_POINT ( 'NONE',  ( -18.65135909430610539, 0.9340140483890049250, 5.659018568344508893 ) ) ;
#19472 = CARTESIAN_POINT ( 'NONE',  ( -23.66772770479517618, 18.99370688441070953, -4.657437592157546824 ) ) ;
#19473 = FACE_OUTER_BOUND ( 'NONE', #31409, .T. ) ;
#19474 = ORIENTED_EDGE ( 'NONE', *, *, #314, .F. ) ;
#19475 = LINE ( 'NONE', #1611, #36492 ) ;
#19476 = AXIS2_PLACEMENT_3D ( 'NONE', #35016, #43504, #20805 ) ;
#19477 = EDGE_LOOP ( 'NONE', ( #23387, #30662, #49194, #21632 ) ) ;
#19478 = ORIENTED_EDGE ( 'NONE', *, *, #50317, .T. ) ;
#19479 = ADVANCED_FACE ( 'NONE', ( #37266 ), #45791, .F. ) ;
#19480 = DIRECTION ( 'NONE',  ( -0.02128905125521653521, -0.002441305003918738115, 0.9997703818010066357 ) ) ;
#19481 = VECTOR ( 'NONE', #23867, 999.9999999999998863 ) ;
#19482 = CARTESIAN_POINT ( 'NONE',  ( -30.26074760107038131, 15.18722507252361709, -4.766914839722605102 ) ) ;
#19483 = VECTOR ( 'NONE', #33011, 1000.000000000000114 ) ;
#19484 = VECTOR ( 'NONE', #41559, 999.9999999999998863 ) ;
#19485 = CARTESIAN_POINT ( 'NONE',  ( -13.26502572267249391, -3.594132820645661308, 7.733102475169945755 ) ) ;
#19486 = DIRECTION ( 'NONE',  ( -0.6427681459581293666, -0.7660444431189770143, -0.005002170337467561935 ) ) ;
#19487 = VECTOR ( 'NONE', #47900, 1000.000000000000227 ) ;
#19488 = LINE ( 'NONE', #41882, #35874 ) ;
#19489 = VERTEX_POINT ( 'NONE', #16522 ) ;
#19490 = CARTESIAN_POINT ( 'NONE',  ( -15.40103151951671734, 0.000000000000000000, 12.95233060667165681 ) ) ;
#19491 = EDGE_LOOP ( 'NONE', ( #36657, #54653, #17114, #15146 ) ) ;
#19492 = VECTOR ( 'NONE', #13141, 1000.000000000000227 ) ;
#19493 = DIRECTION ( 'NONE',  ( -0.5449076811759708816, 0.6444004775717707689, 0.5364919789714475140 ) ) ;
#19494 = LINE ( 'NONE', #36839, #6934 ) ;
#19495 = LINE ( 'NONE', #54152, #8171 ) ;
#19496 = DIRECTION ( 'NONE',  ( 0.000000000000000000, 0.000000000000000000, 1.000000000000000000 ) ) ;
#19497 = ADVANCED_FACE ( 'NONE', ( #46077 ), #46629, .F. ) ;
#19498 = LINE ( 'NONE', #32569, #2344 ) ;
#19499 = AXIS2_PLACEMENT_3D ( 'NONE', #1762, #36699, #28439 ) ;
#19500 = AXIS2_PLACEMENT_3D ( 'NONE', #9217, #13216, #26532 ) ;
#19501 = EDGE_LOOP ( 'NONE', ( #17954, #41601, #35982, #6984 ) ) ;
#19502 = DIRECTION ( 'NONE',  ( 0.9999697198139515519, 0.000000000000000000, 0.007781995580013368816 ) ) ;
#19503 = DIRECTION ( 'NONE',  ( 0.9999697198139515519, 0.000000000000000000, 0.007781995580013368816 ) ) ;
#19504 = LINE ( 'NONE', #19210, #9776 ) ;
#19505 = FACE_OUTER_BOUND ( 'NONE', #6429, .T. ) ;
#19506 = ADVANCED_FACE ( 'NONE', ( #50877 ), #29623, .F. ) ;
#19507 = LINE ( 'NONE', #24330, #41180 ) ;
#19508 = CARTESIAN_POINT ( 'NONE',  ( -19.53160284976675598, 0.000000000000000000, 6.345742011377845770 ) ) ;
#19509 = CARTESIAN_POINT ( 'NONE',  ( -16.94509306707230678, 0.000000000000000000, 6.535196842164872955 ) ) ;
#19510 = ADVANCED_FACE ( 'NONE', ( #42644 ), #25342, .F. ) ;
#19511 = VECTOR ( 'NONE', #45283, 1000.000000000000000 ) ;
#19512 = CARTESIAN_POINT ( 'NONE',  ( -21.36215635309214989, 4.172053068839010947, 4.846608384923496438 ) ) ;
#19513 = VECTOR ( 'NONE', #28615, 1000.000000000000227 ) ;
#19514 = DIRECTION ( 'NONE',  ( 0.9999697198139515519, 0.000000000000000000, 0.007781995580013368816 ) ) ;
#19515 = VECTOR ( 'NONE', #23806, 1000.000000000000227 ) ;
#19516 = ADVANCED_FACE ( 'NONE', ( #7183 ), #2890, .F. ) ;
#19517 = ORIENTED_EDGE ( 'NONE', *, *, #22087, .F. ) ;
#19518 = VECTOR ( 'NONE', #32605, 1000.000000000000227 ) ;
#19519 = EDGE_CURVE ( 'NONE', #22811, #19054, #37854, .T. ) ;
#19520 = ORIENTED_EDGE ( 'NONE', *, *, #1067, .F. ) ;
#19521 = ORIENTED_EDGE ( 'NONE', *, *, #50258, .T. ) ;
#19522 = VECTOR ( 'NONE', #54875, 999.9999999999998863 ) ;
#19523 = VECTOR ( 'NONE', #15820, 999.9999999999998863 ) ;
#19524 = EDGE_LOOP ( 'NONE', ( #38049, #49960, #32034, #51627 ) ) ;
#19525 = VECTOR ( 'NONE', #28997, 999.9999999999998863 ) ;
#19526 = EDGE_LOOP ( 'NONE', ( #21972, #51590, #19714, #15061 ) ) ;
#19527 = LINE ( 'NONE', #49349, #26939 ) ;
#19528 = DIRECTION ( 'NONE',  ( 0.9999697198139515519, 0.000000000000000000, 0.007781995580013368816 ) ) ;
#19529 = VECTOR ( 'NONE', #54677, 999.9999999999998863 ) ;
#19530 = VECTOR ( 'NONE', #32471, 1000.000000000000114 ) ;
#19531 = ORIENTED_EDGE ( 'NONE', *, *, #21234, .T. ) ;
#19532 = LINE ( 'NONE', #12433, #47612 ) ;
#19533 = EDGE_LOOP ( 'NONE', ( #860, #35595, #48396, #42291 ) ) ;
#19534 = ORIENTED_EDGE ( 'NONE', *, *, #35962, .F. ) ;
#19535 = AXIS2_PLACEMENT_3D ( 'NONE', #19992, #49828, #2671 ) ;
#19536 = AXIS2_PLACEMENT_3D ( 'NONE', #22225, #30178, #16546 ) ;
#19537 = CARTESIAN_POINT ( 'NONE',  ( -67.89698098956576189, -8.875497699457834955, 5.577208301931539935 ) ) ;
#19538 = PLANE ( 'NONE',  #29189 ) ;
#19539 = CARTESIAN_POINT ( 'NONE',  ( -20.40437129806706196, -3.270328918600661439, 4.702731250161795273 ) ) ;
#19540 = ORIENTED_EDGE ( 'NONE', *, *, #19048, .F. ) ;
#19541 = DIRECTION ( 'NONE',  ( -0.9999697198139514409, -0.000000000000000000, -0.007781995580013368816 ) ) ;
#19542 = EDGE_CURVE ( 'NONE', #34361, #30915, #11977, .T. ) ;
#19543 = LINE ( 'NONE', #54190, #31859 ) ;
#19544 = ADVANCED_FACE ( 'NONE', ( #29031 ), #41542, .F. ) ;
#19545 = PLANE ( 'NONE',  #46580 ) ;
#19546 = VECTOR ( 'NONE', #1425, 1000.000000000000000 ) ;
#19547 = DIRECTION ( 'NONE',  ( -0.005961354470445682716, -0.6427876096865404731, 0.7660212471507180654 ) ) ;
#19548 = CARTESIAN_POINT ( 'NONE',  ( -12.22842013625588820, -0.03739765774599676518, 1.569878849409872545 ) ) ;
#19549 = EDGE_CURVE ( 'NONE', #52700, #45157, #24481, .T. ) ;
#19550 = CARTESIAN_POINT ( 'NONE',  ( -10.43885885690782800, 0.000000000000000000, 6.416503847622031742 ) ) ;
#19551 = DIRECTION ( 'NONE',  ( 0.6427681459581294776, -0.7660444431189769032, 0.005002170337467562802 ) ) ;
#19553 = VECTOR ( 'NONE', #42616, 1000.000000000000114 ) ;
#19552 = LINE ( 'NONE', #24364, #27609 ) ;
#19554 = EDGE_CURVE ( 'NONE', #29102, #38297, #41795, .T. ) ;
#19555 = PLANE ( 'NONE',  #39274 ) ;
#19556 = ORIENTED_EDGE ( 'NONE', *, *, #17277, .T. ) ;
#19557 = PLANE ( 'NONE',  #22940 ) ;
#19558 = VERTEX_POINT ( 'NONE', #21063 ) ;
#19559 = VECTOR ( 'NONE', #28498, 1000.000000000000227 ) ;
#19560 = EDGE_CURVE ( 'NONE', #29459, #19401, #21653, .T. ) ;
#19561 = EDGE_CURVE ( 'NONE', #36795, #45113, #30446, .T. ) ;
#19562 = ADVANCED_FACE ( 'NONE', ( #12569 ), #26441, .F. ) ;
#19563 = CARTESIAN_POINT ( 'NONE',  ( -31.72704407542318350, -0.1191753592594197858, 9.105487798182664960 ) ) ;
#19564 = LINE ( 'NONE', #37156, #55898 ) ;
#19565 = PLANE ( 'NONE',  #22242 ) ;
#19566 = PLANE ( 'NONE',  #22346 ) ;
#19567 = AXIS2_PLACEMENT_3D ( 'NONE', #2299, #37213, #11668 ) ;
#19568 = DIRECTION ( 'NONE',  ( 0.6246952433987894571, -0.7422098413412800966, -0.2426528472758541777 ) ) ;
#19569 = CARTESIAN_POINT ( 'NONE',  ( -12.33850799832341849, 0.000000000000000000, 11.68350162852954632 ) ) ;
#19571 = VECTOR ( 'NONE', #55166, 1000.000000000000114 ) ;
#19570 = CARTESIAN_POINT ( 'NONE',  ( -10.74029228357944987, 0.000000000000000000, 11.14194120806293320 ) ) ;
#19572 = DIRECTION ( 'NONE',  ( 0.9953987247224346246, 0.05289437297717029807, 0.07989720976544260889 ) ) ;
#19573 = PLANE ( 'NONE',  #43749 ) ;
#19574 = CARTESIAN_POINT ( 'NONE',  ( -22.40478740399063895, 0.000000000000000000, 5.384712028983816623 ) ) ;
#19575 = CARTESIAN_POINT ( 'NONE',  ( -14.66887761629205222, 0.000000000000000000, 12.58869632783390990 ) ) ;
#19576 = CARTESIAN_POINT ( 'NONE',  ( -25.20123094555300369, 0.000000000000000000, 6.470945668149052032 ) ) ;
#19578 = AXIS2_PLACEMENT_3D ( 'NONE', #50712, #25177, #46738 ) ;
#19577 = DIRECTION ( 'NONE',  ( -0.9999697198139514409, -0.000000000000000000, -0.007781995580013368816 ) ) ;
#19579 = VECTOR ( 'NONE', #11292, 999.9999999999998863 ) ;
#19580 = FACE_OUTER_BOUND ( 'NONE', #50022, .T. ) ;
#19581 = EDGE_CURVE ( 'NONE', #31672, #49287, #52314, .T. ) ;
#19582 = VECTOR ( 'NONE', #47943, 999.9999999999998863 ) ;
#19583 = LINE ( 'NONE', #24654, #49338 ) ;
#19584 = PLANE ( 'NONE',  #52217 ) ;
#19585 = CARTESIAN_POINT ( 'NONE',  ( -20.10223246962251764, 1.178764073316398875, 5.890828872904841695 ) ) ;
#19586 = EDGE_LOOP ( 'NONE', ( #18182, #15063, #18342, #20060 ) ) ;
#19587 = VECTOR ( 'NONE', #451, 1000.000000000000114 ) ;
#19588 = EDGE_CURVE ( 'NONE', #49949, #19711, #51723, .T. ) ;
#19590 = CARTESIAN_POINT ( 'NONE',  ( -22.40478740399063895, 0.000000000000000000, 5.384712028983816623 ) ) ;
#19589 = VECTOR ( 'NONE', #43937, 1000.000000000000114 ) ;
#19591 = EDGE_LOOP ( 'NONE', ( #16239, #23943, #2113, #43606 ) ) ;
#19592 = ADVANCED_FACE ( 'NONE', ( #43760 ), #34419, .F. ) ;
#19593 = DIRECTION ( 'NONE',  ( -0.005961354470445682716, -0.6427876096865404731, 0.7660212471507180654 ) ) ;
#19594 = CARTESIAN_POINT ( 'NONE',  ( -9.859076521000934790, -0.1191753592594181482, 4.474352470677822602 ) ) ;
#19595 = EDGE_CURVE ( 'NONE', #31964, #26839, #38391, .T. ) ;
#19596 = ORIENTED_EDGE ( 'NONE', *, *, #54835, .T. ) ;
#19597 = DIRECTION ( 'NONE',  ( -0.5364919789714478471, 0.6444004775717705469, -0.5449076811759709926 ) ) ;
#19598 = ORIENTED_EDGE ( 'NONE', *, *, #28868, .T. ) ;
#19599 = FACE_OUTER_BOUND ( 'NONE', #17509, .T. ) ;
#19600 = VECTOR ( 'NONE', #55469, 1000.000000000000227 ) ;
#19601 = VERTEX_POINT ( 'NONE', #16827 ) ;
#19602 = ORIENTED_EDGE ( 'NONE', *, *, #21587, .T. ) ;
#19603 = ORIENTED_EDGE ( 'NONE', *, *, #7154, .T. ) ;
#19604 = LINE ( 'NONE', #10804, #54701 ) ;
#19605 = CARTESIAN_POINT ( 'NONE',  ( -16.31417959753190416, 4.819660872929012463, 2.865140703502121688 ) ) ;
#19606 = VECTOR ( 'NONE', #4363, 999.9999999999998863 ) ;
#19607 = CARTESIAN_POINT ( 'NONE',  ( -17.49802427868480947, 2.481410104826615282, 12.59520711516599256 ) ) ;
#19608 = ORIENTED_EDGE ( 'NONE', *, *, #48918, .F. ) ;
#19609 = AXIS2_PLACEMENT_3D ( 'NONE', #45140, #24374, #54457 ) ;
#19610 = ORIENTED_EDGE ( 'NONE', *, *, #49518, .F. ) ;
#19611 = AXIS2_PLACEMENT_3D ( 'NONE', #36070, #40602, #36601 ) ;
#19612 = VECTOR ( 'NONE', #18208, 1000.000000000000227 ) ;
#19613 = LINE ( 'NONE', #19310, #39079 ) ;
#19614 = ORIENTED_EDGE ( 'NONE', *, *, #12019, .T. ) ;
#19615 = DIRECTION ( 'NONE',  ( -0.7660212471507179544, -0.6427876096865405842, -0.005961354470445141482 ) ) ;
#19616 = ORIENTED_EDGE ( 'NONE', *, *, #51653, .T. ) ;
#19617 = FACE_OUTER_BOUND ( 'NONE', #4335, .T. ) ;
#19618 = LINE ( 'NONE', #45184, #41238 ) ;
#19619 = AXIS2_PLACEMENT_3D ( 'NONE', #14943, #49298, #18933 ) ;
#19620 = ORIENTED_EDGE ( 'NONE', *, *, #51028, .T. ) ;
#19621 = AXIS2_PLACEMENT_3D ( 'NONE', #35340, #22287, #21984 ) ;
#19622 = PLANE ( 'NONE',  #45828 ) ;
#19623 = CARTESIAN_POINT ( 'NONE',  ( -12.15271748404464880, 0.000000000000000000, 1.601849296007406664 ) ) ;
#19624 = AXIS2_PLACEMENT_3D ( 'NONE', #24802, #11180, #42122 ) ;
#19625 = EDGE_LOOP ( 'NONE', ( #40332, #24066, #48606, #6371 ) ) ;
#19626 = LINE ( 'NONE', #1988, #28560 ) ;
#19627 = CARTESIAN_POINT ( 'NONE',  ( -19.80206979258221622, -3.108426967578159950, 4.473942411073648984 ) ) ;
#19628 = DIRECTION ( 'NONE',  ( 0.6427681459581294776, -0.7660444431189769032, 0.005002170337467562802 ) ) ;
#19629 = ORIENTED_EDGE ( 'NONE', *, *, #27866, .T. ) ;
#19630 = EDGE_CURVE ( 'NONE', #18585, #13470, #52009, .T. ) ;
#19631 = ADVANCED_FACE ( 'NONE', ( #30734 ), #52570, .F. ) ;
#19632 = DIRECTION ( 'NONE',  ( 0.9999697198139515519, 0.000000000000000000, 0.007781995580013368816 ) ) ;
#19633 = PLANE ( 'NONE',  #17868 ) ;
#19634 = PLANE ( 'NONE',  #420 ) ;
#19635 = DIRECTION ( 'NONE',  ( 0.005961354470445682716, -0.6427876096865404731, -0.7660212471507180654 ) ) ;
#19636 = EDGE_CURVE ( 'NONE', #33095, #39543, #625, .T. ) ;
#19637 = CARTESIAN_POINT ( 'NONE',  ( -23.59415687586314547, 18.97399364021188717, 4.500635337789387513 ) ) ;
#19638 = LINE ( 'NONE', #37215, #44234 ) ;
#19639 = VECTOR ( 'NONE', #29837, 999.9999999999998863 ) ;
#19640 = CARTESIAN_POINT ( 'NONE',  ( -68.75440753303996644, -11.59206300474163065, 7.127210919649165533 ) ) ;
#19641 = ORIENTED_EDGE ( 'NONE', *, *, #20055, .F. ) ;
#19642 = LINE ( 'NONE', #7394, #55233 ) ;
#19643 = CARTESIAN_POINT ( 'NONE',  ( -9.542064456761055524, 0.000000000000000000, 10.59726798936431180 ) ) ;
#19644 = CARTESIAN_POINT ( 'NONE',  ( -66.43509620407327532, 1.406259945342289676E-11, 0.3563396980984065432 ) ) ;
#19645 = ORIENTED_EDGE ( 'NONE', *, *, #31222, .T. ) ;
#19646 = LINE ( 'NONE', #37506, #35685 ) ;
#19647 = LINE ( 'NONE', #32686, #21820 ) ;
#19648 = VECTOR ( 'NONE', #22226, 1000.000000000000227 ) ;
#19649 = VECTOR ( 'NONE', #6668, 1000.000000000000227 ) ;
#19650 = DIRECTION ( 'NONE',  ( 0.8660254037844380415, 0.5000000000000011102, 0.000000000000000000 ) ) ;
#19651 = CARTESIAN_POINT ( 'NONE',  ( -14.59604210131933577, 0.000000000000000000, 3.229489071685041068 ) ) ;
#19652 = EDGE_CURVE ( 'NONE', #49950, #33592, #3740, .T. ) ;
#19653 = DIRECTION ( 'NONE',  ( 0.007781995580012663651, -3.146120232559066537E-19, -0.9999697198139514409 ) ) ;
#19654 = ORIENTED_EDGE ( 'NONE', *, *, #21246, .F. ) ;
#19655 = VECTOR ( 'NONE', #15849, 999.9999999999998863 ) ;
#19656 = ORIENTED_EDGE ( 'NONE', *, *, #7075, .T. ) ;
#19657 = EDGE_CURVE ( 'NONE', #15538, #26566, #13664, .T. ) ;
#19658 = DIRECTION ( 'NONE',  ( 0.000000000000000000, -0.000000000000000000, -1.000000000000000000 ) ) ;
#19659 = LINE ( 'NONE', #14553, #39307 ) ;
#19660 = EDGE_CURVE ( 'NONE', #36681, #25334, #48297, .T. ) ;
#19661 = VECTOR ( 'NONE', #50754, 1000.000000000000000 ) ;
#19662 = ORIENTED_EDGE ( 'NONE', *, *, #44341, .F. ) ;
#19663 = CARTESIAN_POINT ( 'NONE',  ( -17.46532115785441519, 0.000000000000000000, 13.67492996699914265 ) ) ;
#19664 = ORIENTED_EDGE ( 'NONE', *, *, #36764, .F. ) ;
#19665 = FACE_OUTER_BOUND ( 'NONE', #16650, .T. ) ;
#19666 = EDGE_CURVE ( 'NONE', #46158, #48080, #56015, .T. ) ;
#19667 = VECTOR ( 'NONE', #21825, 1000.000000000000114 ) ;
#19668 = VECTOR ( 'NONE', #8252, 1000.000000000000227 ) ;
#19669 = VERTEX_POINT ( 'NONE', #4592 ) ;
#19670 = ORIENTED_EDGE ( 'NONE', *, *, #23312, .F. ) ;
#19671 = CARTESIAN_POINT ( 'NONE',  ( -20.81378277464309434, 4.010151117816509903, 11.54744235706348654 ) ) ;
#19672 = DIRECTION ( 'NONE',  ( 0.9999697198139515519, 0.000000000000000000, 0.007781995580013368816 ) ) ;
#19673 = CARTESIAN_POINT ( 'NONE',  ( -17.74404816805336793, 0.000000000000000000, 3.574322630375089460 ) ) ;
#19674 = VERTEX_POINT ( 'NONE', #34161 ) ;
#19675 = DIRECTION ( 'NONE',  ( -0.5364919789714478471, 0.6444004775717705469, -0.5449076811759709926 ) ) ;
#19676 = ORIENTED_EDGE ( 'NONE', *, *, #33502, .F. ) ;
#19677 = VECTOR ( 'NONE', #29620, 1000.000000000000227 ) ;
#19678 = ORIENTED_EDGE ( 'NONE', *, *, #41735, .T. ) ;
#19679 = EDGE_LOOP ( 'NONE', ( #15493, #14109, #31556, #21822 ) ) ;
#19680 = DIRECTION ( 'NONE',  ( -0.5364919789714478471, 0.6444004775717705469, -0.5449076811759709926 ) ) ;
#19681 = ORIENTED_EDGE ( 'NONE', *, *, #42598, .T. ) ;
#19682 = PLANE ( 'NONE',  #21209 ) ;
#19683 = ORIENTED_EDGE ( 'NONE', *, *, #10970, .T. ) ;
#19684 = DIRECTION ( 'NONE',  ( 0.8531650599175529814, -0.4028455766673920135, -0.3313982828793697877 ) ) ;
#19685 = LINE ( 'NONE', #42083, #14115 ) ;
#19686 = VERTEX_POINT ( 'NONE', #8290 ) ;
#19687 = AXIS2_PLACEMENT_3D ( 'NONE', #18841, #48927, #40413 ) ;
#19688 = CARTESIAN_POINT ( 'NONE',  ( -13.02381224048627040, 0.000000000000000000, 6.027055072872212982 ) ) ;
#19689 = ORIENTED_EDGE ( 'NONE', *, *, #22681, .F. ) ;
#19690 = VECTOR ( 'NONE', #20254, 1000.000000000000000 ) ;
#19691 = DIRECTION ( 'NONE',  ( 0.005002170337468016433, -0.7660444431189770143, -0.6427681459581293666 ) ) ;
#19692 = DIRECTION ( 'NONE',  ( 0.005961354470445682716, -0.6427876096865404731, -0.7660212471507180654 ) ) ;
#19693 = CARTESIAN_POINT ( 'NONE',  ( -21.41819867739107153, 4.172053068839010059, 12.04792670369172036 ) ) ;
#19694 = CARTESIAN_POINT ( 'NONE',  ( -14.20280369269832832, 0.000000000000000000, 12.40765738797303719 ) ) ;
#19695 = FACE_OUTER_BOUND ( 'NONE', #29558, .T. ) ;
#19696 = LINE ( 'NONE', #15172, #16538 ) ;
#19697 = ORIENTED_EDGE ( 'NONE', *, *, #23519, .F. ) ;
#19698 = EDGE_CURVE ( 'NONE', #485, #55742, #51472, .T. ) ;
#19699 = ORIENTED_EDGE ( 'NONE', *, *, #22697, .F. ) ;
#19700 = AXIS2_PLACEMENT_3D ( 'NONE', #3290, #52098, #42470 ) ;
#19701 = DIRECTION ( 'NONE',  ( 0.007781995580012662783, 0.000000000000000000, -0.9999697198139514409 ) ) ;
#19702 = LINE ( 'NONE', #36744, #6715 ) ;
#19703 = EDGE_CURVE ( 'NONE', #48176, #38162, #43245, .T. ) ;
#19704 = ADVANCED_FACE ( 'NONE', ( #17106 ), #4339, .F. ) ;
#19705 = CARTESIAN_POINT ( 'NONE',  ( -14.94916102560700821, 0.000000000000000000, 2.688082935172642962 ) ) ;
#19706 = CARTESIAN_POINT ( 'NONE',  ( -10.88050332570665546, 0.000000000000000000, 3.458410309791905224 ) ) ;
#19707 = CARTESIAN_POINT ( 'NONE',  ( -24.57312852195785524, 18.34675584111407787, 4.549864924635812713 ) ) ;
#19708 = ORIENTED_EDGE ( 'NONE', *, *, #30663, .F. ) ;
#19709 = DIRECTION ( 'NONE',  ( 0.007781995580012662783, 0.000000000000000000, -0.9999697198139514409 ) ) ;
#19710 = LINE ( 'NONE', #14601, #55891 ) ;
#19711 = VERTEX_POINT ( 'NONE', #36369 ) ;
#19712 = DIRECTION ( 'NONE',  ( -0.005002170337468016433, -0.7660444431189770143, 0.6427681459581293666 ) ) ;
#19713 = LINE ( 'NONE', #54338, #29544 ) ;
#19714 = ORIENTED_EDGE ( 'NONE', *, *, #24405, .T. ) ;
#19715 = FACE_OUTER_BOUND ( 'NONE', #48189, .T. ) ;
#19716 = CARTESIAN_POINT ( 'NONE',  ( -56.66762604419704985, 5.055998648713354804, 2.999999999999993339 ) ) ;
#19717 = CARTESIAN_POINT ( 'NONE',  ( -18.13558483980604308, 2.553033558614008047, 3.644953633207256072 ) ) ;
#19718 = CARTESIAN_POINT ( 'NONE',  ( -21.47419595591918906, 0.000000000000000000, 5.222628093224860102 ) ) ;
#19719 = CARTESIAN_POINT ( 'NONE',  ( -69.96913243261153070, 2.000000000000049738, 7.657023247222836559 ) ) ;
#19720 = ORIENTED_EDGE ( 'NONE', *, *, #14649, .T. ) ;
#19721 = EDGE_LOOP ( 'NONE', ( #25487, #1519, #51273, #162 ) ) ;
#19722 = CARTESIAN_POINT ( 'NONE',  ( -11.14802033209023158, 0.000000000000000000, 3.825660500397664254 ) ) ;
#19723 = CARTESIAN_POINT ( 'NONE',  ( -14.59029399430876950, 0.000000000000000000, 2.490869665169511915 ) ) ;
#19724 = LINE ( 'NONE', #41834, #40579 ) ;
#19725 = CARTESIAN_POINT ( 'NONE',  ( -16.40688773272033885, -0.1159828484229834950, 9.591365951305096615 ) ) ;
#19726 = CARTESIAN_POINT ( 'NONE',  ( -16.01007116637957495, 0.000000000000000000, 5.803809259185364056 ) ) ;
#19727 = DIRECTION ( 'NONE',  ( -0.5364919789714478471, 0.6444004775717705469, -0.5449076811759709926 ) ) ;
#19728 = EDGE_LOOP ( 'NONE', ( #37380, #35376, #37066, #41573 ) ) ;
#19729 = CARTESIAN_POINT ( 'NONE',  ( -12.80458192191714595, 0.000000000000000000, 11.86454056839041726 ) ) ;
#19730 = EDGE_CURVE ( 'NONE', #14403, #29996, #5439, .T. ) ;
#19732 = AXIS2_PLACEMENT_3D ( 'NONE', #21747, #39062, #5539 ) ;
#19731 = CARTESIAN_POINT ( 'NONE',  ( -14.39604815735654597, 0.000000000000000000, 3.231045470801043429 ) ) ;
#19733 = CARTESIAN_POINT ( 'NONE',  ( -12.60458797795435615, 0.000000000000000000, 11.86609696750642229 ) ) ;
#19734 = EDGE_LOOP ( 'NONE', ( #15675, #7040, #27848, #10354 ) ) ;
#19735 = EDGE_CURVE ( 'NONE', #35539, #34834, #10253, .T. ) ;
#19736 = FACE_OUTER_BOUND ( 'NONE', #42310, .T. ) ;
#19737 = DIRECTION ( 'NONE',  ( -0.005961354470445682716, -0.6427876096865404731, 0.7660212471507180654 ) ) ;
#19738 = EDGE_CURVE ( 'NONE', #42394, #17567, #20995, .T. ) ;
#19739 = DIRECTION ( 'NONE',  ( -0.5364919789714478471, 0.6444004775717705469, -0.5449076811759709926 ) ) ;
#19740 = VERTEX_POINT ( 'NONE', #31831 ) ;
#19741 = AXIS2_PLACEMENT_3D ( 'NONE', #38065, #55115, #42600 ) ;
#19742 = LINE ( 'NONE', #23992, #12326 ) ;
#19743 = EDGE_CURVE ( 'NONE', #14535, #18621, #36661, .T. ) ;
#19744 = EDGE_LOOP ( 'NONE', ( #42095, #20573, #48976, #51803 ) ) ;
#19745 = EDGE_LOOP ( 'NONE', ( #40889, #35179, #7787, #39645 ) ) ;
#19746 = ORIENTED_EDGE ( 'NONE', *, *, #31356, .T. ) ;
#19747 = ORIENTED_EDGE ( 'NONE', *, *, #38868, .F. ) ;
#19748 = ORIENTED_EDGE ( 'NONE', *, *, #26064, .T. ) ;
#19749 = FACE_OUTER_BOUND ( 'NONE', #21846, .T. ) ;
#19750 = ORIENTED_EDGE ( 'NONE', *, *, #44421, .F. ) ;
#19751 = VERTEX_POINT ( 'NONE', #35830 ) ;
#19752 = CARTESIAN_POINT ( 'NONE',  ( -25.20123094555300369, 0.000000000000000000, 6.470945668149052032 ) ) ;
#19753 = ORIENTED_EDGE ( 'NONE', *, *, #18986, .F. ) ;
#19754 = ORIENTED_EDGE ( 'NONE', *, *, #18726, .T. ) ;
#19755 = EDGE_CURVE ( 'NONE', #20189, #30522, #44060, .T. ) ;
#19756 = EDGE_LOOP ( 'NONE', ( #45414, #5442, #39823, #20653 ) ) ;
#19757 = CARTESIAN_POINT ( 'NONE',  ( -23.33693525117809386, 0.000000000000000000, 5.746789908705562944 ) ) ;
#19758 = DIRECTION ( 'NONE',  ( 0.005002170337468016433, -0.7660444431189770143, -0.6427681459581293666 ) ) ;
#19759 = CARTESIAN_POINT ( 'NONE',  ( -22.14101869848777682, 19.68270265044663958, 4.490773887887535842 ) ) ;
#19760 = FACE_OUTER_BOUND ( 'NONE', #23100, .T. ) ;
#19761 = EDGE_CURVE ( 'NONE', #34418, #25320, #5715, .T. ) ;
#19762 = VERTEX_POINT ( 'NONE', #23587 ) ;
#19763 = CARTESIAN_POINT ( 'NONE',  ( -16.76964795026778532, 0.000000000000000000, 9.691224811305781728 ) ) ;
#19764 = ORIENTED_EDGE ( 'NONE', *, *, #18938, .T. ) ;
#19765 = EDGE_LOOP ( 'NONE', ( #40586, #48157, #21548, #4588 ) ) ;
#19766 = EDGE_CURVE ( 'NONE', #39800, #7659, #40360, .T. ) ;
#19767 = LINE ( 'NONE', #37090, #11349 ) ;
#19768 = DIRECTION ( 'NONE',  ( 0.007781995580012663651, -3.146120232559066537E-19, -0.9999697198139514409 ) ) ;
#19769 = ADVANCED_FACE ( 'NONE', ( #5179 ), #48884, .F. ) ;
#19770 = EDGE_CURVE ( 'NONE', #8057, #7579, #10562, .T. ) ;
#19771 = LINE ( 'NONE', #41059, #15175 ) ;
#19772 = DIRECTION ( 'NONE',  ( 0.000000000000000000, -1.000000000000000000, 0.000000000000000000 ) ) ;
#19773 = CARTESIAN_POINT ( 'NONE',  ( 4.866417447938705898, 0.000000000000000000, -1.967953638240998337 ) ) ;
#19774 = LINE ( 'NONE', #23482, #43123 ) ;
#19775 = ORIENTED_EDGE ( 'NONE', *, *, #10615, .T. ) ;
#19776 = FACE_OUTER_BOUND ( 'NONE', #9194, .T. ) ;
#19777 = ORIENTED_EDGE ( 'NONE', *, *, #30639, .F. ) ;
#19778 = VECTOR ( 'NONE', #51279, 1000.000000000000000 ) ;
#19779 = CARTESIAN_POINT ( 'NONE',  ( -8.949704955220703084, -0.1159828484229828427, 6.694742913531133155 ) ) ;
#19780 = LINE ( 'NONE', #23489, #44142 ) ;
#19781 = PRODUCT_RELATED_PRODUCT_CATEGORY ( 'part', '', ( #22381 ) ) ;
#19782 = CARTESIAN_POINT ( 'NONE',  ( -30.79567442779373110, 0.000000000000000000, 8.843406890442315316 ) ) ;
#19783 = DIRECTION ( 'NONE',  ( 0.007781995580012663651, 0.000000000000000000, -0.9999697198139515519 ) ) ;
#19784 = LINE ( 'NONE', #49620, #26851 ) ;
#19785 = EDGE_CURVE ( 'NONE', #33865, #51703, #36117, .T. ) ;
#19786 = ORIENTED_EDGE ( 'NONE', *, *, #32921, .T. ) ;
#19787 = CARTESIAN_POINT ( 'NONE',  ( -29.86352658060627618, 0.000000000000000000, 8.481329010720569883 ) ) ;
#19788 = DIRECTION ( 'NONE',  ( 0.007781995580012663651, -3.146120232559066537E-19, -0.9999697198139514409 ) ) ;
#19789 = DIRECTION ( 'NONE',  ( -0.7660212471507179544, -0.6427876096865405842, -0.005961354470445141482 ) ) ;
#19790 = DIRECTION ( 'NONE',  ( 0.007781995580012663651, -3.146120232559066537E-19, -0.9999697198139514409 ) ) ;
#19791 = CARTESIAN_POINT ( 'NONE',  ( -20.06177075545399191, 0.000000000000000000, 14.76272000528038220 ) ) ;
#19792 = PLANE ( 'NONE',  #20006 ) ;
#19793 = DIRECTION ( 'NONE',  ( -0.5449076811759708816, 0.6444004775717707689, 0.5364919789714475140 ) ) ;
#19794 = LINE ( 'NONE', #36860, #43217 ) ;
#19795 = CARTESIAN_POINT ( 'NONE',  ( -19.93268291358662481, 3.524445264749008100, 10.40806719690053050 ) ) ;
#19796 = ORIENTED_EDGE ( 'NONE', *, *, #40614, .T. ) ;
#19797 = EDGE_LOOP ( 'NONE', ( #23323, #8501, #49517, #27484 ) ) ;
#19798 = EDGE_CURVE ( 'NONE', #28974, #55568, #18202, .T. ) ;
#19799 = ORIENTED_EDGE ( 'NONE', *, *, #56074, .T. ) ;
#19800 = ORIENTED_EDGE ( 'NONE', *, *, #471, .T. ) ;
#19801 = EDGE_CURVE ( 'NONE', #54647, #52427, #49442, .T. ) ;
#19802 = EDGE_LOOP ( 'NONE', ( #34725, #4019, #25454, #24657 ) ) ;
#19803 = ORIENTED_EDGE ( 'NONE', *, *, #48286, .F. ) ;
#19804 = FACE_OUTER_BOUND ( 'NONE', #12568, .T. ) ;
#19805 = CARTESIAN_POINT ( 'NONE',  ( -16.50085385711260599, 0.6102101463440035012, 3.071954842479957204 ) ) ;
#19806 = CARTESIAN_POINT ( 'NONE',  ( -14.46888367232926420, 0.000000000000000000, 12.59025272694991315 ) ) ;
#19807 = EDGE_CURVE ( 'NONE', #23468, #35736, #1985, .T. ) ;
#19808 = CIRCLE ( 'NONE', #1691, 2.749999999999998224 ) ;
#19809 = EDGE_LOOP ( 'NONE', ( #5411, #38326, #3458, #52462 ) ) ;
#19810 = CARTESIAN_POINT ( 'NONE',  ( -10.23024275242918968, 0.000000000000000000, 5.310131136964741039 ) ) ;
#19811 = VERTEX_POINT ( 'NONE', #53421 ) ;
#19812 = ADVANCED_FACE ( 'NONE', ( #14262 ), #6019, .F. ) ;
#19813 = EDGE_LOOP ( 'NONE', ( #54045, #12446, #21694, #5112 ) ) ;
#19814 = EDGE_CURVE ( 'NONE', #41874, #21510, #23334, .T. ) ;
#19815 = CARTESIAN_POINT ( 'NONE',  ( -66.55921131444038963, -8.722325662721239325, 0.3393403235802882056 ) ) ;
#19816 = LINE ( 'NONE', #7303, #9253 ) ;
#19817 = PLANE ( 'NONE',  #3285 ) ;
#19818 = EDGE_CURVE ( 'NONE', #42377, #5037, #15093, .T. ) ;
#19819 = ORIENTED_EDGE ( 'NONE', *, *, #18218, .F. ) ;
#19820 = PLANE ( 'NONE',  #19213 ) ;
#19821 = CARTESIAN_POINT ( 'NONE',  ( -11.81109477377810180, 0.000000000000000000, 3.620494245550860857 ) ) ;
#19822 = ADVANCED_FACE ( 'NONE', ( #39805 ), #35529, .F. ) ;
#19823 = CARTESIAN_POINT ( 'NONE',  ( -20.13191613428482185, -2.946525016555661125, 4.607231451707245462 ) ) ;
#19824 = ADVANCED_FACE ( 'NONE', ( #48605 ), #11371, .F. ) ;
#19825 = DIRECTION ( 'NONE',  ( 0.005002170337468016433, -0.7660444431189770143, -0.6427681459581293666 ) ) ;
#19826 = LINE ( 'NONE', #28334, #20600 ) ;
#19827 = LINE ( 'NONE', #53901, #15910 ) ;
#19828 = CARTESIAN_POINT ( 'NONE',  ( -11.40636015113596180, 0.000000000000000000, 11.32142374880780089 ) ) ;
#19829 = LINE ( 'NONE', #23533, #49332 ) ;
#19830 = LINE ( 'NONE', #50761, #36558 ) ;
#19831 = ORIENTED_EDGE ( 'NONE', *, *, #17496, .F. ) ;
#19832 = CARTESIAN_POINT ( 'NONE',  ( 0.3240706152708106025, -3.670543518250628967, -1.335466778558061241E-15 ) ) ;
#19833 = ORIENTED_EDGE ( 'NONE', *, *, #2873, .T. ) ;
#19834 = EDGE_CURVE ( 'NONE', #43196, #41770, #50559, .T. ) ;
#19835 = LINE ( 'NONE', #37419, #22014 ) ;
#19836 = LINE ( 'NONE', #53913, #32317 ) ;
#19837 = FACE_OUTER_BOUND ( 'NONE', #24020, .T. ) ;
#19838 = LINE ( 'NONE', #37158, #29593 ) ;
#19839 = DIRECTION ( 'NONE',  ( 0.7660212471507180654, -0.6427876096865404731, 0.005961354470445141482 ) ) ;
#19840 = EDGE_CURVE ( 'NONE', #37474, #37895, #2820, .T. ) ;
#19841 = DIRECTION ( 'NONE',  ( 0.5364919789714477361, 0.6444004775717706579, 0.5449076811759711036 ) ) ;
#19842 = DIRECTION ( 'NONE',  ( 0.000000000000000000, 0.000000000000000000, 1.000000000000000000 ) ) ;
#19843 = ORIENTED_EDGE ( 'NONE', *, *, #51181, .T. ) ;
#19844 = CARTESIAN_POINT ( 'NONE',  ( -17.16820509746884582, -4.889348428825661230, 11.37489936847406291 ) ) ;
#19845 = DIRECTION ( 'NONE',  ( -0.5364919789714478471, 0.6444004775717705469, -0.5449076811759709926 ) ) ;
#19846 = CARTESIAN_POINT ( 'NONE',  ( -13.73672976910459909, 0.000000000000000000, 12.22661844811216270 ) ) ;
#19847 = DIRECTION ( 'NONE',  ( 0.000000000000000000, -1.000000000000000000, 0.000000000000000000 ) ) ;
#19848 = PLANE ( 'NONE',  #17810 ) ;
#19849 = MECHANICAL_DESIGN_GEOMETRIC_PRESENTATION_REPRESENTATION (  '', ( #32581 ), #40740 ) ;
#19850 = CARTESIAN_POINT ( 'NONE',  ( -20.54049170961573267, 0.000000000000000000, 4.660556269540326646 ) ) ;
#19851 = CARTESIAN_POINT ( 'NONE',  ( -26.13337879274045505, 0.000000000000000000, 6.833023547870798353 ) ) ;
#19852 = DIRECTION ( 'NONE',  ( -0.3620778797217456546, 0.000000000000000000, -0.9321478471874540261 ) ) ;
#19853 = CARTESIAN_POINT ( 'NONE',  ( -16.06709938707323460, 0.000000000000000000, 13.13181314741652628 ) ) ;
#19854 = ORIENTED_EDGE ( 'NONE', *, *, #1517, .T. ) ;
#19855 = LINE ( 'NONE', #38020, #53031 ) ;
#19856 = ORIENTED_EDGE ( 'NONE', *, *, #39360, .F. ) ;
#19857 = LINE ( 'NONE', #24661, #11409 ) ;
#19858 = CARTESIAN_POINT ( 'NONE',  ( -13.10578669187797018, -0.1191753592594188005, 3.710421681786226777 ) ) ;
#19859 = EDGE_LOOP ( 'NONE', ( #23925, #11976, #49425, #6206 ) ) ;
#19860 = EDGE_CURVE ( 'NONE', #47452, #45757, #15605, .T. ) ;
#19861 = ADVANCED_FACE ( 'NONE', ( #28125 ), #19622, .F. ) ;
#19862 = EDGE_LOOP ( 'NONE', ( #33623, #14386, #17268, #30756 ) ) ;
#19863 = DIRECTION ( 'NONE',  ( -0.7660212471507179544, -0.6427876096865405842, -0.005961354470445141482 ) ) ;
#19864 = ORIENTED_EDGE ( 'NONE', *, *, #2651, .T. ) ;
#19865 = ORIENTED_EDGE ( 'NONE', *, *, #47186, .F. ) ;
#19866 = ORIENTED_EDGE ( 'NONE', *, *, #40791, .T. ) ;
#19867 = CARTESIAN_POINT ( 'NONE',  ( -11.88300507327610411, 2.876837460659008361, 1.205908273609587189 ) ) ;
#19868 = PLANE ( 'NONE',  #33253 ) ;
#19869 = CARTESIAN_POINT ( 'NONE',  ( -8.409922665610809034, 0.000000000000000000, 10.23674650875856962 ) ) ;
#19870 = EDGE_CURVE ( 'NONE', #43429, #33308, #29729, .T. ) ;
#19871 = ADVANCED_FACE ( 'NONE', ( #55358 ), #7374, .F. ) ;
#19872 = ORIENTED_EDGE ( 'NONE', *, *, #22094, .T. ) ;
#19873 = VERTEX_POINT ( 'NONE', #16452 ) ;
#19874 = EDGE_CURVE ( 'NONE', #17790, #41029, #33781, .T. ) ;
#19875 = CARTESIAN_POINT ( 'NONE',  ( -65.83373593673759672, -1.561251128379126385E-14, 2.627585852360243113 ) ) ;
#19876 = CARTESIAN_POINT ( 'NONE',  ( -12.23851102634202448, -0.1191753592594197858, 11.68427982808754884 ) ) ;
#19877 = ORIENTED_EDGE ( 'NONE', *, *, #782, .T. ) ;
#19878 = PLANE ( 'NONE',  #27330 ) ;
#19879 = ORIENTED_EDGE ( 'NONE', *, *, #22536, .F. ) ;
#19880 = DIRECTION ( 'NONE',  ( 0.7660212471507180654, -0.6427876096865404731, 0.005961354470445141482 ) ) ;
#19881 = PLANE ( 'NONE',  #28508 ) ;
#19882 = VERTEX_POINT ( 'NONE', #24422 ) ;
#19883 = DIRECTION ( 'NONE',  ( -0.7660212471507179544, -0.6427876096865405842, -0.005961354470445141482 ) ) ;
#19884 = ADVANCED_FACE ( 'NONE', ( #24693 ), #28971, .F. ) ;
#19885 = ADVANCED_FACE ( 'NONE', ( #28401 ), #42017, .F. ) ;
#19886 = FACE_OUTER_BOUND ( 'NONE', #34342, .T. ) ;
#19887 = ORIENTED_EDGE ( 'NONE', *, *, #19188, .F. ) ;
#19888 = DIRECTION ( 'NONE',  ( 0.007781995580012663651, 0.000000000000000000, -0.9999697198139515519 ) ) ;
#19889 = DIRECTION ( 'NONE',  ( -0.5449076811759708816, 0.6444004775717707689, 0.5364919789714475140 ) ) ;
#19890 = ADVANCED_FACE ( 'NONE', ( #51099 ), #54799, .F. ) ;
#19891 = CARTESIAN_POINT ( 'NONE',  ( -18.39746900504187010, 0.000000000000000000, 14.03700784672088808 ) ) ;
#19892 = EDGE_LOOP ( 'NONE', ( #23460, #16930, #2640, #10061 ) ) ;
#19893 = EDGE_CURVE ( 'NONE', #2943, #32088, #41189, .T. ) ;
#19894 = DIRECTION ( 'NONE',  ( 0.5449076811759707706, 0.6444004775717708799, -0.5364919789714476250 ) ) ;
#19895 = LINE ( 'NONE', #54515, #42341 ) ;
#19896 = LINE ( 'NONE', #28984, #48500 ) ;
#19897 = LINE ( 'NONE', #55112, #47702 ) ;
#19898 = FACE_OUTER_BOUND ( 'NONE', #50336, .T. ) ;
#19899 = FACE_OUTER_BOUND ( 'NONE', #36099, .T. ) ;
#19900 = FACE_OUTER_BOUND ( 'NONE', #53140, .T. ) ;
#19901 = VERTEX_POINT ( 'NONE', #45434 ) ;
#19902 = PLANE ( 'NONE',  #7170 ) ;
#19903 = CARTESIAN_POINT ( 'NONE',  ( -10.94028622754223967, 0.000000000000000000, 11.14038480894692995 ) ) ;
#19904 = CARTESIAN_POINT ( 'NONE',  ( -67.94414157437554991, -0.6013562474879498021, -4.659789304345617111 ) ) ;
#19905 = ORIENTED_EDGE ( 'NONE', *, *, #35705, .T. ) ;
#19906 = DIRECTION ( 'NONE',  ( -0.5449076811759708816, 0.6444004775717707689, 0.5364919789714475140 ) ) ;
#19907 = PLANE ( 'NONE',  #32 ) ;
#19908 = DIRECTION ( 'NONE',  ( -0.005002170337468016433, -0.7660444431189770143, 0.6427681459581293666 ) ) ;
#19909 = CARTESIAN_POINT ( 'NONE',  ( -11.77243710274829525, -0.1191753592594197858, 11.50324088822667612 ) ) ;
#19910 = DIRECTION ( 'NONE',  ( 0.6427681459581294776, -0.7660444431189769032, 0.005002170337467562802 ) ) ;
#19911 = EDGE_LOOP ( 'NONE', ( #29919, #8741, #6165, #53301 ) ) ;
#19912 = ORIENTED_EDGE ( 'NONE', *, *, #50106, .F. ) ;
#19913 = DIRECTION ( 'NONE',  ( 0.9999697198139515519, 0.000000000000000000, 0.007781995580013368816 ) ) ;
#19914 = EDGE_CURVE ( 'NONE', #15067, #24549, #6548, .T. ) ;
#19915 = CARTESIAN_POINT ( 'NONE',  ( 4.994031378522669762, 0.000000000000000000, -2.289010529401725780 ) ) ;
#19916 = PRODUCT_DEFINITION_FORMATION_WITH_SPECIFIED_SOURCE ( 'ANY', '', #27850, .NOT_KNOWN. ) ;
#19917 = LINE ( 'NONE', #10086, #46507 ) ;
#19918 = VERTEX_POINT ( 'NONE', #15350 ) ;
#19919 = CARTESIAN_POINT ( 'NONE',  ( -13.73672976910459909, 0.000000000000000000, 12.22661844811216270 ) ) ;
#19920 = EDGE_CURVE ( 'NONE', #12052, #11173, #49967, .T. ) ;
#19921 = ORIENTED_EDGE ( 'NONE', *, *, #31766, .T. ) ;
#19922 = CARTESIAN_POINT ( 'NONE',  ( -14.16014573953108169, 0.000000000000000000, 6.926202016030694963 ) ) ;
#19923 = ORIENTED_EDGE ( 'NONE', *, *, #39728, .F. ) ;
#19924 = ORIENTED_EDGE ( 'NONE', *, *, #6156, .T. ) ;
#19925 = DIRECTION ( 'NONE',  ( 0.9999697198139515519, 0.000000000000000000, 0.007781995580013368816 ) ) ;
#19926 = CARTESIAN_POINT ( 'NONE',  ( -19.79569077582305070, 0.000000000000000000, 14.58012466630350445 ) ) ;
#19927 = LINE ( 'NONE', #32998, #346 ) ;
#19928 = ADVANCED_FACE ( 'NONE', ( #45717 ), #41482, .F. ) ;
#19929 = EDGE_CURVE ( 'NONE', #12677, #52731, #25280, .T. ) ;
#19930 = EDGE_CURVE ( 'NONE', #6528, #52808, #9069, .T. ) ;
#19931 = ORIENTED_EDGE ( 'NONE', *, *, #19874, .T. ) ;
#19932 = CARTESIAN_POINT ( 'NONE',  ( -14.01545677930355183, 0.000000000000000000, 2.126011111488108174 ) ) ;
#19933 = ORIENTED_EDGE ( 'NONE', *, *, #5793, .F. ) ;
#19934 = EDGE_CURVE ( 'NONE', #5501, #47873, #55948, .T. ) ;
#19935 = ORIENTED_EDGE ( 'NONE', *, *, #42608, .F. ) ;
#19936 = ORIENTED_EDGE ( 'NONE', *, *, #39397, .F. ) ;
#19937 = LINE ( 'NONE', #23923, #41310 ) ;
#19938 = VERTEX_POINT ( 'NONE', #26123 ) ;
#19939 = CARTESIAN_POINT ( 'NONE',  ( -17.31913335200585280, -0.1191753592594158168, 7.740285211709545976 ) ) ;
#19940 = ORIENTED_EDGE ( 'NONE', *, *, #23171, .T. ) ;
#19941 = DIRECTION ( 'NONE',  ( 0.6427681459581294776, -0.7660444431189769032, 0.005002170337467562802 ) ) ;
#19942 = CARTESIAN_POINT ( 'NONE',  ( -18.39353927776868503, 5.629170628041515023, 3.647007019221114810 ) ) ;
#19943 = ORIENTED_EDGE ( 'NONE', *, *, #56180, .T. ) ;
#19944 = PLANE ( 'NONE',  #25001 ) ;
#19945 = ORIENTED_EDGE ( 'NONE', *, *, #28749, .F. ) ;
#19946 = ADVANCED_FACE ( 'NONE', ( #55645 ), #39159, .F. ) ;
#19947 = AXIS2_PLACEMENT_3D ( 'NONE', #10687, #14923, #35382 ) ;
#19948 = ADVANCED_FACE ( 'NONE', ( #3964 ), #12766, .F. ) ;
#19949 = PLANE ( 'NONE',  #1056 ) ;
#19950 = CARTESIAN_POINT ( 'NONE',  ( -9.310908773652148085, 0.000000000000000000, 6.594607829569027579 ) ) ;
#19951 = FACE_OUTER_BOUND ( 'NONE', #43368, .T. ) ;
#19952 = PLANE ( 'NONE',  #32943 ) ;
#19953 = EDGE_CURVE ( 'NONE', #38023, #48125, #17044, .T. ) ;
#19954 = CARTESIAN_POINT ( 'NONE',  ( -23.33771345073609638, -0.1191753592594197858, 5.846786880686956955 ) ) ;
#19955 = CARTESIAN_POINT ( 'NONE',  ( -60.92294909528611413, 7.225036622302098976, 2.999999999999993339 ) ) ;
#19956 = ORIENTED_EDGE ( 'NONE', *, *, #7298, .F. ) ;
#19958 = ORIENTED_EDGE ( 'NONE', *, *, #14936, .T. ) ;
#19957 = EDGE_CURVE ( 'NONE', #47084, #31029, #17588, .T. ) ;
#19959 = CARTESIAN_POINT ( 'NONE',  ( -17.77514808833108262, -0.1191753592594194527, 6.628740190168248780 ) ) ;
#19960 = DIRECTION ( 'NONE',  ( 0.9999697198139515519, 0.000000000000000000, 0.007781995580013368816 ) ) ;
#19961 = LINE ( 'NONE', #7199, #37564 ) ;
#19962 = EDGE_CURVE ( 'NONE', #29543, #678, #47968, .T. ) ;
#19963 = DIRECTION ( 'NONE',  ( 0.005961354470445682716, -0.6427876096865404731, -0.7660212471507180654 ) ) ;
#19964 = LINE ( 'NONE', #7201, #40366 ) ;
#19965 = ORIENTED_EDGE ( 'NONE', *, *, #14690, .T. ) ;
#19966 = DIRECTION ( 'NONE',  ( 0.000000000000000000, -1.000000000000000000, 0.000000000000000000 ) ) ;
#19967 = FACE_OUTER_BOUND ( 'NONE', #3630, .T. ) ;
#19968 = ORIENTED_EDGE ( 'NONE', *, *, #37925, .T. ) ;
#19969 = LINE ( 'NONE', #1805, #22048 ) ;
#19970 = DIRECTION ( 'NONE',  ( 0.007781995580012662783, 0.000000000000000000, -0.9999697198139514409 ) ) ;
#19971 = ORIENTED_EDGE ( 'NONE', *, *, #17850, .F. ) ;
#19972 = DIRECTION ( 'NONE',  ( -0.9999697198139514409, -0.000000000000000000, -0.007781995580013368816 ) ) ;
#19973 = CARTESIAN_POINT ( 'NONE',  ( -14.93495759592298988, 0.000000000000000000, 12.77129166681078409 ) ) ;
#19974 = FACE_OUTER_BOUND ( 'NONE', #9468, .T. ) ;
#19975 = DIRECTION ( 'NONE',  ( 0.005002170337468016433, -0.7660444431189770143, -0.6427681459581293666 ) ) ;
#19976 = DIRECTION ( 'NONE',  ( -0.9999697198139514409, -0.000000000000000000, -0.007781995580013368816 ) ) ;
#19977 = EDGE_LOOP ( 'NONE', ( #27638, #20803, #4153, #30842 ) ) ;
#19978 = ORIENTED_EDGE ( 'NONE', *, *, #14206, .T. ) ;
#19979 = DIRECTION ( 'NONE',  ( -0.5449076811759708816, 0.6444004775717707689, 0.5364919789714475140 ) ) ;
#19980 = DIRECTION ( 'NONE',  ( 0.9999697198139515519, 0.000000000000000000, 0.007781995580013368816 ) ) ;
#19981 = DIRECTION ( 'NONE',  ( 0.007781995580012663651, 0.000000000000000000, -0.9999697198139515519 ) ) ;
#19982 = CARTESIAN_POINT ( 'NONE',  ( -18.35049997161669566, 0.000000000000000000, 8.001587919891903766 ) ) ;
#19983 = CARTESIAN_POINT ( 'NONE',  ( -18.70154782850797659, -0.1191753592594164690, 6.252198663374462839 ) ) ;
#19984 = LINE ( 'NONE', #32769, #32194 ) ;
#19985 = VERTEX_POINT ( 'NONE', #8819 ) ;
#19986 = DIRECTION ( 'NONE',  ( -0.005961354470445682716, -0.6427876096865404731, 0.7660212471507180654 ) ) ;
#19987 = VECTOR ( 'NONE', #17067, 1000.000000000000227 ) ;
#19988 = CARTESIAN_POINT ( 'NONE',  ( -19.60990026154428278, 0.000000000000000000, 4.498472333781370125 ) ) ;
#19989 = FACE_OUTER_BOUND ( 'NONE', #220, .T. ) ;
#19990 = ORIENTED_EDGE ( 'NONE', *, *, #50231, .F. ) ;
#19991 = CARTESIAN_POINT ( 'NONE',  ( -68.51296364132990391, -11.00146576780565866, 7.485090880804395219 ) ) ;
#19992 = CARTESIAN_POINT ( 'NONE',  ( -12.15271748404464880, 0.000000000000000000, 1.601849296007406664 ) ) ;
#19993 = CARTESIAN_POINT ( 'NONE',  ( -16.64402593923450979, 4.657758921906512306, 2.998429744135719943 ) ) ;
#19994 = EDGE_CURVE ( 'NONE', #23668, #8314, #13054, .T. ) ;
#19995 = ORIENTED_EDGE ( 'NONE', *, *, #36619, .F. ) ;
#19996 = DIRECTION ( 'NONE',  ( 0.007781995580012662783, 0.000000000000000000, -0.9999697198139514409 ) ) ;
#19997 = ORIENTED_EDGE ( 'NONE', *, *, #50487, .T. ) ;
#19998 = ADVANCED_FACE ( 'NONE', ( #34358 ), #20994, .F. ) ;
#19999 = EDGE_CURVE ( 'NONE', #35810, #3699, #51662, .T. ) ;
#20000 = VERTEX_POINT ( 'NONE', #17891 ) ;
#20001 = EDGE_LOOP ( 'NONE', ( #7593, #34366, #14298, #8148, #3451 ) ) ;
#20002 = ORIENTED_EDGE ( 'NONE', *, *, #9836, .T. ) ;
#20003 = VERTEX_POINT ( 'NONE', #12506 ) ;
#20004 = CARTESIAN_POINT ( 'NONE',  ( -18.29747203306047609, -0.1191753592594177458, 14.03778604627889059 ) ) ;
#20005 = ORIENTED_EDGE ( 'NONE', *, *, #42701, .T. ) ;
#20006 = AXIS2_PLACEMENT_3D ( 'NONE', #24590, #32576, #45915 ) ;
#20007 = EDGE_LOOP ( 'NONE', ( #47045, #54136, #2427, #4044 ) ) ;
#20008 = DIRECTION ( 'NONE',  ( 0.9999697198139515519, 0.000000000000000000, 0.007781995580013368816 ) ) ;
#20009 = ORIENTED_EDGE ( 'NONE', *, *, #46120, .F. ) ;
#20010 = EDGE_LOOP ( 'NONE', ( #52842, #17034, #31832, #39819 ) ) ;
#20011 = CARTESIAN_POINT ( 'NONE',  ( -12.08693257711994384, -0.03228989815065527735, 1.575265987285825675 ) ) ;
#20012 = LINE ( 'NONE', #24014, #39384 ) ;
#20013 = CARTESIAN_POINT ( 'NONE',  ( -22.40478740399063895, 0.000000000000000000, 5.384712028983816623 ) ) ;
#20014 = DIRECTION ( 'NONE',  ( -0.5449076811759708816, 0.6444004775717707689, 0.5364919789714475140 ) ) ;
#20015 = CARTESIAN_POINT ( 'NONE',  ( -12.80458192191714595, 0.000000000000000000, 11.86454056839041726 ) ) ;
#20016 = EDGE_LOOP ( 'NONE', ( #29216, #45049, #9955, #5814 ) ) ;
#20017 = ORIENTED_EDGE ( 'NONE', *, *, #30411, .F. ) ;
#20018 = VECTOR ( 'NONE', #29826, 999.9999999999998863 ) ;
#20019 = CARTESIAN_POINT ( 'NONE',  ( 0.000000000000000000, 2.000000000000000000, 0.000000000000000000 ) ) ;
#20020 = DIRECTION ( 'NONE',  ( 0.007781995580012663651, -3.146120232559066537E-19, -0.9999697198139514409 ) ) ;
#20021 = ADVANCED_FACE ( 'NONE', ( #16747 ), #12207, .F. ) ;
#20022 = AXIS2_PLACEMENT_3D ( 'NONE', #5670, #37166, #1947 ) ;
#20023 = CARTESIAN_POINT ( 'NONE',  ( 2.072287782118878319, 0.000000000000000000, -2.950529333540147015 ) ) ;
#20024 = CARTESIAN_POINT ( 'NONE',  ( 2.072287782118878319, 0.000000000000000000, -2.950529333540147015 ) ) ;
#20025 = EDGE_CURVE ( 'NONE', #156, #21894, #21837, .T. ) ;
#20026 = PLANE ( 'NONE',  #28580 ) ;
#20027 = CARTESIAN_POINT ( 'NONE',  ( -19.45503627000849889, 0.000000000000000000, 7.556996783084074742 ) ) ;
#20028 = ORIENTED_EDGE ( 'NONE', *, *, #5021, .F. ) ;
#20029 = PLANE ( 'NONE',  #4778 ) ;
#20030 = ORIENTED_EDGE ( 'NONE', *, *, #42046, .F. ) ;
#20031 = B_SPLINE_CURVE_WITH_KNOTS ( 'NONE', 1,
 ( #21648, #38960 ),
 .UNSPECIFIED., .F., .F.,
 ( 2, 2 ),
 ( 0.000000000000000000, 0.0006430183911724572481 ),
 .UNSPECIFIED. ) ;
#20032 = FACE_OUTER_BOUND ( 'NONE', #45426, .T. ) ;
#20033 = LINE ( 'NONE', #11545, #55042 ) ;
#20034 = DIRECTION ( 'NONE',  ( -0.5449076811759708816, 0.6444004775717707689, 0.5364919789714475140 ) ) ;
#20035 = EDGE_CURVE ( 'NONE', #15181, #21588, #38316, .T. ) ;
#20036 = FACE_OUTER_BOUND ( 'NONE', #8439, .T. ) ;
#20037 = DIRECTION ( 'NONE',  ( 0.007781995580012662783, 0.000000000000000000, -0.9999697198139514409 ) ) ;
#20038 = ORIENTED_EDGE ( 'NONE', *, *, #31540, .T. ) ;
#20039 = VERTEX_POINT ( 'NONE', #8226 ) ;
#20040 = DIRECTION ( 'NONE',  ( -0.3620778797217455991, 0.000000000000000000, -0.9321478471874540261 ) ) ;
#20041 = CARTESIAN_POINT ( 'NONE',  ( -1.905187828007888884, 6.291258001618519557, 3.958413228513044668 ) ) ;
#20042 = LINE ( 'NONE', #54409, #16086 ) ;
#20043 = AXIS2_PLACEMENT_3D ( 'NONE', #34645, #56234, #51966 ) ;
#20044 = VECTOR ( 'NONE', #7597, 999.9999999999998863 ) ;
#20045 = CARTESIAN_POINT ( 'NONE',  ( 0.000000000000000000, 0.000000000000000000, 0.000000000000000000 ) ) ;
#20046 = CARTESIAN_POINT ( 'NONE',  ( -16.02024972601142494, 0.000000000000000000, 7.111732312921445143 ) ) ;
#20047 = DIRECTION ( 'NONE',  ( -0.7660212471507179544, -0.6427876096865405842, -0.005961354470445141482 ) ) ;
#20048 = CARTESIAN_POINT ( 'NONE',  ( -13.61044419115797410, -0.1159828484229804557, 8.505132312139858541 ) ) ;
#20049 = CARTESIAN_POINT ( 'NONE',  ( -58.00000000000000711, -9.000000000000000000, 7.102951435054649637E-15 ) ) ;
#20050 = LINE ( 'NONE', #55541, #26505 ) ;
#20051 = EDGE_CURVE ( 'NONE', #39913, #15552, #25541, .T. ) ;
#20052 = ADVANCED_FACE ( 'NONE', ( #43169 ), #17292, .F. ) ;
#20053 = ORIENTED_EDGE ( 'NONE', *, *, #11027, .F. ) ;
#20054 = EDGE_CURVE ( 'NONE', #42137, #2673, #47701, .T. ) ;
#20055 = EDGE_CURVE ( 'NONE', #45226, #33224, #816, .T. ) ;
#20056 = AXIS2_PLACEMENT_3D ( 'NONE', #1148, #17946, #6011 ) ;
#20057 = ORIENTED_EDGE ( 'NONE', *, *, #18198, .F. ) ;
#20058 = ORIENTED_EDGE ( 'NONE', *, *, #34482, .T. ) ;
#20059 = ORIENTED_EDGE ( 'NONE', *, *, #19291, .T. ) ;
#20060 = ORIENTED_EDGE ( 'NONE', *, *, #13424, .F. ) ;
#20061 = CARTESIAN_POINT ( 'NONE',  ( -16.34593356761463667, -3.432230869623162928, 3.121130690641215732 ) ) ;
#20062 = CARTESIAN_POINT ( 'NONE',  ( -31.72626587586518099, 0.000000000000000000, 9.005490826201270949 ) ) ;
#20063 = DIRECTION ( 'NONE',  ( -0.005961354470445682716, -0.6427876096865404731, 0.7660212471507180654 ) ) ;
#20064 = EDGE_LOOP ( 'NONE', ( #1592, #11366, #8408, #9658 ) ) ;
#20065 = ORIENTED_EDGE ( 'NONE', *, *, #44506, .T. ) ;
#20066 = ORIENTED_EDGE ( 'NONE', *, *, #21152, .T. ) ;
#20067 = CARTESIAN_POINT ( 'NONE',  ( -15.51131483200478201, 1.095915999411505526, 2.672087720579162884 ) ) ;
#20068 = ORIENTED_EDGE ( 'NONE', *, *, #53108, .F. ) ;
#20069 = EDGE_CURVE ( 'NONE', #32592, #3505, #44824, .T. ) ;
#20070 = CARTESIAN_POINT ( 'NONE',  ( -66.85871239793839038, -9.361568451089064880, 4.869406872008419818 ) ) ;
#20071 = CARTESIAN_POINT ( 'NONE',  ( -16.53317331066696383, 0.000000000000000000, 13.31285208727739899 ) ) ;
#20072 = DIRECTION ( 'NONE',  ( 0.7660212471507180654, -0.6427876096865404731, 0.005961354470445141482 ) ) ;
#20073 = VERTEX_POINT ( 'NONE', #22434 ) ;
#20074 = CARTESIAN_POINT ( 'NONE',  ( -8.860905869600903983, 1.712176620043476140E-14, 2.600000000000000089 ) ) ;
#20075 = EDGE_LOOP ( 'NONE', ( #44222, #55075, #26109, #38362, #8284, #28341, #45302, #31079, #35192, #7435, #10938, #51437, #614, #1180, #51913, #44400, #54425, #5864, #34421, #3739, #23826, #945, #19037, #9812, #44459, #42235, #54967 ) ) ;
#20076 = VECTOR ( 'NONE', #52168, 1000.000000000000227 ) ;
#20077 = CARTESIAN_POINT ( 'NONE',  ( -19.69569380384165669, -0.1191753592594177458, 14.58090286586150697 ) ) ;
#20078 = FACE_OUTER_BOUND ( 'NONE', #52987, .T. ) ;
#20079 = CARTESIAN_POINT ( 'NONE',  ( 2.072287782118878319, 0.000000000000000000, -2.950529333540147015 ) ) ;
#20080 = DIRECTION ( 'NONE',  ( 0.6427681459581294776, -0.7660444431189769032, 0.005002170337467562802 ) ) ;
#20081 = AXIS2_PLACEMENT_3D ( 'NONE', #48959, #44994, #2068 ) ;
#20082 = LINE ( 'NONE', #24362, #25903 ) ;
#20083 = CARTESIAN_POINT ( 'NONE',  ( -16.06709938707323460, 0.000000000000000000, 13.13181314741652628 ) ) ;
#20084 = CARTESIAN_POINT ( 'NONE',  ( -17.46532115785441519, 0.000000000000000000, 13.67492996699914265 ) ) ;
#20085 = DIRECTION ( 'NONE',  ( 0.7660212471507180654, -0.6427876096865404731, 0.005961354470445141482 ) ) ;
#20086 = PLANE ( 'NONE',  #9351 ) ;
#20087 = ORIENTED_EDGE ( 'NONE', *, *, #29162, .F. ) ;
#20088 = DIRECTION ( 'NONE',  ( 0.6427681459581294776, -0.7660444431189769032, 0.005002170337467562802 ) ) ;
#20089 = ORIENTED_EDGE ( 'NONE', *, *, #19929, .T. ) ;
#20090 = FACE_OUTER_BOUND ( 'NONE', #24764, .T. ) ;
#20091 = CARTESIAN_POINT ( 'NONE',  ( -18.54926312204414174, 1.905425754524005200, 7.213613129226924769 ) ) ;
#20092 = DIRECTION ( 'NONE',  ( 0.000000000000000000, -0.000000000000000000, -1.000000000000000000 ) ) ;
#20093 = EDGE_CURVE ( 'NONE', #23151, #50536, #5943, .T. ) ;
#20094 = LINE ( 'NONE', #32890, #5106 ) ;
#20095 = PLANE ( 'NONE',  #44913 ) ;
#20096 = VECTOR ( 'NONE', #54049, 999.9999999999998863 ) ;
#20097 = DIRECTION ( 'NONE',  ( 0.007781995580012663651, -3.146120232559066537E-19, -0.9999697198139514409 ) ) ;
#20098 = ORIENTED_EDGE ( 'NONE', *, *, #54706, .T. ) ;
#20099 = DIRECTION ( 'NONE',  ( 0.9999697198139515519, 0.000000000000000000, 0.007781995580013368816 ) ) ;
#20100 = LINE ( 'NONE', #32622, #48394 ) ;
#20101 = DIRECTION ( 'NONE',  ( 0.5364919789714477361, 0.6444004775717706579, 0.5449076811759711036 ) ) ;
#20102 = LINE ( 'NONE', #33208, #52703 ) ;
#20103 = CARTESIAN_POINT ( 'NONE',  ( -11.22505254250097906, -0.1166911823299084244, 1.141818036232515876 ) ) ;
#20104 = ADVANCED_FACE ( 'NONE', ( #48225 ), #14190, .F. ) ;
#20105 = CARTESIAN_POINT ( 'NONE',  ( 2.072287782118878319, 0.000000000000000000, -2.950529333540147015 ) ) ;
#20106 = LINE ( 'NONE', #6255, #42971 ) ;
#20107 = EDGE_CURVE ( 'NONE', #15058, #38157, #5639, .T. ) ;
#20108 = DIRECTION ( 'NONE',  ( 0.005002170337468016433, -0.7660444431189770143, -0.6427681459581293666 ) ) ;
#20109 = EDGE_CURVE ( 'NONE', #36639, #3399, #22965, .T. ) ;
#20110 = LINE ( 'NONE', #51060, #22902 ) ;
#20111 = ORIENTED_EDGE ( 'NONE', *, *, #34582, .T. ) ;
#20112 = PLANE ( 'NONE',  #25829 ) ;
#20113 = FACE_OUTER_BOUND ( 'NONE', #23396, .T. ) ;
#20114 = ORIENTED_EDGE ( 'NONE', *, *, #7771, .T. ) ;
#20115 = CARTESIAN_POINT ( 'NONE',  ( -12.70458494993575194, -0.1191753592594197858, 11.86531876794841978 ) ) ;
#20116 = FACE_OUTER_BOUND ( 'NONE', #248, .T. ) ;
#20117 = EDGE_CURVE ( 'NONE', #1131, #46770, #22683, .T. ) ;
#20118 = VECTOR ( 'NONE', #29359, 999.9999999999998863 ) ;
#20119 = VECTOR ( 'NONE', #11919, 1000.000000000000227 ) ;
#20120 = ORIENTED_EDGE ( 'NONE', *, *, #29785, .T. ) ;
#20121 = EDGE_CURVE ( 'NONE', #5026, #18137, #45124, .T. ) ;
#20122 = VERTEX_POINT ( 'NONE', #49367 ) ;
#20123 = DIRECTION ( 'NONE',  ( 0.5364919789714477361, 0.6444004775717706579, 0.5449076811759711036 ) ) ;
#20124 = EDGE_CURVE ( 'NONE', #4731, #27276, #18988, .T. ) ;
#20125 = ORIENTED_EDGE ( 'NONE', *, *, #56174, .T. ) ;
#20126 = VERTEX_POINT ( 'NONE', #6225 ) ;
#20127 = AXIS2_PLACEMENT_3D ( 'NONE', #53430, #48620, #31587 ) ;
#20128 = ORIENTED_EDGE ( 'NONE', *, *, #32052, .F. ) ;
#20129 = CARTESIAN_POINT ( 'NONE',  ( -19.60990026154428278, 0.000000000000000000, 4.498472333781370125 ) ) ;
#20130 = CARTESIAN_POINT ( 'NONE',  ( -11.40636015113596180, 0.000000000000000000, 11.32142374880780089 ) ) ;
#20131 = DIRECTION ( 'NONE',  ( 0.007781995580012662783, 0.000000000000000000, -0.9999697198139514409 ) ) ;
#20132 = ADVANCED_FACE ( 'NONE', ( #52507 ), #53074, .F. ) ;
#20133 = ORIENTED_EDGE ( 'NONE', *, *, #37680, .T. ) ;
#20134 = VECTOR ( 'NONE', #19541, 1000.000000000000227 ) ;
#20135 = VERTEX_POINT ( 'NONE', #18418 ) ;
#20136 = ADVANCED_FACE ( 'NONE', ( #10483 ), #31773, .F. ) ;
#20137 = CARTESIAN_POINT ( 'NONE',  ( -67.45463423721670893, 0.000000000000000000, 6.901237005686192028 ) ) ;
#20138 = CARTESIAN_POINT ( 'NONE',  ( -16.11361633748963129, 1.257817950434005683, 2.900876559667310950 ) ) ;
#20139 = ORIENTED_EDGE ( 'NONE', *, *, #46040, .F. ) ;
#20140 = DIRECTION ( 'NONE',  ( -0.7660212471507179544, -0.6427876096865405842, -0.005961354470445141482 ) ) ;
#20141 = ORIENTED_EDGE ( 'NONE', *, *, #26754, .T. ) ;
#20142 = LINE ( 'NONE', #53416, #23966 ) ;
#20143 = CARTESIAN_POINT ( 'NONE',  ( -9.942607371508632497, 0.000000000000000000, 2.357713023554631970 ) ) ;
#20144 = ORIENTED_EDGE ( 'NONE', *, *, #35136, .T. ) ;
#20145 = CARTESIAN_POINT ( 'NONE',  ( -20.71168680238113424, 4.981562823951510843, 13.10203691794590419 ) ) ;
#20146 = VECTOR ( 'NONE', #49552, 1000.000000000000227 ) ;
#20147 = LINE ( 'NONE', #19323, #47224 ) ;
#20148 = ORIENTED_EDGE ( 'NONE', *, *, #49035, .F. ) ;
#20149 = DIRECTION ( 'NONE',  ( 0.5449076811759707706, 0.6444004775717708799, -0.5364919789714476250 ) ) ;
#20150 = PRESENTATION_STYLE_ASSIGNMENT (( #15099 ) ) ;
#20151 = VECTOR ( 'NONE', #40412, 999.9999999999998863 ) ;
#20152 = FACE_OUTER_BOUND ( 'NONE', #34001, .T. ) ;
#20153 = ORIENTED_EDGE ( 'NONE', *, *, #34491, .T. ) ;
#20154 = VECTOR ( 'NONE', #27539, 1000.000000000000000 ) ;
#20155 = AXIS2_PLACEMENT_3D ( 'NONE', #36898, #37153, #50202 ) ;
#20156 = LINE ( 'NONE', #41491, #22866 ) ;
#20157 = CARTESIAN_POINT ( 'NONE',  ( -3.486932065698848504, -6.851436116247921149, -1.863930744634968883 ) ) ;
#20158 = CARTESIAN_POINT ( 'NONE',  ( -23.33693525117809386, 0.000000000000000000, 5.746789908705562944 ) ) ;
#20159 = EDGE_CURVE ( 'NONE', #428, #11699, #43981, .T. ) ;
#20160 = DIRECTION ( 'NONE',  ( 0.9999697198139515519, 0.000000000000000000, 0.007781995580013368816 ) ) ;
#20161 = CARTESIAN_POINT ( 'NONE',  ( -12.52600435597107342, 0.000000000000000000, 1.768270304842026963 ) ) ;
#20162 = LINE ( 'NONE', #3693, #51484 ) ;
#20163 = VECTOR ( 'NONE', #47887, 1000.000000000000114 ) ;
#20164 = CARTESIAN_POINT ( 'NONE',  ( -68.66066644775141015, -11.58131332038088246, -6.967005367358785506 ) ) ;
#20165 = VECTOR ( 'NONE', #11249, 1000.000000000000227 ) ;
#20166 = ORIENTED_EDGE ( 'NONE', *, *, #11402, .F. ) ;
#20167 = DIRECTION ( 'NONE',  ( -0.005961354470445682716, -0.6427876096865404731, 0.7660212471507180654 ) ) ;
#20168 = CARTESIAN_POINT ( 'NONE',  ( -12.54480507611877194, 0.000000000000000000, 4.184122468351399782 ) ) ;
#20169 = DIRECTION ( 'NONE',  ( 0.007781995580012663651, 0.000000000000000000, -0.9999697198139515519 ) ) ;
#20170 = VERTEX_POINT ( 'NONE', #49079 ) ;
#20171 = LINE ( 'NONE', #37222, #12069 ) ;
#20172 = CARTESIAN_POINT ( 'NONE',  ( -13.10866074538325243, -0.1191753592594186895, 4.079731385043992020 ) ) ;
#20173 = CARTESIAN_POINT ( 'NONE',  ( -25.20123094555300369, 0.000000000000000000, 6.470945668149052032 ) ) ;
#20174 = AXIS2_PLACEMENT_3D ( 'NONE', #20015, #33938, #12641 ) ;
#20175 = AXIS2_PLACEMENT_3D ( 'NONE', #37536, #54856, #29019 ) ;
#20176 = DIRECTION ( 'NONE',  ( -0.005961354470445682716, -0.6427876096865404731, 0.7660212471507180654 ) ) ;
#20177 = ADVANCED_FACE ( 'NONE', ( #40842 ), #30917, .F. ) ;
#20178 = CARTESIAN_POINT ( 'NONE',  ( -55.54283117668188652, 6.653082554758466216, 1.248231344413326394 ) ) ;
#20179 = ORIENTED_EDGE ( 'NONE', *, *, #11641, .T. ) ;
#20180 = ORIENTED_EDGE ( 'NONE', *, *, #43279, .T. ) ;
#20181 = DIRECTION ( 'NONE',  ( -0.5364919789714478471, 0.6444004775717705469, -0.5449076811759709926 ) ) ;
#20182 = AXIS2_PLACEMENT_3D ( 'NONE', #39986, #53885, #27802 ) ;
#20183 = CARTESIAN_POINT ( 'NONE',  ( -10.90924386075947972, 0.000000000000000000, 7.151507342369550990 ) ) ;
#20184 = CARTESIAN_POINT ( 'NONE',  ( 2.072287782118878319, 0.000000000000000000, -2.950529333540147015 ) ) ;
#20185 = ORIENTED_EDGE ( 'NONE', *, *, #37145, .T. ) ;
#20186 = EDGE_CURVE ( 'NONE', #28807, #11287, #5105, .T. ) ;
#20187 = DIRECTION ( 'NONE',  ( -0.2588190451025212946, -0.9659258262890680902, 0.000000000000000000 ) ) ;
#20188 = VECTOR ( 'NONE', #54473, 1000.000000000000227 ) ;
#20189 = VERTEX_POINT ( 'NONE', #9646 ) ;
#20190 = PLANE ( 'NONE',  #10246 ) ;
#20191 = ADVANCED_FACE ( 'NONE', ( #26966 ), #44279, .F. ) ;
#20192 = ORIENTED_EDGE ( 'NONE', *, *, #11210, .F. ) ;
#20193 = ORIENTED_EDGE ( 'NONE', *, *, #54532, .F. ) ;
#20194 = CARTESIAN_POINT ( 'NONE',  ( -14.96058358053937454, -0.1134144341942091572, 2.592825150574666448 ) ) ;
#20195 = VECTOR ( 'NONE', #30428, 999.9999999999998863 ) ;
#20196 = CARTESIAN_POINT ( 'NONE',  ( -12.80458192191714595, 0.000000000000000000, 11.86454056839041726 ) ) ;
#20197 = CARTESIAN_POINT ( 'NONE',  ( -21.47419595591918906, 0.000000000000000000, 5.222628093224860102 ) ) ;
#20198 = ORIENTED_EDGE ( 'NONE', *, *, #40271, .F. ) ;
#20199 = VECTOR ( 'NONE', #54448, 1000.000000000000227 ) ;
#20200 = EDGE_CURVE ( 'NONE', #29054, #12905, #18724, .T. ) ;
#20201 = CIRCLE ( 'NONE', #10212, 2.749999999999998224 ) ;
#20202 = CARTESIAN_POINT ( 'NONE',  ( -15.54411661514920695, 0.000000000000000000, 5.638109411658397185 ) ) ;
#20203 = ORIENTED_EDGE ( 'NONE', *, *, #1843, .F. ) ;
#20204 = ORIENTED_EDGE ( 'NONE', *, *, #41803, .T. ) ;
#20205 = EDGE_CURVE ( 'NONE', #37323, #42326, #49904, .T. ) ;
#20206 = VECTOR ( 'NONE', #47825, 999.9999999999998863 ) ;
#20207 = ORIENTED_EDGE ( 'NONE', *, *, #52309, .F. ) ;
#20208 = LINE ( 'NONE', #14575, #53112 ) ;
#20209 = VECTOR ( 'NONE', #24445, 999.9999999999998863 ) ;
#20210 = PLANE ( 'NONE',  #45784 ) ;
#20211 = ORIENTED_EDGE ( 'NONE', *, *, #28097, .F. ) ;
#20212 = LINE ( 'NONE', #11968, #17568 ) ;
#20213 = ORIENTED_EDGE ( 'NONE', *, *, #33762, .T. ) ;
#20214 = LINE ( 'NONE', #49780, #29461 ) ;
#20215 = CARTESIAN_POINT ( 'NONE',  ( -17.46532115785441519, 0.000000000000000000, 13.67492996699914265 ) ) ;
#20216 = VERTEX_POINT ( 'NONE', #6483 ) ;
#20218 = VECTOR ( 'NONE', #30317, 1000.000000000000227 ) ;
#20217 = CARTESIAN_POINT ( 'NONE',  ( -15.72637881786665837, 1.905425754524006532, 2.729798276854666028 ) ) ;
#20219 = EDGE_LOOP ( 'NONE', ( #31014, #9806, #49123, #31996 ) ) ;
#20220 = VECTOR ( 'NONE', #33432, 999.9999999999998863 ) ;
#20221 = DIRECTION ( 'NONE',  ( -0.5364919789714478471, 0.6444004775717705469, -0.5449076811759709926 ) ) ;
#20222 = LINE ( 'NONE', #6920, #20228 ) ;
#20223 = DIRECTION ( 'NONE',  ( -0.6427681459581293666, -0.7660444431189770143, -0.005002170337467561935 ) ) ;
#20224 = CARTESIAN_POINT ( 'NONE',  ( -16.76389984325721727, 0.000000000000000000, 8.952605404790253019 ) ) ;
#20225 = DIRECTION ( 'NONE',  ( 0.007781995580012662783, 0.000000000000000000, -0.9999697198139514409 ) ) ;
#20226 = ORIENTED_EDGE ( 'NONE', *, *, #27877, .F. ) ;
#20227 = ADVANCED_FACE ( 'NONE', ( #50494 ), #46479, .F. ) ;
#20228 = VECTOR ( 'NONE', #24774, 999.9999999999998863 ) ;
#20229 = EDGE_LOOP ( 'NONE', ( #56093, #49793, #41533, #42548 ) ) ;
#20230 = LINE ( 'NONE', #42403, #28251 ) ;
#20231 = CARTESIAN_POINT ( 'NONE',  ( -67.91822744485311603, -9.430911930847621250, 7.468591521940118660 ) ) ;
#20232 = EDGE_CURVE ( 'NONE', #39606, #2632, #6768, .T. ) ;
#20233 = VECTOR ( 'NONE', #9454, 999.9999999999998863 ) ;
#20234 = CARTESIAN_POINT ( 'NONE',  ( -69.58726886377220922, 0.1328949963053452921, 6.962762944060566284 ) ) ;
#20235 = CARTESIAN_POINT ( 'NONE',  ( -24.26986129792355129, -0.1191753592594197858, 6.208864760408702388 ) ) ;
#20236 = LINE ( 'NONE', #19406, #32443 ) ;
#20237 = DIRECTION ( 'NONE',  ( 0.5449076811759707706, 0.6444004775717708799, -0.5364919789714476250 ) ) ;
#20238 = VERTEX_POINT ( 'NONE', #50188 ) ;
#20239 = EDGE_CURVE ( 'NONE', #36106, #55458, #23789, .T. ) ;
#20240 = CARTESIAN_POINT ( 'NONE',  ( -28.92982233430281980, 0.000000000000000000, 7.919257187036034651 ) ) ;
#20241 = PLANE ( 'NONE',  #12361 ) ;
#20242 = ORIENTED_EDGE ( 'NONE', *, *, #49469, .F. ) ;
#20244 = LINE ( 'NONE', #24504, #13889 ) ;
#20243 = VECTOR ( 'NONE', #19739, 1000.000000000000000 ) ;
#20245 = DIRECTION ( 'NONE',  ( -0.005961354470445682716, -0.6427876096865404731, 0.7660212471507180654 ) ) ;
#20246 = VERTEX_POINT ( 'NONE', #3044 ) ;
#20247 = EDGE_CURVE ( 'NONE', #10472, #45226, #45950, .T. ) ;
#20248 = EDGE_CURVE ( 'NONE', #52686, #46703, #24088, .T. ) ;
#20249 = EDGE_CURVE ( 'NONE', #52604, #4570, #33176, .T. ) ;
#20250 = AXIS2_PLACEMENT_3D ( 'NONE', #3199, #33576, #20533 ) ;
#20251 = VECTOR ( 'NONE', #28796, 999.9999999999998863 ) ;
#20252 = DIRECTION ( 'NONE',  ( -0.005961354470445682716, -0.6427876096865404731, 0.7660212471507180654 ) ) ;
#20254 = DIRECTION ( 'NONE',  ( -0.5364919789714478471, 0.6444004775717705469, -0.5449076811759709926 ) ) ;
#20253 = B_SPLINE_CURVE_WITH_KNOTS ( 'NONE', 3,
 ( #43799, #47220, #4630, #35305 ),
 .UNSPECIFIED., .F., .F.,
 ( 4, 4 ),
 ( 0.0001107606836644239992, 0.0004080808962162847881 ),
 .UNSPECIFIED. ) ;
#20255 = DIRECTION ( 'NONE',  ( -0.9999697198139514409, -0.000000000000000000, -0.007781995580013368816 ) ) ;
#20256 = DIRECTION ( 'NONE',  ( -0.005961354470445682716, -0.6427876096865404731, 0.7660212471507180654 ) ) ;
#20257 = FACE_OUTER_BOUND ( 'NONE', #4028, .T. ) ;
#20258 = ORIENTED_EDGE ( 'NONE', *, *, #27144, .F. ) ;
#20259 = AXIS2_PLACEMENT_3D ( 'NONE', #37187, #54489, #32925 ) ;
#20260 = VECTOR ( 'NONE', #51686, 1000.000000000000227 ) ;
#20261 = VERTEX_POINT ( 'NONE', #19821 ) ;
#20262 = DIRECTION ( 'NONE',  ( 0.9999697198139515519, 0.000000000000000000, 0.007781995580013368816 ) ) ;
#20263 = DIRECTION ( 'NONE',  ( 0.000000000000000000, -0.000000000000000000, -1.000000000000000000 ) ) ;
#20264 = CARTESIAN_POINT ( 'NONE',  ( -18.66354898467281132, 0.000000000000000000, 14.21960318569776582 ) ) ;
#20265 = CARTESIAN_POINT ( 'NONE',  ( -17.93139508144814442, 0.000000000000000000, 13.85596890686001537 ) ) ;
#20266 = DIRECTION ( 'NONE',  ( 0.000000000000000000, -0.000000000000000000, -1.000000000000000000 ) ) ;
#20267 = ADVANCED_FACE ( 'NONE', ( #36584 ), #28064, .F. ) ;
#20268 = DIRECTION ( 'NONE',  ( 0.005002170337468016433, -0.7660444431189770143, -0.6427681459581293666 ) ) ;
#20269 = ORIENTED_EDGE ( 'NONE', *, *, #28418, .T. ) ;
#20270 = DIRECTION ( 'NONE',  ( 0.000000000000000000, -0.000000000000000000, -1.000000000000000000 ) ) ;
#20271 = EDGE_CURVE ( 'NONE', #547, #6826, #11297, .T. ) ;
#20272 = CARTESIAN_POINT ( 'NONE',  ( -16.06709938707323460, 0.000000000000000000, 13.13181314741652628 ) ) ;
#20273 = PLANE ( 'NONE',  #18774 ) ;
#20274 = ORIENTED_EDGE ( 'NONE', *, *, #46702, .F. ) ;
#20275 = VECTOR ( 'NONE', #4033, 1000.000000000000000 ) ;
#20276 = EDGE_CURVE ( 'NONE', #27953, #47622, #19543, .T. ) ;
#20277 = CARTESIAN_POINT ( 'NONE',  ( -11.91804826722769306, 25.86399001096056338, -4.999999999999888978 ) ) ;
#20278 = CARTESIAN_POINT ( 'NONE',  ( -13.27065584551087163, 0.000000000000000000, 12.04557950825129176 ) ) ;
#20279 = AXIS2_PLACEMENT_3D ( 'NONE', #32874, #37407, #54727 ) ;
#20280 = CARTESIAN_POINT ( 'NONE',  ( -14.66887761629205222, 0.000000000000000000, 12.58869632783390990 ) ) ;
#20281 = ORIENTED_EDGE ( 'NONE', *, *, #37400, .F. ) ;
#20282 = EDGE_CURVE ( 'NONE', #35036, #15384, #41413, .T. ) ;
#20283 = PLANE ( 'NONE',  #7789 ) ;
#20284 = VECTOR ( 'NONE', #55580, 999.9999999999998863 ) ;
#20285 = VERTEX_POINT ( 'NONE', #24357 ) ;
#20286 = EDGE_CURVE ( 'NONE', #18631, #31141, #32601, .T. ) ;
#20287 = VERTEX_POINT ( 'NONE', #3354 ) ;
#20288 = ORIENTED_EDGE ( 'NONE', *, *, #19581, .F. ) ;
#20289 = ORIENTED_EDGE ( 'NONE', *, *, #25722, .F. ) ;
#20290 = VECTOR ( 'NONE', #54491, 1000.000000000000000 ) ;
#20291 = CARTESIAN_POINT ( 'NONE',  ( 1.710209902397132220, 0.000000000000000000, -3.882677180727601041 ) ) ;
#20292 = VERTEX_POINT ( 'NONE', #54441 ) ;
#20293 = VECTOR ( 'NONE', #43177, 1000.000000000000114 ) ;
#20294 = VERTEX_POINT ( 'NONE', #15541 ) ;
#20295 = PLANE ( 'NONE',  #463 ) ;
#20296 = ORIENTED_EDGE ( 'NONE', *, *, #10970, .F. ) ;
#20297 = ORIENTED_EDGE ( 'NONE', *, *, #25329, .F. ) ;
#20298 = AXIS2_PLACEMENT_3D ( 'NONE', #41449, #15572, #46233 ) ;
#20299 = AXIS2_PLACEMENT_3D ( 'NONE', #1265, #35643, #27389 ) ;
#20300 = DIRECTION ( 'NONE',  ( 0.000000000000000000, -1.000000000000000000, 0.000000000000000000 ) ) ;
#20301 = DIRECTION ( 'NONE',  ( 0.005002170337468016433, -0.7660444431189770143, -0.6427681459581293666 ) ) ;
#20302 = CARTESIAN_POINT ( 'NONE',  ( -12.13851405436063047, 0.000000000000000000, 11.68505802764555135 ) ) ;
#20303 = DIRECTION ( 'NONE',  ( -0.5364919789714478471, 0.6444004775717705469, -0.5449076811759709926 ) ) ;
#20304 = CARTESIAN_POINT ( 'NONE',  ( -12.75916928760797653, 0.000000000000000000, 6.029114585524220082 ) ) ;
#20305 = EDGE_LOOP ( 'NONE', ( #27861, #28608, #19654, #38462 ) ) ;
#20306 = VERTEX_POINT ( 'NONE', #32872 ) ;
#20307 = LINE ( 'NONE', #55235, #30335 ) ;
#20308 = CARTESIAN_POINT ( 'NONE',  ( -16.39273361182896238, -0.1191753592594177180, 8.116826738503332805 ) ) ;
#20309 = DIRECTION ( 'NONE',  ( -0.005002170337468016433, -0.7660444431189770143, 0.6427681459581293666 ) ) ;
#20310 = DIRECTION ( 'NONE',  ( 0.007781995580012663651, 0.000000000000000000, -0.9999697198139515519 ) ) ;
#20311 = VECTOR ( 'NONE', #47829, 999.9999999999998863 ) ;
#20312 = DIRECTION ( 'NONE',  ( -0.7660212471507179544, -0.6427876096865405842, -0.005961354470445141482 ) ) ;
#20313 = CARTESIAN_POINT ( 'NONE',  ( -10.39862210783386942, 0.000000000000000000, 1.246168002013329446 ) ) ;
#20314 = VERTEX_POINT ( 'NONE', #53893 ) ;
#20315 = CARTESIAN_POINT ( 'NONE',  ( -58.00000000000000711, 8.000000000000000000, 7.102951435054649637E-15 ) ) ;
#20316 = VECTOR ( 'NONE', #51486, 999.9999999999998863 ) ;
#20317 = ORIENTED_EDGE ( 'NONE', *, *, #15158, .F. ) ;
#20318 = EDGE_CURVE ( 'NONE', #40480, #20696, #41666, .T. ) ;
#20319 = EDGE_CURVE ( 'NONE', #12432, #14535, #2752, .T. ) ;
#20320 = CARTESIAN_POINT ( 'NONE',  ( -15.00578141713185332, -1.813211359398156919, 5.486475579755086152 ) ) ;
#20321 = CARTESIAN_POINT ( 'NONE',  ( -11.40636015113596180, 0.000000000000000000, 11.32142374880780089 ) ) ;
#20322 = CARTESIAN_POINT ( 'NONE',  ( -16.33317936670417225, 0.000000000000000000, 13.31440848639340224 ) ) ;
#20323 = LINE ( 'NONE', #10968, #26355 ) ;
#20324 = AXIS2_PLACEMENT_3D ( 'NONE', #27162, #5572, #5871 ) ;
#20325 = LINE ( 'NONE', #21473, #2336 ) ;
#20326 = ADVANCED_FACE ( 'NONE', ( #24927 ), #15014, .F. ) ;
#20327 = LINE ( 'NONE', #33408, #49505 ) ;
#20328 = ORIENTED_EDGE ( 'NONE', *, *, #50151, .F. ) ;
#20329 = EDGE_LOOP ( 'NONE', ( #28614, #24143, #32553, #1277 ) ) ;
#20330 = VECTOR ( 'NONE', #54711, 999.9999999999998863 ) ;
#20331 = CARTESIAN_POINT ( 'NONE',  ( -23.33693525117809386, 0.000000000000000000, 5.746789908705562944 ) ) ;
#20332 = LINE ( 'NONE', #37673, #459 ) ;
#20333 = CARTESIAN_POINT ( 'NONE',  ( -11.40636015113596180, 0.000000000000000000, 11.32142374880780089 ) ) ;
#20334 = VECTOR ( 'NONE', #24631, 1000.000000000000227 ) ;
#20335 = DIRECTION ( 'NONE',  ( 0.000000000000000000, -1.000000000000000000, 0.000000000000000000 ) ) ;
#20336 = CARTESIAN_POINT ( 'NONE',  ( -13.60203817727716391, -0.1191753592594181482, 7.769212505853626105 ) ) ;
#20337 = FACE_OUTER_BOUND ( 'NONE', #34687, .T. ) ;
#20338 = CARTESIAN_POINT ( 'NONE',  ( -13.96589990257885638, 0.000000000000000000, 7.666377821662226033 ) ) ;
#20339 = EDGE_CURVE ( 'NONE', #42669, #42711, #45370, .T. ) ;
#20340 = VECTOR ( 'NONE', #27130, 999.9999999999998863 ) ;
#20341 = VECTOR ( 'NONE', #2787, 999.9999999999998863 ) ;
#20342 = DIRECTION ( 'NONE',  ( 0.5364919789714477361, 0.6444004775717706579, 0.5449076811759711036 ) ) ;
#20343 = EDGE_CURVE ( 'NONE', #41698, #3615, #30612, .T. ) ;
#20344 = FACE_OUTER_BOUND ( 'NONE', #45782, .T. ) ;
#20345 = ORIENTED_EDGE ( 'NONE', *, *, #32481, .F. ) ;
#20346 = ADVANCED_FACE ( 'NONE', ( #43379 ), #8168, .F. ) ;
#20347 = EDGE_CURVE ( 'NONE', #23998, #42364, #51870, .T. ) ;
#20348 = AXIS2_PLACEMENT_3D ( 'NONE', #48161, #9010, #17821 ) ;
#20349 = ORIENTED_EDGE ( 'NONE', *, *, #32462, .F. ) ;
#20350 = VERTEX_POINT ( 'NONE', #47916 ) ;
#20351 = ORIENTED_EDGE ( 'NONE', *, *, #52270, .T. ) ;
#20352 = EDGE_CURVE ( 'NONE', #55206, #22415, #16980, .T. ) ;
#20353 = AXIS2_PLACEMENT_3D ( 'NONE', #18486, #30977, #39222 ) ;
#20354 = EDGE_LOOP ( 'NONE', ( #16016, #11590, #46836, #51120 ) ) ;
#20355 = DIRECTION ( 'NONE',  ( -0.000000000000000000, -0.000000000000000000, 1.000000000000000000 ) ) ;
#20356 = CARTESIAN_POINT ( 'NONE',  ( -18.29747203306047609, -0.1191753592594177458, 14.03778604627889059 ) ) ;
#20357 = EDGE_CURVE ( 'NONE', #44507, #42836, #47065, .T. ) ;
#20358 = DIRECTION ( 'NONE',  ( 0.9999697198139515519, 0.000000000000000000, 0.007781995580013368816 ) ) ;
#20359 = VECTOR ( 'NONE', #16467, 1000.000000000000227 ) ;
#20360 = ORIENTED_EDGE ( 'NONE', *, *, #3610, .F. ) ;
#20361 = VERTEX_POINT ( 'NONE', #21783 ) ;
#20362 = EDGE_CURVE ( 'NONE', #54876, #46454, #37990, .T. ) ;
#20363 = ORIENTED_EDGE ( 'NONE', *, *, #45910, .F. ) ;
#20364 = DIRECTION ( 'NONE',  ( 0.007781995580012663651, -3.146120232559066537E-19, -0.9999697198139514409 ) ) ;
#20365 = VERTEX_POINT ( 'NONE', #39101 ) ;
#20366 = VECTOR ( 'NONE', #183, 999.9999999999998863 ) ;
#20367 = CARTESIAN_POINT ( 'NONE',  ( -66.84374069725500078, -8.754700742360908450, -2.713115426954385789 ) ) ;
#20368 = VECTOR ( 'NONE', #25908, 1000.000000000000227 ) ;
#20369 = DIRECTION ( 'NONE',  ( 0.005961354470445682716, -0.6427876096865404731, -0.7660212471507180654 ) ) ;
#20370 = LINE ( 'NONE', #41935, #45886 ) ;
#20371 = ORIENTED_EDGE ( 'NONE', *, *, #45500, .F. ) ;
#20372 = CARTESIAN_POINT ( 'NONE',  ( -12.99219765192816212, 0.000000000000000000, 1.964648337036805081 ) ) ;
#20373 = VERTEX_POINT ( 'NONE', #46791 ) ;
#20374 = AXIS2_PLACEMENT_3D ( 'NONE', #30687, #3431, #33798 ) ;
#20375 = CARTESIAN_POINT ( 'NONE',  ( -13.19253370888792709, -1.327505506330656893, 3.985022539870387348 ) ) ;
#20376 = DIRECTION ( 'NONE',  ( 0.007781995580012663651, -3.146120232559066537E-19, -0.9999697198139514409 ) ) ;
#20377 = VECTOR ( 'NONE', #1821, 1000.000000000000114 ) ;
#20378 = DIRECTION ( 'NONE',  ( -0.7660212471507179544, -0.6427876096865405842, -0.005961354470445141482 ) ) ;
#20379 = AXIS2_PLACEMENT_3D ( 'NONE', #54071, #23669, #48703 ) ;
#20380 = DIRECTION ( 'NONE',  ( 0.007781995580012663651, -3.146120232559066537E-19, -0.9999697198139514409 ) ) ;
#20381 = LINE ( 'NONE', #3624, #22954 ) ;
#20382 = DIRECTION ( 'NONE',  ( 0.6427681459581294776, -0.7660444431189769032, 0.005002170337467562802 ) ) ;
#20383 = DIRECTION ( 'NONE',  ( 0.007781995580012663651, 0.000000000000000000, -0.9999697198139515519 ) ) ;
#20384 = LINE ( 'NONE', #2510, #4816 ) ;
#20385 = ORIENTED_EDGE ( 'NONE', *, *, #20724, .T. ) ;
#20386 = FACE_OUTER_BOUND ( 'NONE', #38282, .T. ) ;
#20387 = ORIENTED_EDGE ( 'NONE', *, *, #45732, .T. ) ;
#20388 = ADVANCED_FACE ( 'NONE', ( #51606 ), #34301, .F. ) ;
#20389 = DIRECTION ( 'NONE',  ( 0.007781995580012662783, 0.000000000000000000, -0.9999697198139514409 ) ) ;
#20390 = DIRECTION ( 'NONE',  ( 0.9999697198139515519, 0.000000000000000000, 0.007781995580013368816 ) ) ;
#20391 = DIRECTION ( 'NONE',  ( 0.5449076811759707706, 0.6444004775717708799, -0.5364919789714476250 ) ) ;
#20392 = LINE ( 'NONE', #38856, #53053 ) ;
#20393 = DIRECTION ( 'NONE',  ( 0.9999697198139515519, 0.000000000000000000, 0.007781995580013368816 ) ) ;
#20394 = ADVANCED_FACE ( 'NONE', ( #34013 ), #38547, .F. ) ;
#20395 = EDGE_CURVE ( 'NONE', #1256, #34545, #26317, .T. ) ;
#20396 = VECTOR ( 'NONE', #3071, 1000.000000000000227 ) ;
#20397 = DIRECTION ( 'NONE',  ( -0.9999697198139514409, -0.000000000000000000, -0.007781995580013368816 ) ) ;
#20398 = ORIENTED_EDGE ( 'NONE', *, *, #38700, .T. ) ;
#20399 = CARTESIAN_POINT ( 'NONE',  ( -18.76354595665420177, -0.1191753592594177458, 14.21882498613976331 ) ) ;
#20400 = CARTESIAN_POINT ( 'NONE',  ( -16.94664946618831181, 0.000000000000000000, 6.735190786127661866 ) ) ;
#20401 = LINE ( 'NONE', #8467, #30382 ) ;
#20402 = LINE ( 'NONE', #51054, #29110 ) ;
#20403 = VECTOR ( 'NONE', #40304, 1000.000000000000227 ) ;
#20404 = LINE ( 'NONE', #28661, #4236 ) ;
#20405 = CARTESIAN_POINT ( 'NONE',  ( 2.072287782118878319, 0.000000000000000000, -2.950529333540147015 ) ) ;
#20406 = AXIS2_PLACEMENT_3D ( 'NONE', #45440, #54257, #19051 ) ;
#20407 = CARTESIAN_POINT ( 'NONE',  ( -15.80720316891149757, 0.000000000000000000, 5.436055955043602061 ) ) ;
#20408 = CARTESIAN_POINT ( 'NONE',  ( -14.79423097067920168, 1.905425754524006532, 2.367720397132919707 ) ) ;
#20409 = DIRECTION ( 'NONE',  ( 0.5449076811759707706, 0.6444004775717708799, -0.5364919789714476250 ) ) ;
#20410 = EDGE_CURVE ( 'NONE', #40212, #940, #51336, .T. ) ;
#20411 = ORIENTED_EDGE ( 'NONE', *, *, #55186, .T. ) ;
#20412 = CARTESIAN_POINT ( 'NONE',  ( -16.36111902327085232, -0.1191753592594190780, 4.054420002667924905 ) ) ;
#20413 = VECTOR ( 'NONE', #18567, 999.9999999999998863 ) ;
#20414 = CARTESIAN_POINT ( 'NONE',  ( 2.072287782118878319, 0.000000000000000000, -2.950529333540147015 ) ) ;
#20415 = AXIS2_PLACEMENT_3D ( 'NONE', #55441, #29904, #20548 ) ;
#20416 = ORIENTED_EDGE ( 'NONE', *, *, #54945, .T. ) ;
#20417 = AXIS2_PLACEMENT_3D ( 'NONE', #32976, #15371, #19650 ) ;
#20418 = CARTESIAN_POINT ( 'NONE',  ( -18.29747203306047609, -0.1191753592594177458, 14.03778604627889059 ) ) ;
#20419 = FACE_OUTER_BOUND ( 'NONE', #42774, .T. ) ;
#20420 = AXIS2_PLACEMENT_3D ( 'NONE', #18746, #19839, #1938 ) ;
#20421 = EDGE_LOOP ( 'NONE', ( #5777, #52511, #48845, #35959, #56014, #42692, #1712, #42174, #27998, #27284, #19325, #27420, #6942, #6869, #35203, #22877, #38182, #38616, #29204, #11672, #47463, #53282, #34348, #8724, #27867, #35523, #20634, #10661, #44800, #46924, #42697, #54449, #21760, #18959, #55492, #38613, #6126, #39288, #47321, #33260, #33438, #26976, #45296, #39075, #54280, #22113, #33327, #53664, #10556 ) ) ;
#20422 = EDGE_LOOP ( 'NONE', ( #15468, #12611, #40058, #53882 ) ) ;
#20423 = CARTESIAN_POINT ( 'NONE',  ( -15.86710544311044302, 0.000000000000000000, 13.13336954653252953 ) ) ;
#20424 = EDGE_CURVE ( 'NONE', #40139, #35650, #4206, .T. ) ;
#20425 = VECTOR ( 'NONE', #25198, 999.9999999999998863 ) ;
#20426 = ORIENTED_EDGE ( 'NONE', *, *, #7163, .F. ) ;
#20427 = VECTOR ( 'NONE', #43511, 1000.000000000000227 ) ;
#20428 = ORIENTED_EDGE ( 'NONE', *, *, #46989, .T. ) ;
#20429 = ORIENTED_EDGE ( 'NONE', *, *, #45981, .T. ) ;
#20430 = EDGE_CURVE ( 'NONE', #27953, #52707, #16383, .T. ) ;
#20431 = DIRECTION ( 'NONE',  ( 0.000000000000000000, -0.000000000000000000, -1.000000000000000000 ) ) ;
#20432 = LINE ( 'NONE', #51389, #36908 ) ;
#20433 = CARTESIAN_POINT ( 'NONE',  ( -12.16414003897701690, -0.1134144341942073114, 1.506591511409430817 ) ) ;
#20434 = EDGE_LOOP ( 'NONE', ( #9325, #26943, #34352 ) ) ;
#20435 = ADVANCED_FACE ( 'NONE', ( #51023 ), #29768, .F. ) ;
#20436 = ORIENTED_EDGE ( 'NONE', *, *, #6705, .T. ) ;
#20437 = AXIS2_PLACEMENT_3D ( 'NONE', #28874, #37364, #3577 ) ;
#20438 = DIRECTION ( 'NONE',  ( 0.000000000000000000, -1.000000000000000000, 0.000000000000000000 ) ) ;
#20439 = CARTESIAN_POINT ( 'NONE',  ( -26.13415699229845757, -0.1191753592594197858, 6.933020519852192365 ) ) ;
#20440 = VECTOR ( 'NONE', #29387, 1000.000000000000114 ) ;
#20441 = ORIENTED_EDGE ( 'NONE', *, *, #9039, .F. ) ;
#20442 = CARTESIAN_POINT ( 'NONE',  ( -14.00280974873554030, 0.000000000000000000, 12.40921378708904044 ) ) ;
#20443 = EDGE_LOOP ( 'NONE', ( #38876, #12819, #2587, #54383 ) ) ;
#20444 = AXIS2_PLACEMENT_3D ( 'NONE', #45327, #37653, #32295 ) ;
#20445 = FACE_OUTER_BOUND ( 'NONE', #23068, .T. ) ;
#20446 = CARTESIAN_POINT ( 'NONE',  ( -25.98475788909843587, 17.60307238499724392, 4.611630842834720134 ) ) ;
#20447 = EDGE_CURVE ( 'NONE', #40382, #2633, #12135, .T. ) ;
#20448 = EDGE_LOOP ( 'NONE', ( #31883, #33357, #8065, #22340 ) ) ;
#20449 = CARTESIAN_POINT ( 'NONE',  ( -18.86354292863559579, 0.000000000000000000, 14.21804678658176080 ) ) ;
#20450 = VECTOR ( 'NONE', #51191, 999.9999999999998863 ) ;
#20451 = EDGE_CURVE ( 'NONE', #16795, #42240, #38248, .T. ) ;
#20452 = CARTESIAN_POINT ( 'NONE',  ( -14.00280974873554030, 0.000000000000000000, 12.40921378708904044 ) ) ;
#20453 = VECTOR ( 'NONE', #39227, 999.9999999999998863 ) ;
#20454 = AXIS2_PLACEMENT_3D ( 'NONE', #11835, #20916, #3341 ) ;
#20455 = ORIENTED_EDGE ( 'NONE', *, *, #43705, .F. ) ;
#20456 = CARTESIAN_POINT ( 'NONE',  ( -15.86710544311044302, 0.000000000000000000, 13.13336954653252953 ) ) ;
#20457 = LINE ( 'NONE', #27884, #22123 ) ;
#20458 = CARTESIAN_POINT ( 'NONE',  ( -15.81869938293262834, 0.000000000000000000, 6.913294768074659480 ) ) ;
#20459 = EDGE_CURVE ( 'NONE', #8988, #15552, #30024, .T. ) ;
#20460 = VERTEX_POINT ( 'NONE', #25766 ) ;
#20461 = VECTOR ( 'NONE', #31669, 999.9999999999998863 ) ;
#20462 = VECTOR ( 'NONE', #29303, 1000.000000000000114 ) ;
#20463 = ADVANCED_FACE ( 'NONE', ( #17235 ), #10883, .F. ) ;
#20464 = DIRECTION ( 'NONE',  ( 0.000000000000000000, -0.000000000000000000, -1.000000000000000000 ) ) ;
#20465 = PLANE ( 'NONE',  #31454 ) ;
#20466 = DIRECTION ( 'NONE',  ( -0.8531650599175527594, 0.4028455766673922356, 0.3313982828793700652 ) ) ;
#20467 = AXIS2_PLACEMENT_3D ( 'NONE', #41450, #11625, #2531 ) ;
#20468 = PLANE ( 'NONE',  #34087 ) ;
#20469 = LINE ( 'NONE', #15622, #7699 ) ;
#20470 = EDGE_CURVE ( 'NONE', #33290, #1300, #15171, .T. ) ;
#20471 = CARTESIAN_POINT ( 'NONE',  ( -11.69969505749696559, -0.6798977022406572646, 1.404187704473179865 ) ) ;
#20472 = AXIS2_PLACEMENT_3D ( 'NONE', #48139, #39914, #44728 ) ;
#20473 = VECTOR ( 'NONE', #25178, 1000.000000000000227 ) ;
#20474 = PLANE ( 'NONE',  #34004 ) ;
#20475 = ORIENTED_EDGE ( 'NONE', *, *, #10308, .F. ) ;
#20476 = LINE ( 'NONE', #24440, #43442 ) ;
#20477 = CARTESIAN_POINT ( 'NONE',  ( -14.28874784433092060, 4.010151117816508126, 9.012897199011266736 ) ) ;
#20478 = DIRECTION ( 'NONE',  ( 0.007781995580012663651, 0.000000000000000000, -0.9999697198139515519 ) ) ;
#20479 = EDGE_LOOP ( 'NONE', ( #51287, #47398, #38098, #14926 ) ) ;
#20480 = DIRECTION ( 'NONE',  ( 0.000000000000000000, -1.000000000000000000, 0.000000000000000000 ) ) ;
#20481 = DIRECTION ( 'NONE',  ( -0.5364919789714478471, 0.6444004775717705469, -0.5449076811759709926 ) ) ;
#20482 = ADVANCED_FACE ( 'NONE', ( #31907 ), #28479, .F. ) ;
#20483 = EDGE_CURVE ( 'NONE', #43341, #32707, #53491, .T. ) ;
#20484 = LINE ( 'NONE', #41754, #29514 ) ;
#20485 = LINE ( 'NONE', #11683, #53251 ) ;
#20486 = CARTESIAN_POINT ( 'NONE',  ( -10.84028925556084388, -0.1191753592594197858, 11.14116300850493246 ) ) ;
#20487 = AXIS2_PLACEMENT_3D ( 'NONE', #13388, #25309, #35248 ) ;
#20488 = EDGE_CURVE ( 'NONE', #49068, #53142, #49223, .T. ) ;
#20489 = ORIENTED_EDGE ( 'NONE', *, *, #18771, .F. ) ;
#20490 = EDGE_LOOP ( 'NONE', ( #46132, #31966, #2852, #13221 ) ) ;
#20491 = DIRECTION ( 'NONE',  ( 0.6427681459581294776, -0.7660444431189769032, 0.005002170337467562802 ) ) ;
#20492 = VECTOR ( 'NONE', #16547, 1000.000000000000227 ) ;
#20493 = DIRECTION ( 'NONE',  ( 0.6246952433987894571, -0.7422098413412800966, -0.2426528472758541777 ) ) ;
#20494 = VERTEX_POINT ( 'NONE', #39393 ) ;
#20495 = PLANE ( 'NONE',  #491 ) ;
#20496 = AXIS2_PLACEMENT_3D ( 'NONE', #1736, #35286, #5193 ) ;
#20497 = ORIENTED_EDGE ( 'NONE', *, *, #54100, .F. ) ;
#20498 = DIRECTION ( 'NONE',  ( 0.007781995580012662783, 0.000000000000000000, -0.9999697198139514409 ) ) ;
#20499 = VECTOR ( 'NONE', #39174, 1000.000000000000227 ) ;
#20500 = VECTOR ( 'NONE', #54318, 1000.000000000000227 ) ;
#20501 = ORIENTED_EDGE ( 'NONE', *, *, #35347, .T. ) ;
#20502 = ORIENTED_EDGE ( 'NONE', *, *, #23683, .F. ) ;
#20503 = ORIENTED_EDGE ( 'NONE', *, *, #8674, .T. ) ;
#20504 = DIRECTION ( 'NONE',  ( -0.6427681459581293666, -0.7660444431189770143, -0.005002170337467561935 ) ) ;
#20505 = DIRECTION ( 'NONE',  ( 0.005961354470445682716, -0.6427876096865404731, -0.7660212471507180654 ) ) ;
#20506 = DIRECTION ( 'NONE',  ( 0.2426528472758542054, 0.7422098413412800966, 0.6246952433987894571 ) ) ;
#20507 = VECTOR ( 'NONE', #44218, 999.9999999999998863 ) ;
#20508 = VECTOR ( 'NONE', #52706, 1000.000000000000114 ) ;
#20509 = PLANE ( 'NONE',  #37541 ) ;
#20510 = ADVANCED_FACE ( 'NONE', ( #52452 ), #1539, .F. ) ;
#20511 = ORIENTED_EDGE ( 'NONE', *, *, #19157, .T. ) ;
#20512 = AXIS2_PLACEMENT_3D ( 'NONE', #52295, #30717, #48017 ) ;
#20513 = ORIENTED_EDGE ( 'NONE', *, *, #49438, .F. ) ;
#20514 = VECTOR ( 'NONE', #12663, 1000.000000000000000 ) ;
#20515 = ORIENTED_EDGE ( 'NONE', *, *, #39592, .T. ) ;
#20516 = FACE_OUTER_BOUND ( 'NONE', #14255, .T. ) ;
#20517 = FACE_OUTER_BOUND ( 'NONE', #37693, .T. ) ;
#20518 = VERTEX_POINT ( 'NONE', #6626 ) ;
#20519 = FACE_OUTER_BOUND ( 'NONE', #15563, .T. ) ;
#20520 = ORIENTED_EDGE ( 'NONE', *, *, #24450, .F. ) ;
#20521 = PLANE ( 'NONE',  #13329 ) ;
#20522 = FACE_OUTER_BOUND ( 'NONE', #42413, .T. ) ;
#20523 = EDGE_CURVE ( 'NONE', #14352, #52494, #19398, .T. ) ;
#20524 = ORIENTED_EDGE ( 'NONE', *, *, #9104, .T. ) ;
#20525 = DIRECTION ( 'NONE',  ( 0.000000000000000000, -1.000000000000000000, 0.000000000000000000 ) ) ;
#20526 = ORIENTED_EDGE ( 'NONE', *, *, #23411, .T. ) ;
#20527 = ADVANCED_FACE ( 'NONE', ( #32488 ), #54054, .F. ) ;
#20528 = EDGE_CURVE ( 'NONE', #40640, #49579, #41272, .T. ) ;
#20529 = VECTOR ( 'NONE', #4707, 1000.000000000000114 ) ;
#20530 = LINE ( 'NONE', #15991, #49136 ) ;
#20531 = DIRECTION ( 'NONE',  ( -0.9999697198139514409, -0.000000000000000000, -0.007781995580013368816 ) ) ;
#20532 = LINE ( 'NONE', #37018, #20500 ) ;
#20533 = DIRECTION ( 'NONE',  ( 0.6427681459581294776, -0.7660444431189769032, 0.005002170337467562802 ) ) ;
#20534 = DIRECTION ( 'NONE',  ( 0.000000000000000000, -0.000000000000000000, -1.000000000000000000 ) ) ;
#20535 = PLANE ( 'NONE',  #31897 ) ;
#20536 = VECTOR ( 'NONE', #16774, 1000.000000000000227 ) ;
#20537 = ORIENTED_EDGE ( 'NONE', *, *, #53113, .T. ) ;
#20538 = ORIENTED_EDGE ( 'NONE', *, *, #54058, .F. ) ;
#20539 = EDGE_CURVE ( 'NONE', #35388, #36770, #2064, .T. ) ;
#20540 = DIRECTION ( 'NONE',  ( -0.5449076811759708816, 0.6444004775717707689, 0.5364919789714475140 ) ) ;
#20541 = AXIS2_PLACEMENT_3D ( 'NONE', #37757, #33483, #51376 ) ;
#20542 = DIRECTION ( 'NONE',  ( -0.005002170337468016433, -0.7660444431189770143, 0.6427681459581293666 ) ) ;
#20543 = CARTESIAN_POINT ( 'NONE',  ( -23.33849165029409889, 0.000000000000000000, 5.946783852668351855 ) ) ;
#20544 = DIRECTION ( 'NONE',  ( 0.000000000000000000, 1.000000000000000000, 0.000000000000000000 ) ) ;
#20545 = EDGE_CURVE ( 'NONE', #23008, #55560, #2363, .T. ) ;
#20546 = CARTESIAN_POINT ( 'NONE',  ( -10.00813838035478298, 0.000000000000000000, 10.77830692922518452 ) ) ;
#20547 = VECTOR ( 'NONE', #33659, 1000.000000000000227 ) ;
#20548 = DIRECTION ( 'NONE',  ( 0.6427681459581294776, -0.7660444431189769032, 0.005002170337467562802 ) ) ;
#20549 = ORIENTED_EDGE ( 'NONE', *, *, #3283, .T. ) ;
#20550 = LINE ( 'NONE', #7772, #8703 ) ;
#20551 = CARTESIAN_POINT ( 'NONE',  ( -30.79411802867772607, 0.000000000000000000, 8.643412946479525516 ) ) ;
#20552 = ORIENTED_EDGE ( 'NONE', *, *, #22495, .F. ) ;
#20553 = LINE ( 'NONE', #3219, #36802 ) ;
#20554 = ORIENTED_EDGE ( 'NONE', *, *, #52554, .F. ) ;
#20555 = EDGE_CURVE ( 'NONE', #15522, #35148, #1791, .T. ) ;
#20556 = DIRECTION ( 'NONE',  ( 0.6427681459581294776, -0.7660444431189769032, 0.005002170337467562802 ) ) ;
#20557 = LINE ( 'NONE', #19973, #29691 ) ;
#20558 = VECTOR ( 'NONE', #699, 999.9999999999998863 ) ;
#20559 = DIRECTION ( 'NONE',  ( 0.007781995580012662783, 0.000000000000000000, -0.9999697198139514409 ) ) ;
#20560 = DIRECTION ( 'NONE',  ( -0.005961354470445682716, -0.6427876096865404731, 0.7660212471507180654 ) ) ;
#20561 = VECTOR ( 'NONE', #5925, 999.9999999999998863 ) ;
#20562 = CARTESIAN_POINT ( 'NONE',  ( -67.80680003470160955, 0.1329109690309568104, 3.391838660566504071 ) ) ;
#20563 = ADVANCED_FACE ( 'NONE', ( #19695 ), #5800, .F. ) ;
#20564 = ORIENTED_EDGE ( 'NONE', *, *, #33851, .T. ) ;
#20565 = VECTOR ( 'NONE', #8545, 999.9999999999998863 ) ;
#20566 = ORIENTED_EDGE ( 'NONE', *, *, #1841, .T. ) ;
#20567 = CARTESIAN_POINT ( 'NONE',  ( -67.02352122496155573, -0.6009590134347525536, 0.3404743498653474698 ) ) ;
#20568 = CARTESIAN_POINT ( 'NONE',  ( -20.54049170961573267, 0.000000000000000000, 4.660556269540326646 ) ) ;
#20569 = CARTESIAN_POINT ( 'NONE',  ( 4.993307398318179047, 0.01266810708056629979, -2.289010529401725336 ) ) ;
#20570 = DIRECTION ( 'NONE',  ( 0.005961354470445682716, -0.6427876096865404731, -0.7660212471507180654 ) ) ;
#20571 = DIRECTION ( 'NONE',  ( -0.1139275668495183524, 0.9934890585767659488, 4.694855797473114533E-16 ) ) ;
#20572 = LINE ( 'NONE', #38742, #442 ) ;
#20573 = ORIENTED_EDGE ( 'NONE', *, *, #21878, .F. ) ;
#20574 = FACE_OUTER_BOUND ( 'NONE', #21061, .T. ) ;
#20575 = VECTOR ( 'NONE', #37309, 1000.000000000000114 ) ;
#20576 = LINE ( 'NONE', #37897, #22372 ) ;
#20577 = DIRECTION ( 'NONE',  ( 0.000000000000000000, -0.000000000000000000, -1.000000000000000000 ) ) ;
#20578 = ORIENTED_EDGE ( 'NONE', *, *, #10311, .T. ) ;
#20579 = CARTESIAN_POINT ( 'NONE',  ( -68.26343194379199986, -11.13167664141646185, 7.480095325092515068 ) ) ;
#20580 = DIRECTION ( 'NONE',  ( -0.5449076811759708816, 0.6444004775717707689, 0.5364919789714475140 ) ) ;
#20581 = ADVANCED_FACE ( 'NONE', ( #40451 ), #49525, .F. ) ;
#20582 = DIRECTION ( 'NONE',  ( 0.007781995580012663651, 0.000000000000000000, -0.9999697198139515519 ) ) ;
#20583 = ORIENTED_EDGE ( 'NONE', *, *, #33568, .F. ) ;
#20584 = LINE ( 'NONE', #29374, #29552 ) ;
#20585 = VECTOR ( 'NONE', #39657, 1000.000000000000000 ) ;
#20586 = ADVANCED_FACE ( 'NONE', ( #36187 ), #27662, .F. ) ;
#20587 = ORIENTED_EDGE ( 'NONE', *, *, #30611, .T. ) ;
#20588 = ORIENTED_EDGE ( 'NONE', *, *, #1559, .T. ) ;
#20589 = VECTOR ( 'NONE', #11477, 1000.000000000000227 ) ;
#20590 = EDGE_CURVE ( 'NONE', #33865, #15187, #23404, .T. ) ;
#20591 = VERTEX_POINT ( 'NONE', #10642 ) ;
#20592 = ADVANCED_FACE ( 'NONE', ( #46338 ), #29324, .F. ) ;
#20593 = EDGE_LOOP ( 'NONE', ( #47952, #4297, #16067, #881 ) ) ;
#20594 = PLANE ( 'NONE',  #41109 ) ;
#20596 = EDGE_CURVE ( 'NONE', #27675, #460, #45801, .T. ) ;
#20595 = ORIENTED_EDGE ( 'NONE', *, *, #4873, .F. ) ;
#20597 = CARTESIAN_POINT ( 'NONE',  ( -13.17964512767721530, 23.31695337602389273, -3.677660435020122964 ) ) ;
#20598 = EDGE_CURVE ( 'NONE', #14819, #10694, #37273, .T. ) ;
#20599 = ADVANCED_FACE ( 'NONE', ( #42654 ), #20535, .F. ) ;
#20600 = VECTOR ( 'NONE', #32353, 1000.000000000000114 ) ;
#20601 = ORIENTED_EDGE ( 'NONE', *, *, #47103, .T. ) ;
#20602 = CARTESIAN_POINT ( 'NONE',  ( -66.74449147233332269, -11.36157748060019301, 7.448312483692313357 ) ) ;
#20603 = ORIENTED_EDGE ( 'NONE', *, *, #51515, .T. ) ;
#20604 = EDGE_LOOP ( 'NONE', ( #27177, #27919, #35892, #51531 ) ) ;
#20605 = ADVANCED_FACE ( 'NONE', ( #29039 ), #7455, .F. ) ;
#20606 = AXIS2_PLACEMENT_3D ( 'NONE', #30347, #39130, #13318 ) ;
#20607 = FACE_OUTER_BOUND ( 'NONE', #11567, .T. ) ;
#20608 = LINE ( 'NONE', #28264, #8573 ) ;
#20609 = DIRECTION ( 'NONE',  ( 0.05705673239519650636, -0.9983709377222390602, -2.351258244848514932E-16 ) ) ;
#20610 = PLANE ( 'NONE',  #1500 ) ;
#20611 = DIRECTION ( 'NONE',  ( -0.9999697198139514409, -0.000000000000000000, -0.007781995580013368816 ) ) ;
#20612 = ORIENTED_EDGE ( 'NONE', *, *, #28542, .T. ) ;
#20613 = EDGE_LOOP ( 'NONE', ( #19923, #23386, #42165, #41706 ) ) ;
#20614 = ADVANCED_FACE ( 'NONE', ( #37863 ), #41549, .F. ) ;
#20615 = LINE ( 'NONE', #28558, #15803 ) ;
#20616 = CARTESIAN_POINT ( 'NONE',  ( -17.35017059011151375, 1.553641160433663071, 12.97584759397192045 ) ) ;
#20617 = EDGE_CURVE ( 'NONE', #7659, #21622, #33708, .T. ) ;
#20618 = DIRECTION ( 'NONE',  ( -0.3583679495452925523, -0.9335804264972047406, 0.000000000000000000 ) ) ;
#20619 = CARTESIAN_POINT ( 'NONE',  ( -13.19925735729079719, 0.000000000000000000, 2.871027103731305541 ) ) ;
#20620 = EDGE_CURVE ( 'NONE', #54500, #55411, #15996, .T. ) ;
#20621 = DIRECTION ( 'NONE',  ( 0.6427681459581294776, -0.7660444431189769032, 0.005002170337467562802 ) ) ;
#20622 = FACE_OUTER_BOUND ( 'NONE', #38758, .T. ) ;
#20623 = ORIENTED_EDGE ( 'NONE', *, *, #15867, .T. ) ;
#20624 = DIRECTION ( 'NONE',  ( 0.000000000000000000, -0.000000000000000000, -1.000000000000000000 ) ) ;
#20625 = CARTESIAN_POINT ( 'NONE',  ( -18.86354292863559579, 0.000000000000000000, 14.21804678658176080 ) ) ;
#20626 = ORIENTED_EDGE ( 'NONE', *, *, #13299, .F. ) ;
#20627 = ADVANCED_FACE ( 'NONE', ( #54576 ), #21073, .F. ) ;
#20628 = FACE_OUTER_BOUND ( 'NONE', #24717, .T. ) ;
#20629 = DIRECTION ( 'NONE',  ( 0.7660212471507180654, -0.6427876096865404731, 0.005961354470445141482 ) ) ;
#20630 = PLANE ( 'NONE',  #1825 ) ;
#20631 = CARTESIAN_POINT ( 'NONE',  ( -16.01450161900085689, 0.000000000000000000, 6.373112906405917322 ) ) ;
#20632 = LINE ( 'NONE', #46168, #54933 ) ;
#20633 = AXIS2_PLACEMENT_3D ( 'NONE', #16635, #16346, #32833 ) ;
#20634 = ORIENTED_EDGE ( 'NONE', *, *, #3742, .F. ) ;
#20635 = VERTEX_POINT ( 'NONE', #42094 ) ;
#20636 = PLANE ( 'NONE',  #14883 ) ;
#20637 = DIRECTION ( 'NONE',  ( -0.5449076811759708816, 0.6444004775717707689, 0.5364919789714475140 ) ) ;
#20638 = CARTESIAN_POINT ( 'NONE',  ( -26.23274948935539541, 17.48484997744522929, -4.621578396180252568 ) ) ;
#20639 = VECTOR ( 'NONE', #24859, 999.9999999999998863 ) ;
#20640 = DIRECTION ( 'NONE',  ( 0.007781995580012663651, -3.146120232559066537E-19, -0.9999697198139514409 ) ) ;
#20641 = LINE ( 'NONE', #33675, #36652 ) ;
#20642 = LINE ( 'NONE', #34270, #1966 ) ;
#20643 = CARTESIAN_POINT ( 'NONE',  ( -6.599926418471779854, -8.445284758064715902, 5.782009131042851635 ) ) ;
#20644 = LINE ( 'NONE', #47037, #16892 ) ;
#20645 = LINE ( 'NONE', #12416, #28732 ) ;
#20646 = DIRECTION ( 'NONE',  ( 0.5364919789714477361, 0.6444004775717706579, 0.5449076811759711036 ) ) ;
#20647 = EDGE_LOOP ( 'NONE', ( #9123, #31685, #29139 ) ) ;
#20648 = FACE_OUTER_BOUND ( 'NONE', #42720, .T. ) ;
#20649 = ORIENTED_EDGE ( 'NONE', *, *, #635, .T. ) ;
#20650 = ADVANCED_FACE ( 'NONE', ( #16840 ), #12578, .F. ) ;
#20651 = ORIENTED_EDGE ( 'NONE', *, *, #32486, .T. ) ;
#20652 = VERTEX_POINT ( 'NONE', #55431 ) ;
#20653 = ORIENTED_EDGE ( 'NONE', *, *, #50713, .T. ) ;
#20654 = ORIENTED_EDGE ( 'NONE', *, *, #50063, .F. ) ;
#20655 = LINE ( 'NONE', #7290, #14217 ) ;
#20656 = LINE ( 'NONE', #54427, #13866 ) ;
#20657 = CARTESIAN_POINT ( 'NONE',  ( -18.67775241435682432, 0.000000000000000000, 4.136394454059623804 ) ) ;
#20658 = EDGE_CURVE ( 'NONE', #8289, #713, #25351, .T. ) ;
#20659 = EDGE_CURVE ( 'NONE', #34052, #54291, #16532, .T. ) ;
#20660 = EDGE_CURVE ( 'NONE', #32666, #31029, #41805, .T. ) ;
#20661 = VERTEX_POINT ( 'NONE', #7190 ) ;
#20662 = PLANE ( 'NONE',  #14103 ) ;
#20663 = VERTEX_POINT ( 'NONE', #2898 ) ;
#20664 = CARTESIAN_POINT ( 'NONE',  ( -66.74342152241241877, -11.36145478494482042, -7.448289400635804469 ) ) ;
#20665 = EDGE_CURVE ( 'NONE', #10496, #32467, #51184, .T. ) ;
#20666 = ORIENTED_EDGE ( 'NONE', *, *, #30580, .T. ) ;
#20667 = CARTESIAN_POINT ( 'NONE',  ( -65.07007842715393053, -9.156458274479485127, -0.3798655365511886539 ) ) ;
#20668 = LINE ( 'NONE', #37984, #50947 ) ;
#20669 = CARTESIAN_POINT ( 'NONE',  ( 4.930947970565946470, -1.129146301979396139, -1.967953638240999670 ) ) ;
#20670 = ORIENTED_EDGE ( 'NONE', *, *, #6136, .T. ) ;
#20671 = CARTESIAN_POINT ( 'NONE',  ( -22.40478740399063895, 0.000000000000000000, 5.384712028983816623 ) ) ;
#20672 = ORIENTED_EDGE ( 'NONE', *, *, #54889, .F. ) ;
#20673 = VECTOR ( 'NONE', #49983, 1000.000000000000227 ) ;
#20674 = DIRECTION ( 'NONE',  ( -0.5364919789714478471, 0.6444004775717705469, -0.5449076811759709926 ) ) ;
#20675 = CARTESIAN_POINT ( 'NONE',  ( -30.79411802867772607, 0.000000000000000000, 8.643412946479525516 ) ) ;
#20676 = EDGE_CURVE ( 'NONE', #9163, #37975, #16257, .T. ) ;
#20677 = CARTESIAN_POINT ( 'NONE',  ( -17.69029958343410769, 0.000000000000000000, 8.576063877996469742 ) ) ;
#20678 = PLANE ( 'NONE',  #34043 ) ;
#20679 = DIRECTION ( 'NONE',  ( 0.000000000000000000, -1.000000000000000000, 0.000000000000000000 ) ) ;
#20680 = CARTESIAN_POINT ( 'NONE',  ( -15.53106400201207116, 0.000000000000000000, 3.960876654664550411 ) ) ;
#20681 = ADVANCED_FACE ( 'NONE', ( #33578 ), #55725, .F. ) ;
#20682 = LINE ( 'NONE', #42535, #28470 ) ;
#20683 = CARTESIAN_POINT ( 'NONE',  ( -69.97337567751375786, -11.73184720622960953, 8.563005977519212664 ) ) ;
#20684 = ORIENTED_EDGE ( 'NONE', *, *, #11182, .T. ) ;
#20685 = DIRECTION ( 'NONE',  ( 0.3535533905932752297, -0.6123724356957952475, 0.7071067811865462405 ) ) ;
#20686 = ORIENTED_EDGE ( 'NONE', *, *, #49664, .T. ) ;
#20687 = ADVANCED_FACE ( 'NONE', ( #44070 ), #634, .F. ) ;
#20688 = FACE_OUTER_BOUND ( 'NONE', #25757, .T. ) ;
#20689 = DIRECTION ( 'NONE',  ( 0.9999697198139515519, 0.000000000000000000, 0.007781995580013368816 ) ) ;
#20690 = LINE ( 'NONE', #16402, #15957 ) ;
#20691 = PLANE ( 'NONE',  #6803 ) ;
#20692 = CARTESIAN_POINT ( 'NONE',  ( -12.64297938670245536, 4.333955019861511992, 1.454618426794188402 ) ) ;
#20693 = EDGE_CURVE ( 'NONE', #11344, #3168, #17670, .T. ) ;
#20694 = DIRECTION ( 'NONE',  ( 0.007781995580012663651, -3.146120232559066537E-19, -0.9999697198139514409 ) ) ;
#20695 = SHAPE_DEFINITION_REPRESENTATION ( #18260, #3156 ) ;
#20696 = VERTEX_POINT ( 'NONE', #21911 ) ;
#20697 = LINE ( 'NONE', #16409, #42819 ) ;
#20698 = DIRECTION ( 'NONE',  ( 0.000000000000000000, -1.000000000000000000, 0.000000000000000000 ) ) ;
#20699 = CARTESIAN_POINT ( 'NONE',  ( -11.79672450625168878, 0.000000000000000000, 1.773945729262041748 ) ) ;
#20700 = CARTESIAN_POINT ( 'NONE',  ( -19.60990026154428278, 0.000000000000000000, 4.498472333781370125 ) ) ;
#20701 = PLANE ( 'NONE',  #55433 ) ;
#20702 = DIRECTION ( 'NONE',  ( 0.6427681459581294776, -0.7660444431189769032, 0.005002170337467562802 ) ) ;
#20703 = CARTESIAN_POINT ( 'NONE',  ( -9.808144436391993182, 0.000000000000000000, 10.77986332834118777 ) ) ;
#20704 = CARTESIAN_POINT ( 'NONE',  ( 4.912750499197527709, -1.131233082521084343, -2.162384853247615535 ) ) ;
#20705 = ORIENTED_EDGE ( 'NONE', *, *, #15191, .T. ) ;
#20706 = DIRECTION ( 'NONE',  ( -0.6427681459581293666, -0.7660444431189770143, -0.005002170337467561935 ) ) ;
#20707 = DIRECTION ( 'NONE',  ( -1.000000000000000000, 0.000000000000000000, 0.000000000000000000 ) ) ;
#20708 = ORIENTED_EDGE ( 'NONE', *, *, #31040, .F. ) ;
#20709 = ORIENTED_EDGE ( 'NONE', *, *, #16802, .T. ) ;
#20710 = DIRECTION ( 'NONE',  ( -0.9999697198139514409, -0.000000000000000000, -0.007781995580013368816 ) ) ;
#20711 = AXIS2_PLACEMENT_3D ( 'NONE', #47018, #12930, #42735 ) ;
#20712 = ORIENTED_EDGE ( 'NONE', *, *, #31844, .F. ) ;
#20713 = ORIENTED_EDGE ( 'NONE', *, *, #41083, .F. ) ;
#20714 = PLANE ( 'NONE',  #8419 ) ;
#20715 = EDGE_LOOP ( 'NONE', ( #30555, #15642, #23461, #6752 ) ) ;
#20716 = ORIENTED_EDGE ( 'NONE', *, *, #47724, .T. ) ;
#20717 = ORIENTED_EDGE ( 'NONE', *, *, #46106, .F. ) ;
#20718 = LINE ( 'NONE', #26879, #14882 ) ;
#20719 = DIRECTION ( 'NONE',  ( 0.6427681459581294776, -0.7660444431189769032, 0.005002170337467562802 ) ) ;
#20720 = PLANE ( 'NONE',  #4047 ) ;
#20721 = ADVANCED_FACE ( 'NONE', ( #21659 ), #30469, .F. ) ;
#20722 = EDGE_LOOP ( 'NONE', ( #29389, #44315, #33494, #23800 ) ) ;
#20723 = ORIENTED_EDGE ( 'NONE', *, *, #37142, .T. ) ;
#20724 = EDGE_CURVE ( 'NONE', #22478, #21969, #35279, .T. ) ;
#20725 = EDGE_CURVE ( 'NONE', #42368, #45163, #13674, .T. ) ;
#20726 = CARTESIAN_POINT ( 'NONE',  ( -20.37261732798432945, 4.657758921906512306, 4.446741263022703450 ) ) ;
#20727 = FACE_OUTER_BOUND ( 'NONE', #44166, .T. ) ;
#20728 = EDGE_LOOP ( 'NONE', ( #19240, #7179, #24646, #25737 ) ) ;
#20729 = DIRECTION ( 'NONE',  ( 0.9999697198139515519, 0.000000000000000000, 0.007781995580013368816 ) ) ;
#20730 = ORIENTED_EDGE ( 'NONE', *, *, #8109, .F. ) ;
#20731 = CARTESIAN_POINT ( 'NONE',  ( 2.072287782118878319, 0.000000000000000000, -2.950529333540147015 ) ) ;
#20732 = DIRECTION ( 'NONE',  ( -0.5449076811759708816, 0.6444004775717707689, 0.5364919789714475140 ) ) ;
#20733 = EDGE_LOOP ( 'NONE', ( #4905, #40175, #5212, #36053 ) ) ;
#20734 = CARTESIAN_POINT ( 'NONE',  ( -24.26986129792355129, -0.1191753592594197858, 6.208864760408702388 ) ) ;
#20735 = CARTESIAN_POINT ( 'NONE',  ( -12.23851102634202448, -0.1191753592594197858, 11.68427982808754884 ) ) ;
#20736 = ORIENTED_EDGE ( 'NONE', *, *, #46863, .T. ) ;
#20737 = CARTESIAN_POINT ( 'NONE',  ( -11.63121920435228951, 0.000000000000000000, 6.207218567471217696 ) ) ;
#20738 = LINE ( 'NONE', #42863, #2055 ) ;
#20739 = CARTESIAN_POINT ( 'NONE',  ( 2.072287782118878319, 0.000000000000000000, -2.950529333540147015 ) ) ;
#20740 = DIRECTION ( 'NONE',  ( 0.9999697198139515519, 0.000000000000000000, 0.007781995580013368816 ) ) ;
#20741 = ORIENTED_EDGE ( 'NONE', *, *, #55093, .F. ) ;
#20742 = AXIS2_PLACEMENT_3D ( 'NONE', #3764, #8311, #25939 ) ;
#20743 = PLANE ( 'NONE',  #35550 ) ;
#20744 = DIRECTION ( 'NONE',  ( -0.9999697198139514409, -0.000000000000000000, -0.007781995580013368816 ) ) ;
#20745 = DIRECTION ( 'NONE',  ( -0.005002170337468016433, -0.7660444431189770143, 0.6427681459581293666 ) ) ;
#20746 = DIRECTION ( 'NONE',  ( 0.9999697198139515519, 0.000000000000000000, 0.007781995580013368816 ) ) ;
#20747 = EDGE_CURVE ( 'NONE', #25299, #3665, #34698, .T. ) ;
#20748 = FACE_OUTER_BOUND ( 'NONE', #31735, .T. ) ;
#20749 = CARTESIAN_POINT ( 'NONE',  ( -13.53673582514181106, 0.000000000000000000, 12.22817484722816772 ) ) ;
#20750 = CARTESIAN_POINT ( 'NONE',  ( -69.07738657957442285, -11.62910036973895878, -7.520604412854629217 ) ) ;
#20751 = ORIENTED_EDGE ( 'NONE', *, *, #29487, .F. ) ;
#20753 = EDGE_CURVE ( 'NONE', #47842, #47452, #47194, .T. ) ;
#20752 = DIRECTION ( 'NONE',  ( 0.5449076811759707706, 0.6444004775717708799, -0.5364919789714476250 ) ) ;
#20754 = CARTESIAN_POINT ( 'NONE',  ( -13.23414441016926801, -0.8417996532631562001, 1.995054423283073586 ) ) ;
#20755 = ORIENTED_EDGE ( 'NONE', *, *, #49876, .F. ) ;
#20756 = DIRECTION ( 'NONE',  ( -0.7660212471507179544, -0.6427876096865405842, -0.005961354470445141482 ) ) ;
#20757 = LINE ( 'NONE', #51430, #13667 ) ;
#20758 = EDGE_CURVE ( 'NONE', #48862, #41291, #8892, .T. ) ;
#20759 = PLANE ( 'NONE',  #53056 ) ;
#20760 = CARTESIAN_POINT ( 'NONE',  ( -15.13495153988577968, 0.000000000000000000, 12.76973526769478084 ) ) ;
#20761 = DIRECTION ( 'NONE',  ( -0.005961354470445682716, -0.6427876096865404731, 0.7660212471507180654 ) ) ;
#20762 = ORIENTED_EDGE ( 'NONE', *, *, #44510, .F. ) ;
#20763 = ORIENTED_EDGE ( 'NONE', *, *, #6732, .F. ) ;
#20764 = CARTESIAN_POINT ( 'NONE',  ( -19.82770700041984924, 4.010151117816509903, 4.255741666113602939 ) ) ;
#20765 = PLANE ( 'NONE',  #27721 ) ;
#20766 = LINE ( 'NONE', #3710, #55628 ) ;
#20767 = VERTEX_POINT ( 'NONE', #4048 ) ;
#20768 = CARTESIAN_POINT ( 'NONE',  ( -17.66730715539184615, 0.000000000000000000, 5.621586251934354017 ) ) ;
#20769 = EDGE_LOOP ( 'NONE', ( #31258, #37887, #29806, #46995 ) ) ;
#20770 = CARTESIAN_POINT ( 'NONE',  ( -14.56888064431065821, -0.1191753592594197858, 12.58947452739191064 ) ) ;
#20771 = ORIENTED_EDGE ( 'NONE', *, *, #48333, .T. ) ;
#20772 = EDGE_LOOP ( 'NONE', ( #46841, #8074, #27309, #19167 ) ) ;
#20773 = ORIENTED_EDGE ( 'NONE', *, *, #45738, .F. ) ;
#20774 = CARTESIAN_POINT ( 'NONE',  ( -13.63673279712320507, -0.1191753592594197858, 12.22739664767016521 ) ) ;
#20775 = EDGE_CURVE ( 'NONE', #17655, #30132, #26196, .T. ) ;
#20776 = CARTESIAN_POINT ( 'NONE',  ( -17.74560456716937296, 0.000000000000000000, 3.774316574337878372 ) ) ;
#20777 = PLANE ( 'NONE',  #1278 ) ;
#20778 = STYLED_ITEM ( 'NONE', ( #47425 ), #49640 ) ;
#20779 = CARTESIAN_POINT ( 'NONE',  ( -14.56888064431065821, -0.1191753592594197858, 12.58947452739191064 ) ) ;
#20780 = ORIENTED_EDGE ( 'NONE', *, *, #48203, .T. ) ;
#20781 = ADVANCED_FACE ( 'NONE', ( #21378 ), #38709, .F. ) ;
#20782 = ORIENTED_EDGE ( 'NONE', *, *, #53335, .T. ) ;
#20783 = ORIENTED_EDGE ( 'NONE', *, *, #32584, .F. ) ;
#20784 = DIRECTION ( 'NONE',  ( 0.007781995580012663651, 0.000000000000000000, -0.9999697198139515519 ) ) ;
#20785 = CARTESIAN_POINT ( 'NONE',  ( -24.27063949748155380, 0.000000000000000000, 6.308861732390097288 ) ) ;
#20786 = ORIENTED_EDGE ( 'NONE', *, *, #5022, .F. ) ;
#20787 = CARTESIAN_POINT ( 'NONE',  ( 1.969897575278193980, 0.000000000000000000, 10.20639235748909890 ) ) ;
#20788 = ORIENTED_EDGE ( 'NONE', *, *, #31094, .F. ) ;
#20789 = DIRECTION ( 'NONE',  ( 0.9999697198139515519, 0.000000000000000000, 0.007781995580013368816 ) ) ;
#20790 = DIRECTION ( 'NONE',  ( 0.000000000000000000, -0.000000000000000000, -1.000000000000000000 ) ) ;
#20791 = ORIENTED_EDGE ( 'NONE', *, *, #50697, .F. ) ;
#20792 = LINE ( 'NONE', #3480, #19522 ) ;
#20793 = EDGE_LOOP ( 'NONE', ( #38166, #23178, #26823 ) ) ;
#20794 = EDGE_CURVE ( 'NONE', #12574, #49826, #9138, .T. ) ;
#20795 = CARTESIAN_POINT ( 'NONE',  ( -12.33850799832341849, 0.000000000000000000, 11.68350162852954632 ) ) ;
#20796 = FACE_OUTER_BOUND ( 'NONE', #42057, .T. ) ;
#20797 = ORIENTED_EDGE ( 'NONE', *, *, #19807, .F. ) ;
#20798 = DIRECTION ( 'NONE',  ( 0.9999697198139515519, 0.000000000000000000, 0.007781995580013368816 ) ) ;
#20799 = DIRECTION ( 'NONE',  ( 0.007781995580012663651, -3.146120232559066537E-19, -0.9999697198139514409 ) ) ;
#20800 = DIRECTION ( 'NONE',  ( -0.5364919789714478471, 0.6444004775717705469, -0.5449076811759709926 ) ) ;
#20801 = DIRECTION ( 'NONE',  ( 0.007781995580012662783, 0.000000000000000000, -0.9999697198139514409 ) ) ;
#20802 = ORIENTED_EDGE ( 'NONE', *, *, #37964, .T. ) ;
#20803 = ORIENTED_EDGE ( 'NONE', *, *, #39241, .T. ) ;
#20804 = LINE ( 'NONE', #37868, #42755 ) ;
#20805 = DIRECTION ( 'NONE',  ( -0.005002170337468016433, -0.7660444431189770143, 0.6427681459581293666 ) ) ;
#20806 = CARTESIAN_POINT ( 'NONE',  ( -17.11479534437067329, 0.7721120973665037690, 4.796456341994528749 ) ) ;
#20807 = FACE_OUTER_BOUND ( 'NONE', #13530, .T. ) ;
#20808 = DIRECTION ( 'NONE',  ( 0.9999697198139515519, 0.000000000000000000, 0.007781995580013368816 ) ) ;
#20809 = CARTESIAN_POINT ( 'NONE',  ( -13.24198947131226944, 0.000000000000000000, 8.362011986176833389 ) ) ;
#20810 = ORIENTED_EDGE ( 'NONE', *, *, #1876, .T. ) ;
#20811 = DIRECTION ( 'NONE',  ( 0.5449076811759707706, 0.6444004775717708799, -0.5364919789714476250 ) ) ;
#20812 = PLANE ( 'NONE',  #3262 ) ;
#20813 = ORIENTED_EDGE ( 'NONE', *, *, #22192, .F. ) ;
#20814 = CARTESIAN_POINT ( 'NONE',  ( -29.86352658060627618, 0.000000000000000000, 8.481329010720569883 ) ) ;
#20815 = EDGE_LOOP ( 'NONE', ( #24736, #25527, #34208, #14314 ) ) ;
#20816 = CARTESIAN_POINT ( 'NONE',  ( -9.292346798231170268, 0.000000000000000000, 4.209433850727466009 ) ) ;
#20817 = CARTESIAN_POINT ( 'NONE',  ( -8.975993561185934055, -0.1191753592594197858, 10.41700724906143982 ) ) ;
#20818 = EDGE_CURVE ( 'NONE', #39737, #31756, #4884, .T. ) ;
#20819 = DIRECTION ( 'NONE',  ( 0.007781995580012663651, 0.000000000000000000, -0.9999697198139515519 ) ) ;
#20820 = FACE_OUTER_BOUND ( 'NONE', #6155, .T. ) ;
#20821 = CARTESIAN_POINT ( 'NONE',  ( -69.63916331601677712, 0.1328488985137141754, -7.034467916851212976 ) ) ;
#20822 = EDGE_LOOP ( 'NONE', ( #48302, #24925, #21258, #22271 ) ) ;
#20823 = ORIENTED_EDGE ( 'NONE', *, *, #35511, .T. ) ;
#20824 = DIRECTION ( 'NONE',  ( 0.005002170337468016433, -0.7660444431189770143, -0.6427681459581293666 ) ) ;
#20825 = FACE_OUTER_BOUND ( 'NONE', #32523, .T. ) ;
#20826 = LINE ( 'NONE', #23971, #1580 ) ;
#20827 = EDGE_CURVE ( 'NONE', #46599, #36877, #18210, .T. ) ;
#20828 = DIRECTION ( 'NONE',  ( 0.007781995580012663651, 0.000000000000000000, -0.9999697198139515519 ) ) ;
#20829 = LINE ( 'NONE', #52355, #43718 ) ;
#20830 = DIRECTION ( 'NONE',  ( 0.8531650599175527594, 0.4028455766673922356, -0.3313982828793700652 ) ) ;
#20832 = EDGE_CURVE ( 'NONE', #36873, #33080, #26744, .T. ) ;
#20831 = EDGE_LOOP ( 'NONE', ( #1594, #49528, #36810, #18915, #13186 ) ) ;
#20833 = DIRECTION ( 'NONE',  ( 0.5449076811759707706, 0.6444004775717708799, -0.5364919789714476250 ) ) ;
#20834 = EDGE_CURVE ( 'NONE', #32724, #6604, #30986, .T. ) ;
#20835 = FACE_OUTER_BOUND ( 'NONE', #54424, .T. ) ;
#20836 = CARTESIAN_POINT ( 'NONE',  ( -10.44017651129710700, 0.000000000000000000, 6.585819606917006297 ) ) ;
#20837 = VERTEX_POINT ( 'NONE', #35538 ) ;
#20838 = DIRECTION ( 'NONE',  ( 0.7660212471507180654, -0.6427876096865404731, 0.005961354470445141482 ) ) ;
#20839 = EDGE_CURVE ( 'NONE', #33297, #46700, #25617, .T. ) ;
#20840 = LINE ( 'NONE', #37610, #42241 ) ;
#20841 = CARTESIAN_POINT ( 'NONE',  ( -9.808144436391993182, 0.000000000000000000, 10.77986332834118777 ) ) ;
#20842 = ORIENTED_EDGE ( 'NONE', *, *, #31578, .F. ) ;
#20843 = CARTESIAN_POINT ( 'NONE',  ( -20.72814514249575168, 20.40220053346460460, -4.343046601173932153 ) ) ;
#20844 = ADVANCED_FACE ( 'NONE', ( #34427 ), #51733, .F. ) ;
#20845 = VERTEX_POINT ( 'NONE', #6555 ) ;
#20846 = EDGE_CURVE ( 'NONE', #17974, #8156, #44344, .T. ) ;
#20847 = VECTOR ( 'NONE', #21235, 999.9999999999998863 ) ;
#20848 = ORIENTED_EDGE ( 'NONE', *, *, #11355, .F. ) ;
#20849 = ORIENTED_EDGE ( 'NONE', *, *, #47304, .T. ) ;
#20850 = ORIENTED_EDGE ( 'NONE', *, *, #40969, .T. ) ;
#20851 = DIRECTION ( 'NONE',  ( -0.7660212471507179544, -0.6427876096865405842, -0.005961354470445141482 ) ) ;
#20852 = ORIENTED_EDGE ( 'NONE', *, *, #17574, .F. ) ;
#20853 = DIRECTION ( 'NONE',  ( 0.005961354470445682716, -0.6427876096865404731, -0.7660212471507180654 ) ) ;
#20854 = EDGE_CURVE ( 'NONE', #34036, #43311, #5724, .T. ) ;
#20855 = ORIENTED_EDGE ( 'NONE', *, *, #20424, .F. ) ;
#20856 = DIRECTION ( 'NONE',  ( -0.005961354470445682716, -0.6427876096865404731, 0.7660212471507180654 ) ) ;
#20857 = EDGE_LOOP ( 'NONE', ( #12937, #47713, #52225, #26363 ) ) ;
#20858 = ORIENTED_EDGE ( 'NONE', *, *, #19785, .T. ) ;
#20859 = EDGE_CURVE ( 'NONE', #33755, #1256, #31287, .T. ) ;
#20860 = LINE ( 'NONE', #4406, #13874 ) ;
#20861 = DIRECTION ( 'NONE',  ( 0.000000000000000000, -0.000000000000000000, -1.000000000000000000 ) ) ;
#20862 = CARTESIAN_POINT ( 'NONE',  ( -10.94028622754223967, 0.000000000000000000, 11.14038480894692995 ) ) ;
#20863 = DIRECTION ( 'NONE',  ( 0.000000000000000000, -0.000000000000000000, -1.000000000000000000 ) ) ;
#20864 = ORIENTED_EDGE ( 'NONE', *, *, #55791, .F. ) ;
#20865 = ORIENTED_EDGE ( 'NONE', *, *, #15340, .F. ) ;
#20866 = CARTESIAN_POINT ( 'NONE',  ( -18.66354898467281132, 0.000000000000000000, 14.21960318569776582 ) ) ;
#20867 = CARTESIAN_POINT ( 'NONE',  ( -24.96676581047183063, 18.24370688441070953, 4.565775410814726598 ) ) ;
#20868 = FACE_OUTER_BOUND ( 'NONE', #9645, .T. ) ;
#20869 = LINE ( 'NONE', #29965, #11288 ) ;
#20870 = PLANE ( 'NONE',  #40380 ) ;
#20871 = LINE ( 'NONE', #43028, #39562 ) ;
#20872 = ORIENTED_EDGE ( 'NONE', *, *, #13124, .T. ) ;
#20873 = LINE ( 'NONE', #25170, #41056 ) ;
#20874 = LINE ( 'NONE', #42189, #30391 ) ;
#20875 = ORIENTED_EDGE ( 'NONE', *, *, #15714, .F. ) ;
#20876 = DIRECTION ( 'NONE',  ( 0.005961354470445682716, -0.6427876096865404731, -0.7660212471507180654 ) ) ;
#20877 = LINE ( 'NONE', #51280, #20547 ) ;
#20878 = LINE ( 'NONE', #46427, #30864 ) ;
#20879 = ADVANCED_FACE ( 'NONE', ( #36960 ), #28132, .F. ) ;
#20880 = CARTESIAN_POINT ( 'NONE',  ( -13.27065584551087163, 0.000000000000000000, 12.04557950825129176 ) ) ;
#20881 = CARTESIAN_POINT ( 'NONE',  ( -16.80850742758478233, 3.686347215771509145, 9.460240024641782597 ) ) ;
#20882 = AXIS2_PLACEMENT_3D ( 'NONE', #53571, #22645, #31999 ) ;
#20883 = ORIENTED_EDGE ( 'NONE', *, *, #8016, .T. ) ;
#20884 = VERTEX_POINT ( 'NONE', #27885 ) ;
#20885 = LINE ( 'NONE', #29128, #6736 ) ;
#20886 = CARTESIAN_POINT ( 'NONE',  ( -20.38426584293951294, 20.88941447422692477, 4.312559560550884186 ) ) ;
#20887 = LINE ( 'NONE', #38209, #4305 ) ;
#20888 = EDGE_CURVE ( 'NONE', #22464, #51166, #40371, .T. ) ;
#20889 = DIRECTION ( 'NONE',  ( 0.9999697198139515519, 0.000000000000000000, 0.007781995580013368816 ) ) ;
#20890 = PLANE ( 'NONE',  #33932 ) ;
#20891 = LINE ( 'NONE', #16350, #1047 ) ;
#20892 = CARTESIAN_POINT ( 'NONE',  ( -15.81007722241678159, 0.000000000000000000, 5.805365658301368192 ) ) ;
#20893 = EDGE_CURVE ( 'NONE', #30294, #55101, #48891, .T. ) ;
#20894 = LINE ( 'NONE', #38218, #42298 ) ;
#20895 = CARTESIAN_POINT ( 'NONE',  ( -66.67823795591188230, -9.340872688141725888, 4.722169080041619615 ) ) ;
#20896 =( BOUNDED_CURVE ( )  B_SPLINE_CURVE ( 3, ( #5873, #39682, #9575, #36251 ),
 .UNSPECIFIED., .F., .F. ) 
 B_SPLINE_CURVE_WITH_KNOTS ( ( 4, 4 ),
 ( 2.001189637452388759, 3.141592653589797113 ),
 .UNSPECIFIED. ) 
 CURVE ( )  GEOMETRIC_REPRESENTATION_ITEM ( )  RATIONAL_B_SPLINE_CURVE ( ( 1.000000000000000000, 0.8945281452387652266, 0.8945281452387652266, 1.000000000000000000 ) ) 
 REPRESENTATION_ITEM ( '' )  );
#20897 = CARTESIAN_POINT ( 'NONE',  ( -14.01545677930355183, 0.000000000000000000, 2.126011111488108174 ) ) ;
#20898 = EDGE_LOOP ( 'NONE', ( #43354, #52489, #230, #499 ) ) ;
#20899 = CARTESIAN_POINT ( 'NONE',  ( -24.27063949748155380, 0.000000000000000000, 6.308861732390097288 ) ) ;
#20900 = ORIENTED_EDGE ( 'NONE', *, *, #4543, .F. ) ;
#20901 = EDGE_CURVE ( 'NONE', #23998, #35256, #48615, .T. ) ;
#20902 = EDGE_LOOP ( 'NONE', ( #9252, #10984, #21725, #47211 ) ) ;
#20903 = EDGE_CURVE ( 'NONE', #44587, #4593, #18497, .T. ) ;
#20904 = VERTEX_POINT ( 'NONE', #10261 ) ;
#20905 = ORIENTED_EDGE ( 'NONE', *, *, #42469, .F. ) ;
#20906 = ORIENTED_EDGE ( 'NONE', *, *, #30357, .F. ) ;
#20907 = EDGE_LOOP ( 'NONE', ( #1253, #7649, #55699, #13950 ) ) ;
#20908 = CARTESIAN_POINT ( 'NONE',  ( -17.42565663055581382, 0.000000000000000000, 8.578123390648475066 ) ) ;
#20909 = CARTESIAN_POINT ( 'NONE',  ( -18.67619601524082285, 0.000000000000000000, 3.936400510096834893 ) ) ;
#20910 = CARTESIAN_POINT ( 'NONE',  ( -13.02886805270398618, 4.172053068839010059, 8.789225786196009693 ) ) ;
#20911 = ADVANCED_FACE ( 'NONE', ( #23869 ), #27586, .F. ) ;
#20912 = AXIS2_PLACEMENT_3D ( 'NONE', #31835, #49146, #27581 ) ;
#20913 = VERTEX_POINT ( 'NONE', #35839 ) ;
#20914 = CARTESIAN_POINT ( 'NONE',  ( -20.16176772743538237, -0.1191753592594197858, 14.76194180572237968 ) ) ;
#20915 = ORIENTED_EDGE ( 'NONE', *, *, #45591, .T. ) ;
#20916 = DIRECTION ( 'NONE',  ( 0.000000000000000000, -1.000000000000000000, 0.000000000000000000 ) ) ;
#20917 = ORIENTED_EDGE ( 'NONE', *, *, #16007, .T. ) ;
#20918 = VECTOR ( 'NONE', #42348, 1000.000000000000227 ) ;
#20919 = CARTESIAN_POINT ( 'NONE',  ( 5.558065546916891364, 8.867787166497208620E-06, 2.260478567416572826 ) ) ;
#20920 = LINE ( 'NONE', #7591, #50011 ) ;
#20921 = DIRECTION ( 'NONE',  ( 0.9321478471874540261, 0.000000000000000000, -0.3620778797217456546 ) ) ;
#20922 = ORIENTED_EDGE ( 'NONE', *, *, #45357, .T. ) ;
#20923 = DIRECTION ( 'NONE',  ( 0.000000000000000000, -0.000000000000000000, -1.000000000000000000 ) ) ;
#20924 = ORIENTED_EDGE ( 'NONE', *, *, #1866, .F. ) ;
#20925 = DIRECTION ( 'NONE',  ( 0.9999697198139515519, 0.000000000000000000, 0.007781995580013368816 ) ) ;
#20926 = CARTESIAN_POINT ( 'NONE',  ( -13.63673279712320507, -0.1191753592594197858, 12.22739664767016521 ) ) ;
#20927 = CARTESIAN_POINT ( 'NONE',  ( -13.73672976910459909, 0.000000000000000000, 12.22661844811216270 ) ) ;
#20928 = CARTESIAN_POINT ( 'NONE',  ( -23.33849165029409889, 0.000000000000000000, 5.946783852668351855 ) ) ;
#20929 = DIRECTION ( 'NONE',  ( 0.007781995580012662783, 0.000000000000000000, -0.9999697198139514409 ) ) ;
#20930 = CARTESIAN_POINT ( 'NONE',  ( -67.81506811452879901, 0.000000000000000000, -7.454891809856698970 ) ) ;
#20931 = PLANE ( 'NONE',  #3996 ) ;
#20932 = CARTESIAN_POINT ( 'NONE',  ( -21.47419595591918906, 0.000000000000000000, 5.222628093224860102 ) ) ;
#20933 = ORIENTED_EDGE ( 'NONE', *, *, #38878, .T. ) ;
#20934 = LINE ( 'NONE', #34867, #42869 ) ;
#20935 = ORIENTED_EDGE ( 'NONE', *, *, #4326, .F. ) ;
#20936 = EDGE_CURVE ( 'NONE', #5490, #20845, #9727, .T. ) ;
#20937 = AXIS2_PLACEMENT_3D ( 'NONE', #10213, #51366, #42553 ) ;
#20938 = VECTOR ( 'NONE', #47115, 999.9999999999998863 ) ;
#20939 = DIRECTION ( 'NONE',  ( 0.5364919789714477361, 0.6444004775717706579, 0.5449076811759711036 ) ) ;
#20940 = CARTESIAN_POINT ( 'NONE',  ( -12.15193928448667116, -0.1191753592594194527, 1.501852324026011987 ) ) ;
#20941 = CARTESIAN_POINT ( 'NONE',  ( -20.19028461120871754, -5.698858183938165567, 13.87732110161523202 ) ) ;
#20942 = EDGE_CURVE ( 'NONE', #36489, #34036, #40074, .T. ) ;
#20943 = DIRECTION ( 'NONE',  ( 0.007781995580012663651, -3.146120232559066537E-19, -0.9999697198139514409 ) ) ;
#20944 = FACE_OUTER_BOUND ( 'NONE', #52398, .T. ) ;
#20945 = LINE ( 'NONE', #29491, #16514 ) ;
#20946 = CONTEXT_DEPENDENT_SHAPE_REPRESENTATION ( #2803, #44128 ) ;
#20947 = ORIENTED_EDGE ( 'NONE', *, *, #8469, .T. ) ;
#20948 = ADVANCED_FACE ( 'NONE', ( #53686 ), #23594, .F. ) ;
#20949 = CARTESIAN_POINT ( 'NONE',  ( -19.60084266227577032, 19.60967325090364000, 4.310338978832157331 ) ) ;
#20950 = CARTESIAN_POINT ( 'NONE',  ( -17.93139508144814442, 0.000000000000000000, 13.85596890686001537 ) ) ;
#20951 = LINE ( 'NONE', #54757, #6464 ) ;
#20952 = EDGE_CURVE ( 'NONE', #13781, #53854, #53980, .T. ) ;
#20953 = EDGE_CURVE ( 'NONE', #12359, #15460, #53164, .T. ) ;
#20954 = EDGE_CURVE ( 'NONE', #37711, #40517, #32128, .T. ) ;
#20955 = VECTOR ( 'NONE', #23267, 999.9999999999998863 ) ;
#20956 = CARTESIAN_POINT ( 'NONE',  ( -19.12962290826653700, 0.000000000000000000, 14.40064212555863854 ) ) ;
#20957 = PLANE ( 'NONE',  #7617 ) ;
#20958 = CARTESIAN_POINT ( 'NONE',  ( 2.072287782118878319, 0.000000000000000000, -2.950529333540147015 ) ) ;
#20959 = CARTESIAN_POINT ( 'NONE',  ( -16.74767181305720953, -0.03228989815065406305, 3.385655385894552616 ) ) ;
#20960 = ORIENTED_EDGE ( 'NONE', *, *, #42029, .F. ) ;
#20961 = AXIS2_PLACEMENT_3D ( 'NONE', #10209, #5973, #23292 ) ;
#20962 = CARTESIAN_POINT ( 'NONE',  ( -9.775576553118467515, -0.04422114144963021354, 1.826781837067675607 ) ) ;
#20963 = CARTESIAN_POINT ( 'NONE',  ( -8.860905869600902207, 1.745854407020028306E-14, -3.600000000000000089 ) ) ;
#20964 = ORIENTED_EDGE ( 'NONE', *, *, #37671, .T. ) ;
#20965 = EDGE_LOOP ( 'NONE', ( #44638, #48074, #2492, #50252 ) ) ;
#20966 = DIRECTION ( 'NONE',  ( 0.6427681459581294776, -0.7660444431189769032, 0.005002170337467562802 ) ) ;
#20967 = EDGE_LOOP ( 'NONE', ( #1777, #54120, #42049, #28758 ) ) ;
#20968 = EDGE_CURVE ( 'NONE', #50902, #39023, #9985, .T. ) ;
#20969 = LINE ( 'NONE', #20423, #32018 ) ;
#20970 = EDGE_CURVE ( 'NONE', #20189, #38808, #44603, .T. ) ;
#20971 = ORIENTED_EDGE ( 'NONE', *, *, #22357, .T. ) ;
#20972 = ORIENTED_EDGE ( 'NONE', *, *, #6079, .F. ) ;
#20973 = VERTEX_POINT ( 'NONE', #36667 ) ;
#20974 = EDGE_CURVE ( 'NONE', #20246, #50299, #32425, .T. ) ;
#20975 = DIRECTION ( 'NONE',  ( 0.9999697198139515519, 0.000000000000000000, 0.007781995580013368816 ) ) ;
#20976 = CARTESIAN_POINT ( 'NONE',  ( -17.93139508144814442, 0.000000000000000000, 13.85596890686001537 ) ) ;
#20977 = CARTESIAN_POINT ( 'NONE',  ( -22.31155744454273915, -5.536956232915666298, 5.371229839343643953 ) ) ;
#20978 = VECTOR ( 'NONE', #53791, 999.9999999999998863 ) ;
#20979 = EDGE_CURVE ( 'NONE', #38944, #49575, #7679, .T. ) ;
#20980 = AXIS2_PLACEMENT_3D ( 'NONE', #46269, #42321, #3417 ) ;
#20981 = ORIENTED_EDGE ( 'NONE', *, *, #48281, .T. ) ;
#20982 = ORIENTED_EDGE ( 'NONE', *, *, #34269, .F. ) ;
#20983 = ADVANCED_FACE ( 'NONE', ( #25007 ), #7383, .F. ) ;
#20984 = AXIS2_PLACEMENT_3D ( 'NONE', #27105, #14341, #31654 ) ;
#20985 = DIRECTION ( 'NONE',  ( -0.5449076811759708816, 0.6444004775717707689, 0.5364919789714475140 ) ) ;
#20986 = CARTESIAN_POINT ( 'NONE',  ( -18.39746900504187010, 0.000000000000000000, 14.03700784672088808 ) ) ;
#20987 = ORIENTED_EDGE ( 'NONE', *, *, #12885, .F. ) ;
#20988 = LINE ( 'NONE', #29541, #47266 ) ;
#20989 = LINE ( 'NONE', #38612, #42234 ) ;
#20990 = EDGE_LOOP ( 'NONE', ( #151, #3676, #6147, #31369 ) ) ;
#20991 = CARTESIAN_POINT ( 'NONE',  ( -17.93139508144814442, 0.000000000000000000, 13.85596890686001537 ) ) ;
#20992 = CARTESIAN_POINT ( 'NONE',  ( -15.03495456790438389, -0.1191753592594197858, 12.77051346725278158 ) ) ;
#20993 = VERTEX_POINT ( 'NONE', #50268 ) ;
#20994 = PLANE ( 'NONE',  #23703 ) ;
#20995 = B_SPLINE_CURVE_WITH_KNOTS ( 'NONE', 3,
 ( #27879, #31575, #32418, #9719 ),
 .UNSPECIFIED., .F., .F.,
 ( 4, 4 ),
 ( 9.874130977897000849E-05, 0.0003960674641214396866 ),
 .UNSPECIFIED. ) ;
#20996 = AXIS2_PLACEMENT_3D ( 'NONE', #17286, #7666, #50808 ) ;
#20997 = CARTESIAN_POINT ( 'NONE',  ( -13.56399075187187542, -0.6798977022406560433, 2.128343463916670952 ) ) ;
#20998 = ORIENTED_EDGE ( 'NONE', *, *, #15867, .F. ) ;
#20999 = CYLINDRICAL_SURFACE ( 'NONE', #2242, 0.2499999999999998612 ) ;
#21000 = DIRECTION ( 'NONE',  ( -0.6427681459581293666, -0.7660444431189770143, -0.005002170337467561935 ) ) ;
#21001 = CARTESIAN_POINT ( 'NONE',  ( -10.28842178966973897, 0.000000000000000000, 0.8776935365639153552 ) ) ;
#21002 = DIRECTION ( 'NONE',  ( 0.7660212471507180654, -0.6427876096865404731, 0.005961354470445141482 ) ) ;
#21003 = ORIENTED_EDGE ( 'NONE', *, *, #56052, .T. ) ;
#21004 = DIRECTION ( 'NONE',  ( -0.6427681459581293666, -0.7660444431189770143, -0.005002170337467561935 ) ) ;
#21005 = DIRECTION ( 'NONE',  ( -0.6427681459581293666, -0.7660444431189770143, -0.005002170337467561935 ) ) ;
#21006 = CARTESIAN_POINT ( 'NONE',  ( -24.27063949748155380, 0.000000000000000000, 6.308861732390097288 ) ) ;
#21007 = DIRECTION ( 'NONE',  ( -0.005002170337468016433, -0.7660444431189770143, 0.6427681459581293666 ) ) ;
#21008 = LINE ( 'NONE', #26392, #14963 ) ;
#21009 = LINE ( 'NONE', #38338, #27004 ) ;
#21010 = CARTESIAN_POINT ( 'NONE',  ( -25.20278734466900517, 0.000000000000000000, 6.670939612111840944 ) ) ;
#21011 = VERTEX_POINT ( 'NONE', #46024 ) ;
#21012 = SHAPE_REPRESENTATION_RELATIONSHIP ( 'NONE' , 'NONE' ,  #55389, #49640 ) ;
#21013 = DIRECTION ( 'NONE',  ( -0.7660212471507179544, -0.6427876096865405842, -0.005961354470445141482 ) ) ;
#21014 = VERTEX_POINT ( 'NONE', #25288 ) ;
#21015 = PLANE ( 'NONE',  #27482 ) ;
#21016 = DIRECTION ( 'NONE',  ( -0.005961354470445682716, -0.6427876096865404731, 0.7660212471507180654 ) ) ;
#21017 = EDGE_CURVE ( 'NONE', #45314, #48949, #12216, .T. ) ;
#21018 = EDGE_CURVE ( 'NONE', #5914, #47750, #32955, .T. ) ;
#21019 = VECTOR ( 'NONE', #20889, 999.9999999999998863 ) ;
#21020 = VECTOR ( 'NONE', #26447, 1000.000000000000000 ) ;
#21021 = DIRECTION ( 'NONE',  ( 0.5364919789714477361, 0.6444004775717706579, 0.5449076811759711036 ) ) ;
#21022 = ADVANCED_FACE ( 'NONE', ( #3685 ), #24700, .F. ) ;
#21023 = PLANE ( 'NONE',  #11526 ) ;
#21024 = LINE ( 'NONE', #16782, #49230 ) ;
#21025 = VERTEX_POINT ( 'NONE', #51109 ) ;
#21026 = VECTOR ( 'NONE', #38635, 1000.000000000000114 ) ;
#21027 = EDGE_LOOP ( 'NONE', ( #47238, #39729, #22502, #48126 ) ) ;
#21028 = DIRECTION ( 'NONE',  ( -0.9999697198139514409, -0.000000000000000000, -0.007781995580013368816 ) ) ;
#21029 = LINE ( 'NONE', #8002, #39513 ) ;
#21030 = ORIENTED_EDGE ( 'NONE', *, *, #34115, .T. ) ;
#21031 = FACE_OUTER_BOUND ( 'NONE', #8325, .T. ) ;
#21032 = ORIENTED_EDGE ( 'NONE', *, *, #24847, .T. ) ;
#21033 = FACE_OUTER_BOUND ( 'NONE', #42936, .T. ) ;
#21034 = AXIS2_PLACEMENT_3D ( 'NONE', #28063, #15011, #28327 ) ;
#21035 = ORIENTED_EDGE ( 'NONE', *, *, #7350, .T. ) ;
#21036 = FACE_OUTER_BOUND ( 'NONE', #19459, .T. ) ;
#21037 = AXIS2_PLACEMENT_3D ( 'NONE', #31059, #20369, #37709 ) ;
#21038 = ORIENTED_EDGE ( 'NONE', *, *, #48409, .F. ) ;
#21039 = ORIENTED_EDGE ( 'NONE', *, *, #17021, .F. ) ;
#21040 = ORIENTED_EDGE ( 'NONE', *, *, #47652, .T. ) ;
#21041 = CARTESIAN_POINT ( 'NONE',  ( -12.43266248435915422, 0.000000000000000000, 8.047641899584064618 ) ) ;
#21042 = CARTESIAN_POINT ( 'NONE',  ( -18.56568686646327393, 0.000000000000000000, 9.846573634752608939 ) ) ;
#21043 = CARTESIAN_POINT ( 'NONE',  ( -15.46633387165207019, -0.1191753592594185784, 8.493368265297117858 ) ) ;
#21044 = LINE ( 'NONE', #7726, #34706 ) ;
#21045 = ORIENTED_EDGE ( 'NONE', *, *, #13245, .T. ) ;
#21046 = ORIENTED_EDGE ( 'NONE', *, *, #38593, .T. ) ;
#21047 = EDGE_CURVE ( 'NONE', #30203, #10825, #42330, .T. ) ;
#21048 = ORIENTED_EDGE ( 'NONE', *, *, #11715, .F. ) ;
#21049 = DIRECTION ( 'NONE',  ( -0.6427681459581293666, -0.7660444431189770143, -0.005002170337467561935 ) ) ;
#21050 = EDGE_CURVE ( 'NONE', #9472, #46146, #42024, .T. ) ;
#21051 = CARTESIAN_POINT ( 'NONE',  ( -17.26532721389163072, 0.000000000000000000, 13.67648636611514590 ) ) ;
#21052 = ORIENTED_EDGE ( 'NONE', *, *, #53929, .F. ) ;
#21053 = VECTOR ( 'NONE', #25791, 999.9999999999998863 ) ;
#21054 = LINE ( 'NONE', #46923, #5779 ) ;
#21055 = EDGE_CURVE ( 'NONE', #55340, #26051, #45724, .T. ) ;
#21056 = ORIENTED_EDGE ( 'NONE', *, *, #40344, .T. ) ;
#21057 = DIRECTION ( 'NONE',  ( 0.005002170337468016433, -0.7660444431189770143, -0.6427681459581293666 ) ) ;
#21058 = DIRECTION ( 'NONE',  ( -0.8531650599175529814, -0.4028455766673920135, 0.3313982828793697877 ) ) ;
#21059 = VECTOR ( 'NONE', #44105, 1000.000000000000114 ) ;
#21060 = VECTOR ( 'NONE', #17299, 1000.000000000000227 ) ;
#21061 = EDGE_LOOP ( 'NONE', ( #12630, #13938, #4341, #41164 ) ) ;
#21062 = ADVANCED_FACE ( 'NONE', ( #33517 ), #24172, .F. ) ;
#21063 = CARTESIAN_POINT ( 'NONE',  ( -18.35493042423798471, 0.000000000000000000, 8.570891567112456144 ) ) ;
#21064 = ORIENTED_EDGE ( 'NONE', *, *, #2853, .F. ) ;
#21065 = AXIS2_PLACEMENT_3D ( 'NONE', #20897, #37959, #42216 ) ;
#21066 = DIRECTION ( 'NONE',  ( 0.007781995580012663651, 0.000000000000000000, -0.9999697198139515519 ) ) ;
#21067 = DIRECTION ( 'NONE',  ( -0.2426528472758542054, 0.7422098413412800966, -0.6246952433987894571 ) ) ;
#21068 = AXIS2_PLACEMENT_3D ( 'NONE', #2573, #2829, #11088 ) ;
#21069 = ORIENTED_EDGE ( 'NONE', *, *, #24405, .F. ) ;
#21070 = PLANE ( 'NONE',  #17804 ) ;
#21071 = DIRECTION ( 'NONE',  ( 0.005002170337468016433, -0.7660444431189770143, -0.6427681459581293666 ) ) ;
#21072 = DIRECTION ( 'NONE',  ( 0.9659258262890692004, -0.2588190451025176864, 0.000000000000000000 ) ) ;
#21073 = PLANE ( 'NONE',  #51829 ) ;
#21074 = EDGE_LOOP ( 'NONE', ( #36110, #20166, #28273, #56072 ) ) ;
#21075 = DIRECTION ( 'NONE',  ( -0.9999697198139514409, -0.000000000000000000, -0.007781995580013368816 ) ) ;
#21076 = CARTESIAN_POINT ( 'NONE',  ( -68.07189119022113744, 1.958909493320992512, 7.460396425438592161 ) ) ;
#21077 = AXIS2_PLACEMENT_3D ( 'NONE', #4959, #953, #43320 ) ;
#21078 = DIRECTION ( 'NONE',  ( 0.007781995580012662783, 0.000000000000000000, -0.9999697198139514409 ) ) ;
#21079 = DIRECTION ( 'NONE',  ( -0.005002170337468016433, -0.7660444431189770143, 0.6427681459581293666 ) ) ;
#21080 = CARTESIAN_POINT ( 'NONE',  ( -12.60458797795435615, 0.000000000000000000, 11.86609696750642229 ) ) ;
#21081 = FACE_OUTER_BOUND ( 'NONE', #23580, .T. ) ;
#21082 = ORIENTED_EDGE ( 'NONE', *, *, #53470, .T. ) ;
#21083 = CARTESIAN_POINT ( 'NONE',  ( -21.47263955680318404, 0.000000000000000000, 5.022634149262071190 ) ) ;
#21084 = CARTESIAN_POINT ( 'NONE',  ( -17.74404816805336793, 0.000000000000000000, 3.574322630375089460 ) ) ;
#21085 = CARTESIAN_POINT ( 'NONE',  ( -15.82312983555391206, 0.000000000000000000, 7.482598415295212746 ) ) ;
#21086 = EDGE_LOOP ( 'NONE', ( #2954, #51635, #44202, #35934 ) ) ;
#21087 = CARTESIAN_POINT ( 'NONE',  ( -14.53902905116009947, -2.946525016555661125, 2.434764173376773755 ) ) ;
#21088 = VERTEX_POINT ( 'NONE', #24427 ) ;
#21089 = EDGE_CURVE ( 'NONE', #54842, #44961, #2827, .T. ) ;
#21090 = CARTESIAN_POINT ( 'NONE',  ( -57.29829478218162109, -10.27834239552269757, 4.211285351864063224E-15 ) ) ;
#21091 = CARTESIAN_POINT ( 'NONE',  ( -21.47263955680318404, 0.000000000000000000, 5.022634149262071190 ) ) ;
#21092 = AXIS2_PLACEMENT_3D ( 'NONE', #48411, #9817, #27122 ) ;
#21093 = ADVANCED_FACE ( 'NONE', ( #20152 ), #54807, .F. ) ;
#21094 = EDGE_CURVE ( 'NONE', #28463, #45380, #41487, .T. ) ;
#21095 = CARTESIAN_POINT ( 'NONE',  ( -8.929802727318762123, -0.1191753592594179401, 4.481584294213840636 ) ) ;
#21096 = CARTESIAN_POINT ( 'NONE',  ( -67.51160766412522207, 1.999999999982350785, 2.764386752165123085 ) ) ;
#21097 = VERTEX_POINT ( 'NONE', #46564 ) ;
#21098 = VERTEX_POINT ( 'NONE', #15919 ) ;
#21099 = CARTESIAN_POINT ( 'NONE',  ( -10.47421230394850866, 0.000000000000000000, 10.95934586908605723 ) ) ;
#21100 = CARTESIAN_POINT ( 'NONE',  ( -10.19575411036579915, 0.000000000000000000, 0.8784146978715680065 ) ) ;
#21101 = VECTOR ( 'NONE', #17149, 1000.000000000000000 ) ;
#21102 = LINE ( 'NONE', #43801, #33236 ) ;
#21103 = AXIS2_PLACEMENT_3D ( 'NONE', #46444, #11563, #54691 ) ;
#21104 = DIRECTION ( 'NONE',  ( 0.5364919789714477361, 0.6444004775717706579, 0.5449076811759711036 ) ) ;
#21105 = VECTOR ( 'NONE', #33399, 999.9999999999998863 ) ;
#21106 = CARTESIAN_POINT ( 'NONE',  ( -12.10160420820394478, 0.000000000000000000, 6.942222062218735168 ) ) ;
#21107 = CARTESIAN_POINT ( 'NONE',  ( -6.110905869600904872, 1.712176620043476140E-14, -4.599999999999999645 ) ) ;
#21108 = EDGE_LOOP ( 'NONE', ( #22487, #54146, #1424, #5184 ) ) ;
#21109 = CARTESIAN_POINT ( 'NONE',  ( -16.81190032086591302, 0.000000000000000000, 3.212244750653343583 ) ) ;
#21110 = EDGE_CURVE ( 'NONE', #5924, #27743, #32669, .T. ) ;
#21111 = CARTESIAN_POINT ( 'NONE',  ( -16.33317936670417225, 0.000000000000000000, 13.31440848639340224 ) ) ;
#21112 = VECTOR ( 'NONE', #675, 1000.000000000000000 ) ;
#21113 = CARTESIAN_POINT ( 'NONE',  ( -15.87975247367846166, 0.000000000000000000, 2.850166870931599927 ) ) ;
#21114 = AXIS2_PLACEMENT_3D ( 'NONE', #40545, #14137, #17838 ) ;
#21115 = VERTEX_POINT ( 'NONE', #20458 ) ;
#21116 = LINE ( 'NONE', #35057, #30207 ) ;
#21117 = DIRECTION ( 'NONE',  ( -0.7660212471507179544, -0.6427876096865405842, -0.005961354470445141482 ) ) ;
#21118 = DIRECTION ( 'NONE',  ( -0.6427681459581293666, -0.7660444431189770143, -0.005002170337467561935 ) ) ;
#21119 = VERTEX_POINT ( 'NONE', #37797 ) ;
#21120 = DIRECTION ( 'NONE',  ( 0.000000000000000000, 0.000000000000000000, 1.000000000000000000 ) ) ;
#21121 = AXIS2_PLACEMENT_3D ( 'NONE', #9344, #9075, #49375 ) ;
#21122 = ORIENTED_EDGE ( 'NONE', *, *, #3788, .F. ) ;
#21123 = VECTOR ( 'NONE', #18187, 999.9999999999998863 ) ;
#21124 = ORIENTED_EDGE ( 'NONE', *, *, #42297, .T. ) ;
#21125 = ORIENTED_EDGE ( 'NONE', *, *, #4786, .F. ) ;
#21126 = VERTEX_POINT ( 'NONE', #55107 ) ;
#21127 = DIRECTION ( 'NONE',  ( 0.7660212471507180654, -0.6427876096865404731, 0.005961354470445141482 ) ) ;
#21128 = EDGE_LOOP ( 'NONE', ( #15248, #34567, #50095, #828 ) ) ;
#21129 = VECTOR ( 'NONE', #9794, 1000.000000000000114 ) ;
#21130 = PLANE ( 'NONE',  #34003 ) ;
#21131 = ORIENTED_EDGE ( 'NONE', *, *, #5360, .F. ) ;
#21132 = CARTESIAN_POINT ( 'NONE',  ( -14.43496725204122377, 0.000000000000000000, 8.232065557114770726 ) ) ;
#21133 = EDGE_CURVE ( 'NONE', #18997, #19093, #38057, .T. ) ;
#21134 = VERTEX_POINT ( 'NONE', #55364 ) ;
#21135 = VECTOR ( 'NONE', #19653, 1000.000000000000227 ) ;
#21136 = ORIENTED_EDGE ( 'NONE', *, *, #24040, .T. ) ;
#21137 = CARTESIAN_POINT ( 'NONE',  ( -18.79944894654208909, 0.000000000000000000, 5.982107732540097089 ) ) ;
#21138 = LINE ( 'NONE', #3548, #52244 ) ;
#21139 = DIRECTION ( 'NONE',  ( 0.5364919789714477361, 0.6444004775717706579, 0.5449076811759711036 ) ) ;
#21140 = LINE ( 'NONE', #8104, #54080 ) ;
#21141 = AXIS2_PLACEMENT_3D ( 'NONE', #16796, #46908, #8008 ) ;
#21142 = DIRECTION ( 'NONE',  ( 0.5449076811759707706, 0.6444004775717708799, -0.5364919789714476250 ) ) ;
#21143 = ORIENTED_EDGE ( 'NONE', *, *, #34652, .T. ) ;
#21144 = EDGE_CURVE ( 'NONE', #23572, #55568, #16460, .T. ) ;
#21145 = AXIS2_PLACEMENT_3D ( 'NONE', #48133, #25730, #39653 ) ;
#21146 = VECTOR ( 'NONE', #45267, 1000.000000000000227 ) ;
#21147 = EDGE_LOOP ( 'NONE', ( #31251, #25114, #24414, #22015 ) ) ;
#21148 = FACE_OUTER_BOUND ( 'NONE', #52370, .T. ) ;
#21149 = DIRECTION ( 'NONE',  ( -0.2588190451025212946, -0.9659258262890680902, 0.000000000000000000 ) ) ;
#21150 = UNCERTAINTY_MEASURE_WITH_UNIT (LENGTH_MEASURE( 1.000000000000000082E-05 ), #37557, 'distance_accuracy_value', 'NONE');
#21151 = EDGE_CURVE ( 'NONE', #26046, #294, #4282, .T. ) ;
#21152 = EDGE_CURVE ( 'NONE', #11770, #27552, #12513, .T. ) ;
#21153 = CARTESIAN_POINT ( 'NONE',  ( -5.876231750791062858, 5.744269837952261426, 5.500901545341295495 ) ) ;
#21154 = AXIS2_PLACEMENT_3D ( 'NONE', #28381, #6822, #2267 ) ;
#21155 = AXIS2_PLACEMENT_3D ( 'NONE', #20321, #13151, #21395 ) ;
#21156 = DIRECTION ( 'NONE',  ( 0.000000000000000000, -0.000000000000000000, -1.000000000000000000 ) ) ;
#21157 = DIRECTION ( 'NONE',  ( -0.5364919789714478471, 0.6444004775717705469, -0.5449076811759709926 ) ) ;
#21158 = PLANE ( 'NONE',  #21437 ) ;
#21159 = ORIENTED_EDGE ( 'NONE', *, *, #35731, .F. ) ;
#21160 = DIRECTION ( 'NONE',  ( 0.005002170337468016433, -0.7660444431189770143, -0.6427681459581293666 ) ) ;
#21161 = EDGE_CURVE ( 'NONE', #13455, #49751, #34625, .T. ) ;
#21162 = FACE_OUTER_BOUND ( 'NONE', #54702, .T. ) ;
#21163 = ORIENTED_EDGE ( 'NONE', *, *, #15678, .T. ) ;
#21164 = DIRECTION ( 'NONE',  ( 0.7660212471507180654, -0.6427876096865404731, 0.005961354470445141482 ) ) ;
#21165 = FACE_OUTER_BOUND ( 'NONE', #743, .T. ) ;
#21166 = EDGE_CURVE ( 'NONE', #38597, #5370, #9348, .T. ) ;
#21167 = LINE ( 'NONE', #33407, #33210 ) ;
#21168 = EDGE_CURVE ( 'NONE', #1327, #51910, #9078, .T. ) ;
#21169 = DIRECTION ( 'NONE',  ( -0.6427681459581293666, -0.7660444431189770143, -0.005002170337467561935 ) ) ;
#21170 = ORIENTED_EDGE ( 'NONE', *, *, #9337, .F. ) ;
#21171 = EDGE_LOOP ( 'NONE', ( #51105, #12365, #9778, #27878 ) ) ;
#21172 = DIRECTION ( 'NONE',  ( 0.007781995580012662783, 0.000000000000000000, -0.9999697198139514409 ) ) ;
#21173 = CARTESIAN_POINT ( 'NONE',  ( -15.15583128246454336, -0.3560938001956568399, 2.756999424905611118 ) ) ;
#21174 = PLANE ( 'NONE',  #683 ) ;
#21175 = VECTOR ( 'NONE', #8035, 999.9999999999998863 ) ;
#21176 = EDGE_CURVE ( 'NONE', #18261, #51932, #21596, .T. ) ;
#21177 = FACE_OUTER_BOUND ( 'NONE', #44354, .T. ) ;
#21178 = DIRECTION ( 'NONE',  ( 0.000000000000000000, -0.000000000000000000, -1.000000000000000000 ) ) ;
#21179 = VECTOR ( 'NONE', #21877, 999.9999999999998863 ) ;
#21180 = DIRECTION ( 'NONE',  ( 0.5449076811759707706, 0.6444004775717708799, -0.5364919789714476250 ) ) ;
#21181 = CARTESIAN_POINT ( 'NONE',  ( -15.14840367773380336, 1.743523803501505709, 5.626895143433455537 ) ) ;
#21182 = ADVANCED_FACE ( 'NONE', ( #56212 ), #55653, .F. ) ;
#21183 = PLANE ( 'NONE',  #35963 ) ;
#21184 = CARTESIAN_POINT ( 'NONE',  ( -69.94833770632727976, -8.709315162003530730, 7.852029984319920608 ) ) ;
#21185 = AXIS2_PLACEMENT_3D ( 'NONE', #4099, #21427, #42148 ) ;
#21186 = DIRECTION ( 'NONE',  ( -0.5364919789714478471, 0.6444004775717705469, -0.5449076811759709926 ) ) ;
#21187 = VERTEX_POINT ( 'NONE', #43440 ) ;
#21188 = DIRECTION ( 'NONE',  ( 0.5364919789714477361, 0.6444004775717706579, 0.5449076811759711036 ) ) ;
#21189 = AXIS2_PLACEMENT_3D ( 'NONE', #42652, #17112, #21071 ) ;
#21190 = AXIS2_PLACEMENT_3D ( 'NONE', #52472, #30334, #38570 ) ;
#21191 = EDGE_LOOP ( 'NONE', ( #6893, #4331, #29365, #40389 ) ) ;
#21192 = EDGE_LOOP ( 'NONE', ( #55083, #50001, #7037, #22901 ) ) ;
#21193 = VECTOR ( 'NONE', #47383, 1000.000000000000000 ) ;
#21194 = ORIENTED_EDGE ( 'NONE', *, *, #3479, .T. ) ;
#21195 = ORIENTED_EDGE ( 'NONE', *, *, #48716, .T. ) ;
#21196 = VECTOR ( 'NONE', #52795, 1000.000000000000227 ) ;
#21197 = ORIENTED_EDGE ( 'NONE', *, *, #22608, .F. ) ;
#21198 = ORIENTED_EDGE ( 'NONE', *, *, #49992, .T. ) ;
#21199 = CARTESIAN_POINT ( 'NONE',  ( -21.65435634735958104, -3.594132820645660420, 10.99180339266565376 ) ) ;
#21200 = DIRECTION ( 'NONE',  ( 0.7660212471507180654, -0.6427876096865404731, 0.005961354470445141482 ) ) ;
#21201 = DIRECTION ( 'NONE',  ( 0.9999697198139515519, 0.000000000000000000, 0.007781995580013368816 ) ) ;
#21202 = ORIENTED_EDGE ( 'NONE', *, *, #14387, .F. ) ;
#21203 = CARTESIAN_POINT ( 'NONE',  ( -24.26986129792355129, -0.1191753592594197858, 6.208864760408702388 ) ) ;
#21204 = EDGE_CURVE ( 'NONE', #14373, #51521, #21845, .T. ) ;
#21205 = ORIENTED_EDGE ( 'NONE', *, *, #4579, .F. ) ;
#21206 = LINE ( 'NONE', #20067, #10510 ) ;
#21207 = ORIENTED_EDGE ( 'NONE', *, *, #19893, .T. ) ;
#21208 = CARTESIAN_POINT ( 'NONE',  ( -11.23286883698721006, -0.1191753592594199940, 1.878336812569445957 ) ) ;
#21209 = AXIS2_PLACEMENT_3D ( 'NONE', #3185, #19383, #29307 ) ;
#21210 = LINE ( 'NONE', #4200, #26476 ) ;
#21211 = DIRECTION ( 'NONE',  ( -0.3620778797217456546, 0.000000000000000000, -0.9321478471874540261 ) ) ;
#21212 = ORIENTED_EDGE ( 'NONE', *, *, #47646, .T. ) ;
#21213 = DIRECTION ( 'NONE',  ( -0.005961354470445682716, -0.6427876096865404731, 0.7660212471507180654 ) ) ;
#21214 = AXIS2_PLACEMENT_3D ( 'NONE', #41554, #33031, #32738 ) ;
#21215 = ORIENTED_EDGE ( 'NONE', *, *, #28039, .T. ) ;
#21216 = EDGE_CURVE ( 'NONE', #42837, #37228, #17050, .T. ) ;
#21217 = CARTESIAN_POINT ( 'NONE',  ( 2.072287782118878319, 0.000000000000000000, -2.950529333540147015 ) ) ;
#21219 = VECTOR ( 'NONE', #5586, 999.9999999999998863 ) ;
#21218 = PLANE ( 'NONE',  #43878 ) ;
#21220 = EDGE_CURVE ( 'NONE', #2279, #41786, #43994, .T. ) ;
#21221 = CARTESIAN_POINT ( 'NONE',  ( -28.93060053386082231, -0.1191753592594197858, 8.019254159017428663 ) ) ;
#21222 = DIRECTION ( 'NONE',  ( 0.6427681459581294776, -0.7660444431189769032, 0.005002170337467562802 ) ) ;
#21223 = DIRECTION ( 'NONE',  ( -0.005002170337468016433, -0.7660444431189770143, 0.6427681459581293666 ) ) ;
#21224 = DIRECTION ( 'NONE',  ( 0.9999697198139515519, 0.000000000000000000, 0.007781995580013368816 ) ) ;
#21225 = CARTESIAN_POINT ( 'NONE',  ( -12.19881617777849492, 3.200641362704007786, 6.872553345591845719 ) ) ;
#21226 = AXIS2_PLACEMENT_3D ( 'NONE', #870, #21636, #38949 ) ;
#21227 = LINE ( 'NONE', #38558, #49485 ) ;
#21228 = ORIENTED_EDGE ( 'NONE', *, *, #10419, .F. ) ;
#21229 = CARTESIAN_POINT ( 'NONE',  ( -17.74404816805336793, 0.000000000000000000, 3.574322630375089460 ) ) ;
#21230 = VERTEX_POINT ( 'NONE', #52250 ) ;
#21231 = AXIS2_PLACEMENT_3D ( 'NONE', #28713, #45190, #6849 ) ;
#21232 = LINE ( 'NONE', #47647, #47381 ) ;
#21233 = FACE_OUTER_BOUND ( 'NONE', #29297, .T. ) ;
#21234 = EDGE_CURVE ( 'NONE', #25987, #33400, #22903, .T. ) ;
#21235 = DIRECTION ( 'NONE',  ( 0.007781995580012663651, 0.000000000000000000, -0.9999697198139515519 ) ) ;
#21236 = DIRECTION ( 'NONE',  ( 0.5449076811759707706, 0.6444004775717708799, -0.5364919789714476250 ) ) ;
#21237 = CARTESIAN_POINT ( 'NONE',  ( 2.072287782118878319, 0.000000000000000000, -2.950529333540147015 ) ) ;
#21238 = EDGE_CURVE ( 'NONE', #13281, #34911, #39468, .T. ) ;
#21239 = VECTOR ( 'NONE', #53861, 1000.000000000000227 ) ;
#21240 = PLANE ( 'NONE',  #19232 ) ;
#21241 = VECTOR ( 'NONE', #11554, 999.9999999999998863 ) ;
#21242 = VERTEX_POINT ( 'NONE', #5117 ) ;
#21243 = LINE ( 'NONE', #47659, #18443 ) ;
#21244 = CARTESIAN_POINT ( 'NONE',  ( -15.88053067323646417, -0.1191753592594197858, 2.950163842912994383 ) ) ;
#21245 = CARTESIAN_POINT ( 'NONE',  ( -13.27065584551087163, 0.000000000000000000, 12.04557950825129176 ) ) ;
#21246 = EDGE_CURVE ( 'NONE', #21762, #41020, #47131, .T. ) ;
#21247 = PLANE ( 'NONE',  #2805 ) ;
#21248 = CARTESIAN_POINT ( 'NONE',  ( -17.74560456716937296, 0.000000000000000000, 3.774316574337878372 ) ) ;
#21249 = DIRECTION ( 'NONE',  ( 0.000000000000000000, -1.000000000000000000, 0.000000000000000000 ) ) ;
#21250 = DIRECTION ( 'NONE',  ( 0.005002170337468016433, -0.7660444431189770143, -0.6427681459581293666 ) ) ;
#21251 = ORIENTED_EDGE ( 'NONE', *, *, #35218, .T. ) ;
#21252 = AXIS2_PLACEMENT_3D ( 'NONE', #6544, #19880, #37199 ) ;
#21253 = EDGE_CURVE ( 'NONE', #22669, #48082, #25549, .T. ) ;
#21254 = LINE ( 'NONE', #26100, #1294 ) ;
#21255 = DIRECTION ( 'NONE',  ( 0.000000000000000000, -0.000000000000000000, -1.000000000000000000 ) ) ;
#21256 = VERTEX_POINT ( 'NONE', #17597 ) ;
#21257 = AXIS2_PLACEMENT_3D ( 'NONE', #27876, #1718, #41726 ) ;
#21258 = ORIENTED_EDGE ( 'NONE', *, *, #30289, .T. ) ;
#21259 = DIRECTION ( 'NONE',  ( -0.5449076811759708816, 0.6444004775717707689, 0.5364919789714475140 ) ) ;
#21260 = VECTOR ( 'NONE', #15359, 1000.000000000000000 ) ;
#21261 = ORIENTED_EDGE ( 'NONE', *, *, #10829, .F. ) ;
#21262 = ORIENTED_EDGE ( 'NONE', *, *, #16674, .F. ) ;
#21263 = VERTEX_POINT ( 'NONE', #12774 ) ;
#21264 = VECTOR ( 'NONE', #8960, 1000.000000000000000 ) ;
#21265 = EDGE_LOOP ( 'NONE', ( #6260, #40670, #28460, #43579 ) ) ;
#21266 = DIRECTION ( 'NONE',  ( 0.5364919789714477361, 0.6444004775717706579, 0.5449076811759711036 ) ) ;
#21267 = AXIS2_PLACEMENT_3D ( 'NONE', #13588, #26647, #52753 ) ;
#21268 = EDGE_LOOP ( 'NONE', ( #36288, #45415, #37124, #1368 ) ) ;
#21269 = CARTESIAN_POINT ( 'NONE',  ( -19.72716634110825851, 0.000000000000000000, 5.774881965041287479 ) ) ;
#21270 = DIRECTION ( 'NONE',  ( -0.5364919789714478471, 0.6444004775717705469, -0.5449076811759709926 ) ) ;
#21271 = VECTOR ( 'NONE', #51611, 999.9999999999998863 ) ;
#21272 = EDGE_LOOP ( 'NONE', ( #41481, #2090, #15399, #50092 ) ) ;
#21274 = ORIENTED_EDGE ( 'NONE', *, *, #49981, .F. ) ;
#21273 = EDGE_CURVE ( 'NONE', #5706, #6174, #47712, .T. ) ;
#21275 = VECTOR ( 'NONE', #29926, 1000.000000000000114 ) ;
#21276 = VECTOR ( 'NONE', #26219, 1000.000000000000227 ) ;
#21277 = EDGE_CURVE ( 'NONE', #26788, #15460, #21298, .T. ) ;
#21278 = CARTESIAN_POINT ( 'NONE',  ( -13.21518402393321168, 0.000000000000000000, 4.917569563982915781 ) ) ;
#21279 = DIRECTION ( 'NONE',  ( 0.5364919789714477361, 0.6444004775717706579, 0.5449076811759711036 ) ) ;
#21281 = EDGE_CURVE ( 'NONE', #35085, #21351, #34935, .T. ) ;
#21280 = ORIENTED_EDGE ( 'NONE', *, *, #40021, .T. ) ;
#21282 = CARTESIAN_POINT ( 'NONE',  ( 2.072287782118878319, 0.000000000000000000, -2.950529333540147015 ) ) ;
#21283 = CARTESIAN_POINT ( 'NONE',  ( -17.29039281695302677, -0.1191753592594170658, 4.047188179131904207 ) ) ;
#21284 = ORIENTED_EDGE ( 'NONE', *, *, #31045, .T. ) ;
#21285 = FACE_OUTER_BOUND ( 'NONE', #44313, .T. ) ;
#21286 = EDGE_CURVE ( 'NONE', #44937, #16954, #51669, .T. ) ;
#21287 = EDGE_CURVE ( 'NONE', #47771, #48446, #26131, .T. ) ;
#21288 = ADVANCED_FACE ( 'NONE', ( #27232 ), #36065, .F. ) ;
#21289 = ORIENTED_EDGE ( 'NONE', *, *, #19519, .F. ) ;
#21290 = DIRECTION ( 'NONE',  ( 0.000000000000000000, -0.000000000000000000, -1.000000000000000000 ) ) ;
#21291 = VECTOR ( 'NONE', #18377, 1000.000000000000227 ) ;
#21292 = DIRECTION ( 'NONE',  ( 0.9999697198139515519, 0.000000000000000000, 0.007781995580013368816 ) ) ;
#21293 = ORIENTED_EDGE ( 'NONE', *, *, #12054, .T. ) ;
#21294 = FACE_OUTER_BOUND ( 'NONE', #24003, .T. ) ;
#21295 = CARTESIAN_POINT ( 'NONE',  ( -10.47421230394850866, 0.000000000000000000, 10.95934586908605723 ) ) ;
#21297 = VECTOR ( 'NONE', #43369, 1000.000000000000227 ) ;
#21296 = LINE ( 'NONE', #51108, #47503 ) ;
#21298 = LINE ( 'NONE', #38630, #32858 ) ;
#21299 = VERTEX_POINT ( 'NONE', #10190 ) ;
#21300 = AXIS2_PLACEMENT_3D ( 'NONE', #6498, #32614, #49382 ) ;
#21301 = CARTESIAN_POINT ( 'NONE',  ( -16.89925026227929195, -0.1191753592594197858, 13.49466922669627422 ) ) ;
#21302 = DIRECTION ( 'NONE',  ( -0.8531650599175527594, 0.4028455766673922356, 0.3313982828793700652 ) ) ;
#21303 = CARTESIAN_POINT ( 'NONE',  ( -14.01545677930355183, 0.000000000000000000, 2.126011111488108174 ) ) ;
#21304 = ADVANCED_FACE ( 'NONE', ( #49672 ), #10495, .F. ) ;
#21305 = AXIS2_PLACEMENT_3D ( 'NONE', #41421, #2757, #49083 ) ;
#21306 = LINE ( 'NONE', #34372, #42222 ) ;
#21307 = DIRECTION ( 'NONE',  ( 0.5449076811759707706, 0.6444004775717708799, -0.5364919789714476250 ) ) ;
#21308 = LINE ( 'NONE', #34375, #17069 ) ;
#21309 = EDGE_CURVE ( 'NONE', #5703, #32241, #23274, .T. ) ;
#21311 = VECTOR ( 'NONE', #14022, 1000.000000000000227 ) ;
#21310 = CARTESIAN_POINT ( 'NONE',  ( -18.67619601524082285, 0.000000000000000000, 3.936400510096834893 ) ) ;
#21312 = CARTESIAN_POINT ( 'NONE',  ( -19.12962290826653700, 0.000000000000000000, 14.40064212555863854 ) ) ;
#21313 = VECTOR ( 'NONE', #49799, 1000.000000000000114 ) ;
#21314 = ORIENTED_EDGE ( 'NONE', *, *, #47960, .T. ) ;
#21315 = ADVANCED_FACE ( 'NONE', ( #22977 ), #14732, .F. ) ;
#21317 = DIRECTION ( 'NONE',  ( 0.000000000000000000, -1.000000000000000000, 0.000000000000000000 ) ) ;
#21316 = AXIS2_PLACEMENT_3D ( 'NONE', #42609, #42888, #34114 ) ;
#21318 = VERTEX_POINT ( 'NONE', #35471 ) ;
#21319 = VECTOR ( 'NONE', #37542, 1000.000000000000000 ) ;
#21320 = CARTESIAN_POINT ( 'NONE',  ( -13.17065887352947762, -0.1191753592594197858, 12.04635770780929427 ) ) ;
#21321 = LINE ( 'NONE', #3993, #9133 ) ;
#21322 = VECTOR ( 'NONE', #48314, 999.9999999999998863 ) ;
#21323 = ADVANCED_FACE ( 'NONE', ( #26975 ), #5954, .F. ) ;
#21324 = DIRECTION ( 'NONE',  ( 0.6427681459581294776, -0.7660444431189769032, 0.005002170337467562802 ) ) ;
#21325 = LINE ( 'NONE', #4837, #45059 ) ;
#21326 = CARTESIAN_POINT ( 'NONE',  ( -24.87971537937347932, 18.22038179169711825, 4.563126927700496438 ) ) ;
#21327 = VERTEX_POINT ( 'NONE', #1671 ) ;
#21328 = CIRCLE ( 'NONE', #8649, 3.000000000000001332 ) ;
#21329 = AXIS2_PLACEMENT_3D ( 'NONE', #42185, #51271, #15774 ) ;
#21330 = EDGE_LOOP ( 'NONE', ( #40887, #36798, #14100 ) ) ;
#21331 = CARTESIAN_POINT ( 'NONE',  ( -19.45503627000849889, 0.000000000000000000, 7.556996783084074742 ) ) ;
#21332 = CARTESIAN_POINT ( 'NONE',  ( -15.40103151951671734, 0.000000000000000000, 12.95233060667165681 ) ) ;
#21333 = ORIENTED_EDGE ( 'NONE', *, *, #16732, .F. ) ;
#21334 = PLANE ( 'NONE',  #15694 ) ;
#21335 = ORIENTED_EDGE ( 'NONE', *, *, #11641, .F. ) ;
#21336 = LINE ( 'NONE', #9385, #36782 ) ;
#21337 = ORIENTED_EDGE ( 'NONE', *, *, #11569, .F. ) ;
#21338 = DIRECTION ( 'NONE',  ( -0.9999697198139514409, -0.000000000000000000, -0.007781995580013368816 ) ) ;
#21339 = VECTOR ( 'NONE', #19980, 999.9999999999998863 ) ;
#21340 = ORIENTED_EDGE ( 'NONE', *, *, #20318, .F. ) ;
#21341 = VERTEX_POINT ( 'NONE', #40007 ) ;
#21342 = ORIENTED_EDGE ( 'NONE', *, *, #13506, .T. ) ;
#21343 = AXIS2_PLACEMENT_3D ( 'NONE', #49290, #22622, #18073 ) ;
#21344 = DIRECTION ( 'NONE',  ( -0.9321478471874540261, 0.000000000000000000, 0.3620778797217457656 ) ) ;
#21345 = CARTESIAN_POINT ( 'NONE',  ( -13.07066190154808361, 0.000000000000000000, 12.04713590736729678 ) ) ;
#21346 = AXIS2_PLACEMENT_3D ( 'NONE', #48175, #43927, #22378 ) ;
#21347 = LINE ( 'NONE', #16506, #51134 ) ;
#21348 = DIRECTION ( 'NONE',  ( -0.7660212471507179544, -0.6427876096865405842, -0.005961354470445141482 ) ) ;
#21349 = VERTEX_POINT ( 'NONE', #48540 ) ;
#21350 = VECTOR ( 'NONE', #26074, 1000.000000000000227 ) ;
#21351 = VERTEX_POINT ( 'NONE', #53086 ) ;
#21352 = VERTEX_POINT ( 'NONE', #13886 ) ;
#21353 = VECTOR ( 'NONE', #11143, 1000.000000000000227 ) ;
#21354 = EDGE_CURVE ( 'NONE', #16343, #547, #18998, .T. ) ;
#21355 = CARTESIAN_POINT ( 'NONE',  ( 1.969897575278193980, 0.000000000000000000, 10.20639235748909890 ) ) ;
#21356 = AXIS2_PLACEMENT_3D ( 'NONE', #47320, #52915, #5785 ) ;
#21357 = DIRECTION ( 'NONE',  ( -0.5364919789714478471, 0.6444004775717705469, -0.5449076811759709926 ) ) ;
#21358 = ORIENTED_EDGE ( 'NONE', *, *, #22608, .T. ) ;
#21359 = CYLINDRICAL_SURFACE ( 'NONE', #45686, 2.000000000000000888 ) ;
#21360 = EDGE_LOOP ( 'NONE', ( #12050, #25231, #10862, #43873 ) ) ;
#21361 = LINE ( 'NONE', #51719, #43248 ) ;
#21362 = FACE_OUTER_BOUND ( 'NONE', #20793, .T. ) ;
#21363 = VECTOR ( 'NONE', #25238, 999.9999999999998863 ) ;
#21364 = EDGE_CURVE ( 'NONE', #13391, #12878, #14464, .T. ) ;
#21365 = EDGE_CURVE ( 'NONE', #48176, #14783, #1093, .T. ) ;
#21366 = VERTEX_POINT ( 'NONE', #52781 ) ;
#21367 = AXIS2_PLACEMENT_3D ( 'NONE', #1776, #23641, #27934 ) ;
#21368 = DIRECTION ( 'NONE',  ( 0.5449076811759707706, 0.6444004775717708799, -0.5364919789714476250 ) ) ;
#21369 = EDGE_LOOP ( 'NONE', ( #30840, #43667, #51426, #50320, #7839, #24491, #21052, #55924, #44420, #39875, #55330, #12686, #38419, #42308, #48450, #19436, #20797, #9705, #32663, #5853, #36046, #25677, #54638, #16106, #51685, #42957, #5458, #44763, #14521, #2425, #1088, #10158, #24538, #14507, #50578, #20981, #14576, #29972, #18704, #6573, #42783, #31270, #20783, #27623, #41767, #30453, #37209, #42503, #7757, #18129, #31606, #38529, #55354, #31558, #9211, #8082, #38206, #53783, #17196, #14683, #31810, #43297, #16148, #19670, #7050, #10317, #23383, #31771, #30671, #54959, #52578, #1264, #5116, #35658, #49124, #16280, #5154, #3776, #47758, #2022, #4155, #13805, #53906, #9854, #7509, #39294, #14698, #22419, #50610, #26041, #39512, #55026, #54869, #27570, #24295, #23701, #3124, #20198, #2511, #13790, #41552, #49317, #41710, #19664, #6329, #3942, #7511 ) ) ;
#21370 = ADVANCED_FACE ( 'NONE', ( #27822 ), #31522, .F. ) ;
#21371 = VECTOR ( 'NONE', #26790, 1000.000000000000227 ) ;
#21372 = PLANE ( 'NONE',  #39161 ) ;
#21373 = AXIS2_PLACEMENT_3D ( 'NONE', #24249, #19966, #50359 ) ;
#21374 = CARTESIAN_POINT ( 'NONE',  ( -19.60912206198628027, -0.1191753592594197858, 4.398475361799976113 ) ) ;
#21375 = ORIENTED_EDGE ( 'NONE', *, *, #6006, .T. ) ;
#21376 = CARTESIAN_POINT ( 'NONE',  ( -24.26986129792355129, -0.1191753592594197858, 6.208864760408702388 ) ) ;
#21377 = DIRECTION ( 'NONE',  ( -0.7660212471507179544, -0.6427876096865405842, -0.005961354470445141482 ) ) ;
#21378 = FACE_OUTER_BOUND ( 'NONE', #32029, .T. ) ;
#21379 = VERTEX_POINT ( 'NONE', #9659 ) ;
#21380 = CYLINDRICAL_SURFACE ( 'NONE', #145, 6.000000000000001776 ) ;
#21381 = CARTESIAN_POINT ( 'NONE',  ( -15.40103151951671734, 0.000000000000000000, 12.95233060667165681 ) ) ;
#21382 = FACE_OUTER_BOUND ( 'NONE', #34244, .T. ) ;
#21383 = FACE_OUTER_BOUND ( 'NONE', #12497, .T. ) ;
#21385 = EDGE_CURVE ( 'NONE', #41167, #50834, #40853, .T. ) ;
#21384 = DIRECTION ( 'NONE',  ( 0.5449076811759707706, 0.6444004775717708799, -0.5364919789714476250 ) ) ;
#21386 = VECTOR ( 'NONE', #43285, 999.9999999999998863 ) ;
#21387 = LINE ( 'NONE', #48316, #3181 ) ;
#21388 = ORIENTED_EDGE ( 'NONE', *, *, #16387, .F. ) ;
#21389 = FACE_OUTER_BOUND ( 'NONE', #6653, .T. ) ;
#21390 = VECTOR ( 'NONE', #48372, 1000.000000000000000 ) ;
#21391 = CARTESIAN_POINT ( 'NONE',  ( -9.908141408373387193, -0.1191753592594197858, 10.77908512878318703 ) ) ;
#21392 = EDGE_CURVE ( 'NONE', #8533, #28185, #53371, .T. ) ;
#21393 = DIRECTION ( 'NONE',  ( 0.007781995580012663651, -3.146120232559066537E-19, -0.9999697198139514409 ) ) ;
#21394 = ORIENTED_EDGE ( 'NONE', *, *, #16405, .F. ) ;
#21395 = DIRECTION ( 'NONE',  ( 0.6427681459581294776, -0.7660444431189769032, 0.005002170337467562802 ) ) ;
#21396 = DIRECTION ( 'NONE',  ( 0.5364919789714477361, 0.6444004775717706579, 0.5449076811759711036 ) ) ;
#21397 = CIRCLE ( 'NONE', #24147, 2.000000000000002220 ) ;
#21398 = ORIENTED_EDGE ( 'NONE', *, *, #24294, .T. ) ;
#21399 = PLANE ( 'NONE',  #6252 ) ;
#21400 = CARTESIAN_POINT ( 'NONE',  ( -13.50569345835905111, 0.000000000000000000, 8.239297380650791425 ) ) ;
#21401 = EDGE_CURVE ( 'NONE', #41663, #41818, #28074, .T. ) ;
#21402 = VECTOR ( 'NONE', #39476, 999.9999999999998863 ) ;
#21403 = CARTESIAN_POINT ( 'NONE',  ( -14.93495759592298988, 0.000000000000000000, 12.77129166681078409 ) ) ;
#21404 = EDGE_CURVE ( 'NONE', #13581, #9203, #27513, .T. ) ;
#21405 = CARTESIAN_POINT ( 'NONE',  ( -67.68741903510353097, 2.000000000018216539, 3.427396607167120912 ) ) ;
#21406 = EDGE_LOOP ( 'NONE', ( #51558, #51716, #18003, #17645 ) ) ;
#21407 = VECTOR ( 'NONE', #54454, 1000.000000000000227 ) ;
#21408 = AXIS2_PLACEMENT_3D ( 'NONE', #1536, #53752, #35915 ) ;
#21409 = VERTEX_POINT ( 'NONE', #53907 ) ;
#21410 = CARTESIAN_POINT ( 'NONE',  ( -67.09379796712988764, -0.6008889714318613740, 1.346828299457901501 ) ) ;
#21411 = CARTESIAN_POINT ( 'NONE',  ( -14.52268981044348450, -0.1191753592594179401, 6.654051572544311455 ) ) ;
#21412 = CARTESIAN_POINT ( 'NONE',  ( -13.02225584137026893, 0.000000000000000000, 5.827061128909424070 ) ) ;
#21413 = VECTOR ( 'NONE', #53015, 999.9999999999998863 ) ;
#21414 = VECTOR ( 'NONE', #587, 999.9999999999998863 ) ;
#21415 = PLANE ( 'NONE',  #26615 ) ;
#21417 = CARTESIAN_POINT ( 'NONE',  ( -17.23519096270132422, -1.165603555308157846, 3.538865740624604683 ) ) ;
#21416 = VECTOR ( 'NONE', #35205, 1000.000000000000227 ) ;
#21418 = FACE_OUTER_BOUND ( 'NONE', #55014, .T. ) ;
#21419 = ORIENTED_EDGE ( 'NONE', *, *, #52302, .F. ) ;
#21420 = LINE ( 'NONE', #25656, #3871 ) ;
#21421 = AXIS2_PLACEMENT_3D ( 'NONE', #27863, #15070, #10237 ) ;
#21422 = VECTOR ( 'NONE', #53998, 1000.000000000000227 ) ;
#21423 = LINE ( 'NONE', #25660, #51432 ) ;
#21424 = ORIENTED_EDGE ( 'NONE', *, *, #5349, .F. ) ;
#21425 = LINE ( 'NONE', #4644, #54663 ) ;
#21426 = LINE ( 'NONE', #17155, #41317 ) ;
#21427 = DIRECTION ( 'NONE',  ( -0.7660212471507179544, -0.6427876096865405842, -0.005961354470445141482 ) ) ;
#21428 = ORIENTED_EDGE ( 'NONE', *, *, #39039, .F. ) ;
#21429 = DIRECTION ( 'NONE',  ( 0.000000000000000000, -1.000000000000000000, 0.000000000000000000 ) ) ;
#21430 = ORIENTED_EDGE ( 'NONE', *, *, #35440, .T. ) ;
#21431 = VECTOR ( 'NONE', #6667, 999.9999999999998863 ) ;
#21432 = EDGE_LOOP ( 'NONE', ( #7752, #12288, #12806, #41473 ) ) ;
#21433 = B_SPLINE_CURVE_WITH_KNOTS ( 'NONE', 3,
 ( #2397, #45831, #50913, #16868, #12015, #51213, #4078, #3778, #34199, #42974, #37594, #20567, #12328, #21410, #3234, #46370, #37888, #25956, #8326, #12603, #3515, #55192, #55755, #38142, #54920, #51510, #29921, #46965 ),
 .UNSPECIFIED., .F., .F.,
 ( 4, 2, 2, 2, 2, 2, 2, 2, 2, 2, 2, 2, 2, 4 ),
 ( 7.806255641895631925E-18, 0.002014507434814110081, 0.004029014869628212356, 0.006043522304442314197, 0.007050776021849361648, 0.008058029739256410834, 0.009065283456663457418, 0.01007253717407050400, 0.01208704460888460064, 0.01309429832629165416, 0.01410155204369870768, 0.01510880576110576468, 0.01561243261980930011, 0.01611605947851283901 ),
 .UNSPECIFIED. ) ;
#21434 = ORIENTED_EDGE ( 'NONE', *, *, #37764, .F. ) ;
#21435 = ORIENTED_EDGE ( 'NONE', *, *, #40211, .T. ) ;
#21436 = PLANE ( 'NONE',  #52954 ) ;
#21437 = AXIS2_PLACEMENT_3D ( 'NONE', #55240, #38192, #16619 ) ;
#21438 = VERTEX_POINT ( 'NONE', #18735 ) ;
#21439 = DIRECTION ( 'NONE',  ( 0.6427681459581294776, -0.7660444431189769032, 0.005002170337467562802 ) ) ;
#21440 = EDGE_CURVE ( 'NONE', #5343, #47558, #45379, .T. ) ;
#21441 = ORIENTED_EDGE ( 'NONE', *, *, #27498, .F. ) ;
#21442 = LINE ( 'NONE', #7516, #15023 ) ;
#21443 = AXIS2_PLACEMENT_3D ( 'NONE', #47367, #7636, #15873 ) ;
#21444 = ORIENTED_EDGE ( 'NONE', *, *, #39773, .F. ) ;
#21445 = LINE ( 'NONE', #35077, #11967 ) ;
#21446 = ORIENTED_EDGE ( 'NONE', *, *, #11451, .T. ) ;
#21447 = EDGE_CURVE ( 'NONE', #49405, #23911, #7320, .T. ) ;
#21448 = ADVANCED_FACE ( 'NONE', ( #20386 ), #6494, .F. ) ;
#21449 = AXIS2_PLACEMENT_3D ( 'NONE', #33954, #20629, #7856 ) ;
#21450 = DIRECTION ( 'NONE',  ( -0.5449076811759708816, 0.6444004775717707689, 0.5364919789714475140 ) ) ;
#21451 = DIRECTION ( 'NONE',  ( 0.000000000000000000, -1.000000000000000000, 0.000000000000000000 ) ) ;
#21452 = PLANE ( 'NONE',  #49450 ) ;
#21453 = LINE ( 'NONE', #38468, #35990 ) ;
#21454 = PLANE ( 'NONE',  #17433 ) ;
#21455 = ORIENTED_EDGE ( 'NONE', *, *, #12671, .F. ) ;
#21456 = VECTOR ( 'NONE', #20609, 1000.000000000000114 ) ;
#21457 = EDGE_LOOP ( 'NONE', ( #53700, #29628, #38588, #30122 ) ) ;
#21458 = AXIS2_PLACEMENT_3D ( 'NONE', #7454, #17893, #54885 ) ;
#21459 = DIRECTION ( 'NONE',  ( 0.5364919789714477361, 0.6444004775717706579, 0.5449076811759711036 ) ) ;
#21460 = DIRECTION ( 'NONE',  ( -0.005961354470445682716, -0.6427876096865404731, 0.7660212471507180654 ) ) ;
#21461 = VECTOR ( 'NONE', #20355, 1000.000000000000000 ) ;
#21462 = DIRECTION ( 'NONE',  ( 0.6427681459581294776, -0.7660444431189769032, 0.005002170337467562802 ) ) ;
#21463 = AXIS2_PLACEMENT_3D ( 'NONE', #40475, #18598, #6379 ) ;
#21464 = DIRECTION ( 'NONE',  ( 0.007781995580012663651, 0.000000000000000000, -0.9999697198139515519 ) ) ;
#21465 = DIRECTION ( 'NONE',  ( 0.007781995580012662783, 0.000000000000000000, -0.9999697198139514409 ) ) ;
#21466 = DIRECTION ( 'NONE',  ( 0.000000000000000000, -1.000000000000000000, 0.000000000000000000 ) ) ;
#21467 = ORIENTED_EDGE ( 'NONE', *, *, #1503, .T. ) ;
#21468 = DIRECTION ( 'NONE',  ( -0.005961354470445682716, -0.6427876096865404731, 0.7660212471507180654 ) ) ;
#21469 = DIRECTION ( 'NONE',  ( 0.005002170337468016433, -0.7660444431189770143, -0.6427681459581293666 ) ) ;
#21470 = VERTEX_POINT ( 'NONE', #49914 ) ;
#21471 = DIRECTION ( 'NONE',  ( 0.9999697198139515519, 0.000000000000000000, 0.007781995580013368816 ) ) ;
#21472 = CARTESIAN_POINT ( 'NONE',  ( -18.70476884740427437, -5.051250379848162275, 12.23746159482404217 ) ) ;
#21473 = CARTESIAN_POINT ( 'NONE',  ( -18.66354898467281132, 0.000000000000000000, 14.21960318569776582 ) ) ;
#21474 = EDGE_CURVE ( 'NONE', #14373, #33629, #7608, .T. ) ;
#21475 = FACE_OUTER_BOUND ( 'NONE', #33094, .T. ) ;
#21476 = AXIS2_PLACEMENT_3D ( 'NONE', #8287, #55419, #21057 ) ;
#21477 = VERTEX_POINT ( 'NONE', #54450 ) ;
#21478 = EDGE_CURVE ( 'NONE', #1875, #43669, #20201, .T. ) ;
#21479 = VERTEX_POINT ( 'NONE', #37727 ) ;
#21480 = DIRECTION ( 'NONE',  ( 0.005961354470445682716, -0.6427876096865404731, -0.7660212471507180654 ) ) ;
#21481 = LINE ( 'NONE', #22591, #35867 ) ;
#21482 = LINE ( 'NONE', #39345, #55081 ) ;
#21483 = CARTESIAN_POINT ( 'NONE',  ( -27.99767448711536133, 0.000000000000000000, 7.557179307314289218 ) ) ;
#21484 = AXIS2_PLACEMENT_3D ( 'NONE', #37682, #29435, #16099 ) ;
#21485 = ADVANCED_FACE ( 'NONE', ( #42259 ), #46213, .F. ) ;
#21486 = LINE ( 'NONE', #7870, #48441 ) ;
#21487 = DIRECTION ( 'NONE',  ( 0.6246952433987894571, -0.7422098413412800966, -0.2426528472758541777 ) ) ;
#21488 = DIRECTION ( 'NONE',  ( 0.007781995580012663651, -3.146120232559066537E-19, -0.9999697198139514409 ) ) ;
#21489 = ORIENTED_EDGE ( 'NONE', *, *, #11801, .T. ) ;
#21491 = VECTOR ( 'NONE', #2916, 1000.000000000000227 ) ;
#21490 = LINE ( 'NONE', #54224, #28681 ) ;
#21492 = LINE ( 'NONE', #17208, #36017 ) ;
#21493 = ORIENTED_EDGE ( 'NONE', *, *, #11740, .T. ) ;
#21494 = CARTESIAN_POINT ( 'NONE',  ( -16.81267852042391198, -0.1191753592594197858, 3.312241722634738039 ) ) ;
#21495 = ORIENTED_EDGE ( 'NONE', *, *, #19735, .F. ) ;
#21496 = CARTESIAN_POINT ( 'NONE',  ( -11.40636015113596180, 0.000000000000000000, 11.32142374880780089 ) ) ;
#21497 = ORIENTED_EDGE ( 'NONE', *, *, #50659, .F. ) ;
#21498 = VECTOR ( 'NONE', #51029, 1000.000000000000227 ) ;
#21499 = EDGE_LOOP ( 'NONE', ( #42867, #54172, #27406, #45220 ) ) ;
#21500 = ADVANCED_FACE ( 'NONE', ( #33720 ), #15846, .F. ) ;
#21501 = ORIENTED_EDGE ( 'NONE', *, *, #41555, .F. ) ;
#21502 = AXIS2_PLACEMENT_3D ( 'NONE', #1752, #27907, #49747 ) ;
#21503 = ORIENTED_EDGE ( 'NONE', *, *, #7256, .T. ) ;
#21504 = VERTEX_POINT ( 'NONE', #2763 ) ;
#21505 = ORIENTED_EDGE ( 'NONE', *, *, #53064, .T. ) ;
#21506 = DIRECTION ( 'NONE',  ( 0.5449076811759707706, 0.6444004775717708799, -0.5364919789714476250 ) ) ;
#21507 = CARTESIAN_POINT ( 'NONE',  ( -21.50121238896663911, -5.051250379848161387, 13.32369523398927846 ) ) ;
#21508 = EDGE_CURVE ( 'NONE', #41488, #28129, #41132, .T. ) ;
#21509 = CARTESIAN_POINT ( 'NONE',  ( -16.81345671998191449, 0.000000000000000000, 3.412238694616132495 ) ) ;
#21511 = ADVANCED_FACE ( 'NONE', ( #33456 ), #19557, .F. ) ;
#21510 = VERTEX_POINT ( 'NONE', #28340 ) ;
#21512 = FACE_OUTER_BOUND ( 'NONE', #19744, .T. ) ;
#21513 = ORIENTED_EDGE ( 'NONE', *, *, #42117, .F. ) ;
#21514 = CARTESIAN_POINT ( 'NONE',  ( -17.74404816805336793, 0.000000000000000000, 3.574322630375089460 ) ) ;
#21515 = ORIENTED_EDGE ( 'NONE', *, *, #32132, .F. ) ;
#21516 = ADVANCED_FACE ( 'NONE', ( #3056 ), #24635, .F. ) ;
#21517 = EDGE_CURVE ( 'NONE', #15338, #30167, #24939, .T. ) ;
#21518 = CARTESIAN_POINT ( 'NONE',  ( 2.072287782118878319, 0.000000000000000000, -2.950529333540147015 ) ) ;
#21519 = CARTESIAN_POINT ( 'NONE',  ( -67.81626209598535127, 0.000000000000000000, 7.454917401049828918 ) ) ;
#21520 = CARTESIAN_POINT ( 'NONE',  ( -15.90223023344033315, -0.1191753592594212430, 4.796655320951466628 ) ) ;
#21521 = ORIENTED_EDGE ( 'NONE', *, *, #42925, .F. ) ;
#21522 = DIRECTION ( 'NONE',  ( 0.5364919789714477361, 0.6444004775717706579, 0.5449076811759711036 ) ) ;
#21523 = ORIENTED_EDGE ( 'NONE', *, *, #25878, .T. ) ;
#21524 = CARTESIAN_POINT ( 'NONE',  ( -13.53673582514181106, 0.000000000000000000, 12.22817484722816772 ) ) ;
#21525 = VECTOR ( 'NONE', #5767, 1000.000000000000227 ) ;
#21526 = PLANE ( 'NONE',  #49316 ) ;
#21527 = EDGE_CURVE ( 'NONE', #33755, #2289, #38001, .T. ) ;
#21528 = CARTESIAN_POINT ( 'NONE',  ( -21.22173678941378228, -4.241740624735664156, 4.989230645525445595 ) ) ;
#21529 = AXIS2_PLACEMENT_3D ( 'NONE', #7866, #12089, #37674 ) ;
#21530 = DIRECTION ( 'NONE',  ( 0.8531650599175527594, 0.4028455766673922356, -0.3313982828793700652 ) ) ;
#21531 = CARTESIAN_POINT ( 'NONE',  ( -24.26908309836554878, 0.000000000000000000, 6.108867788427308376 ) ) ;
#21532 = LINE ( 'NONE', #29176, #2206 ) ;
#21533 = DIRECTION ( 'NONE',  ( 0.3535533905932738974, -0.6123724356957929160, -0.7071067811865487940 ) ) ;
#21534 = CARTESIAN_POINT ( 'NONE',  ( -11.23781311569048924, 0.4483081953215033444, 1.032776604783083307 ) ) ;
#21535 = EDGE_LOOP ( 'NONE', ( #8702, #21628, #51665, #41525 ) ) ;
#21536 = PLANE ( 'NONE',  #15661 ) ;
#21537 = ORIENTED_EDGE ( 'NONE', *, *, #55936, .T. ) ;
#21538 = VECTOR ( 'NONE', #40459, 1000.000000000000227 ) ;
#21539 = DIRECTION ( 'NONE',  ( 0.000000000000000000, -0.000000000000000000, -1.000000000000000000 ) ) ;
#21540 = LINE ( 'NONE', #53024, #28693 ) ;
#21541 = DIRECTION ( 'NONE',  ( 0.000000000000000000, -1.000000000000000000, 0.000000000000000000 ) ) ;
#21542 = DIRECTION ( 'NONE',  ( -0.9999697198139514409, -0.000000000000000000, -0.007781995580013368816 ) ) ;
#21543 = FACE_OUTER_BOUND ( 'NONE', #801, .T. ) ;
#21544 = CARTESIAN_POINT ( 'NONE',  ( -27.06552663992790997, 0.000000000000000000, 7.195101427592543786 ) ) ;
#21545 = B_SPLINE_CURVE_WITH_KNOTS ( 'NONE', 3,
 ( #30041, #51349, #50768, #4222 ),
 .UNSPECIFIED., .F., .F.,
 ( 4, 4 ),
 ( 0.000000000000000000, 0.0003538173816226116894 ),
 .UNSPECIFIED. ) ;
#21546 = LINE ( 'NONE', #29787, #32065 ) ;
#21547 = APPLICATION_PROTOCOL_DEFINITION ( 'draft international standard', 'automotive_design', 1998, #13390 ) ;
#21548 = ORIENTED_EDGE ( 'NONE', *, *, #29532, .T. ) ;
#21549 = CARTESIAN_POINT ( 'NONE',  ( -11.87243407472968926, 0.000000000000000000, 11.50246268866867361 ) ) ;
#21550 = CARTESIAN_POINT ( 'NONE',  ( -11.77243710274829525, -0.1191753592594197858, 11.50324088822667612 ) ) ;
#21551 = CARTESIAN_POINT ( 'NONE',  ( -15.22435894240294552, 3.524445264749009876, 2.483141509683923775 ) ) ;
#21552 = LINE ( 'NONE', #22398, #38172 ) ;
#21553 = ADVANCED_FACE ( 'NONE', ( #15300 ), #24099, .F. ) ;
#21554 = CARTESIAN_POINT ( 'NONE',  ( -18.67619601524082285, 0.000000000000000000, 3.936400510096834893 ) ) ;
#21555 = CARTESIAN_POINT ( 'NONE',  ( -16.28776673239499928, 0.000000000000000000, 7.478982503527205061 ) ) ;
#21556 = CARTESIAN_POINT ( 'NONE',  ( -17.99589520542714638, 1.257817950434005461, 5.935831502157483897 ) ) ;
#21557 = ORIENTED_EDGE ( 'NONE', *, *, #24391, .F. ) ;
#21558 = LINE ( 'NONE', #38873, #8562 ) ;
#21559 = CARTESIAN_POINT ( 'NONE',  ( -67.07240009714290352, -9.519890509981273397, -2.692672496485625455 ) ) ;
#21560 = ORIENTED_EDGE ( 'NONE', *, *, #3618, .F. ) ;
#21561 = ORIENTED_EDGE ( 'NONE', *, *, #29786, .F. ) ;
#21562 = CARTESIAN_POINT ( 'NONE',  ( -9.974221960066742554, 0.000000000000000000, 6.420119759390041203 ) ) ;
#21563 = ADVANCED_FACE ( 'NONE', ( #51036 ), #32610, .F. ) ;
#21564 = ORIENTED_EDGE ( 'NONE', *, *, #1732, .T. ) ;
#21565 = ADVANCED_FACE ( 'NONE', ( #41427 ), #2512, .F. ) ;
#21566 = EDGE_CURVE ( 'NONE', #42380, #35539, #7072, .T. ) ;
#21567 = AXIS2_PLACEMENT_3D ( 'NONE', #14152, #36280, #54160 ) ;
#21568 = ORIENTED_EDGE ( 'NONE', *, *, #31203, .F. ) ;
#21569 = ORIENTED_EDGE ( 'NONE', *, *, #53310, .T. ) ;
#21570 = ORIENTED_EDGE ( 'NONE', *, *, #15087, .T. ) ;
#21571 = DIRECTION ( 'NONE',  ( 0.005002170337468016433, -0.7660444431189770143, -0.6427681459581293666 ) ) ;
#21572 = ORIENTED_EDGE ( 'NONE', *, *, #13722, .T. ) ;
#21573 = CARTESIAN_POINT ( 'NONE',  ( -13.53673582514181106, 0.000000000000000000, 12.22817484722816772 ) ) ;
#21574 = EDGE_CURVE ( 'NONE', #55289, #6087, #20934, .T. ) ;
#21575 = PLANE ( 'NONE',  #55724 ) ;
#21576 = CIRCLE ( 'NONE', #41507, 1.000000000000000444 ) ;
#21577 = EDGE_CURVE ( 'NONE', #50902, #1435, #56161, .T. ) ;
#21578 = ORIENTED_EDGE ( 'NONE', *, *, #25281, .T. ) ;
#21579 = EDGE_LOOP ( 'NONE', ( #14439, #1851, #5619, #16692 ) ) ;
#21580 = EDGE_CURVE ( 'NONE', #38002, #50681, #17835, .T. ) ;
#21581 = DIRECTION ( 'NONE',  ( 0.007781995580012663651, -3.146120232559066537E-19, -0.9999697198139514409 ) ) ;
#21582 = ORIENTED_EDGE ( 'NONE', *, *, #23918, .T. ) ;
#21583 = LINE ( 'NONE', #25832, #31877 ) ;
#21584 = CARTESIAN_POINT ( 'NONE',  ( 5.558065690504402134, 8.867811663421879681E-06, -2.260478214935544017 ) ) ;
#21585 = ORIENTED_EDGE ( 'NONE', *, *, #15381, .F. ) ;
#21586 = CARTESIAN_POINT ( 'NONE',  ( -19.27721902470766935, 3.848249166794008413, 10.68488013071350551 ) ) ;
#21587 = EDGE_CURVE ( 'NONE', #22163, #19674, #17245, .T. ) ;
#21588 = VERTEX_POINT ( 'NONE', #34566 ) ;
#21589 = CARTESIAN_POINT ( 'NONE',  ( 2.072287782118878319, 0.000000000000000000, -2.950529333540147015 ) ) ;
#21590 = EDGE_CURVE ( 'NONE', #37607, #12378, #43641, .T. ) ;
#21591 = DIRECTION ( 'NONE',  ( -0.9999697198139514409, -0.000000000000000000, -0.007781995580013368816 ) ) ;
#21592 = EDGE_LOOP ( 'NONE', ( #17482, #52223, #17934, #8348 ) ) ;
#21593 = CARTESIAN_POINT ( 'NONE',  ( -16.28046222626843331, 0.000000000000000000, 6.540369153048884776 ) ) ;
#21594 = DIRECTION ( 'NONE',  ( -0.005961354470445682716, -0.6427876096865404731, 0.7660212471507180654 ) ) ;
#21595 = DIRECTION ( 'NONE',  ( 0.000000000000000000, -1.000000000000000000, 0.000000000000000000 ) ) ;
#21596 = LINE ( 'NONE', #22138, #40121 ) ;
#21597 = ORIENTED_EDGE ( 'NONE', *, *, #2237, .F. ) ;
#21598 = CARTESIAN_POINT ( 'NONE',  ( -10.47421230394850866, 0.000000000000000000, 10.95934586908605723 ) ) ;
#21599 = DIRECTION ( 'NONE',  ( 0.2426528472758541499, 0.7422098413412800966, 0.6246952433987894571 ) ) ;
#21600 = CARTESIAN_POINT ( 'NONE',  ( -20.83174675134727138, 0.7721120973665036580, 4.749055200455086556 ) ) ;
#21601 = DIRECTION ( 'NONE',  ( 0.5364919789714477361, 0.6444004775717706579, 0.5449076811759711036 ) ) ;
#21602 = CARTESIAN_POINT ( 'NONE',  ( -20.26176469941677993, 0.000000000000000000, 14.76116360616437895 ) ) ;
#21603 = DIRECTION ( 'NONE',  ( -0.7660212471507179544, -0.6427876096865405842, -0.005961354470445141482 ) ) ;
#21604 = FACE_OUTER_BOUND ( 'NONE', #474, .T. ) ;
#21605 = DIRECTION ( 'NONE',  ( -0.005002170337468016433, -0.7660444431189770143, 0.6427681459581293666 ) ) ;
#21606 = DIRECTION ( 'NONE',  ( 0.007781995580012663651, 0.000000000000000000, -0.9999697198139515519 ) ) ;
#21607 = VERTEX_POINT ( 'NONE', #35166 ) ;
#21608 = PRESENTATION_STYLE_ASSIGNMENT (( #51958 ) ) ;
#21609 = DIRECTION ( 'NONE',  ( 0.007781995580012663651, -3.146120232559066537E-19, -0.9999697198139514409 ) ) ;
#21610 = ORIENTED_EDGE ( 'NONE', *, *, #4327, .T. ) ;
#21611 = PLANE ( 'NONE',  #12980 ) ;
#21612 = CARTESIAN_POINT ( 'NONE',  ( 5.221828392167458865, 0.000000000000000000, 2.393421119419573806 ) ) ;
#21613 = VECTOR ( 'NONE', #36077, 1000.000000000000227 ) ;
#21614 = CARTESIAN_POINT ( 'NONE',  ( -13.56754953521377161, -0.1191753592594196748, 3.337496066760455182 ) ) ;
#21615 = ADVANCED_FACE ( 'NONE', ( #26328 ), #16693, .F. ) ;
#21616 = LINE ( 'NONE', #55976, #38735 ) ;
#21617 = LINE ( 'NONE', #3704, #51043 ) ;
#21618 = ORIENTED_EDGE ( 'NONE', *, *, #8487, .T. ) ;
#21619 = VERTEX_POINT ( 'NONE', #51615 ) ;
#21620 = CARTESIAN_POINT ( 'NONE',  ( -56.20083583094844926, 4.876814673940706335, 2.999999999999993339 ) ) ;
#21621 = PLANE ( 'NONE',  #28593 ) ;
#21622 = VERTEX_POINT ( 'NONE', #22075 ) ;
#21623 = EDGE_CURVE ( 'NONE', #16632, #7363, #8763, .T. ) ;
#21624 = EDGE_CURVE ( 'NONE', #2289, #17587, #38850, .T. ) ;
#21625 = DIRECTION ( 'NONE',  ( 0.000000000000000000, -0.000000000000000000, -1.000000000000000000 ) ) ;
#21626 = ORIENTED_EDGE ( 'NONE', *, *, #51527, .F. ) ;
#21627 = DIRECTION ( 'NONE',  ( 0.5449076811759707706, 0.6444004775717708799, -0.5364919789714476250 ) ) ;
#21628 = ORIENTED_EDGE ( 'NONE', *, *, #16760, .F. ) ;
#21629 = CARTESIAN_POINT ( 'NONE',  ( -17.75502971379410511, -0.1191753592594194250, 4.043572267363897410 ) ) ;
#21630 = EDGE_CURVE ( 'NONE', #26641, #32939, #39407, .T. ) ;
#21631 = VERTEX_POINT ( 'NONE', #47344 ) ;
#21632 = ORIENTED_EDGE ( 'NONE', *, *, #8064, .T. ) ;
#21633 = ORIENTED_EDGE ( 'NONE', *, *, #30945, .F. ) ;
#21634 = CARTESIAN_POINT ( 'NONE',  ( -1.905187828007888884, 6.291258001618519557, 3.958413228513044668 ) ) ;
#21635 = DIRECTION ( 'NONE',  ( 0.000000000000000000, -1.000000000000000000, 0.000000000000000000 ) ) ;
#21636 = DIRECTION ( 'NONE',  ( 0.005961354470445682716, -0.6427876096865404731, -0.7660212471507180654 ) ) ;
#21637 = LINE ( 'NONE', #26175, #11240 ) ;
#21638 = ADVANCED_FACE ( 'NONE', ( #51882 ), #13560, .F. ) ;
#21639 = EDGE_LOOP ( 'NONE', ( #32957, #46907, #43980, #29992 ) ) ;
#21640 = ORIENTED_EDGE ( 'NONE', *, *, #2682, .T. ) ;
#21641 = EDGE_CURVE ( 'NONE', #40359, #30303, #40783, .T. ) ;
#21642 = VERTEX_POINT ( 'NONE', #3902 ) ;
#21643 = CARTESIAN_POINT ( 'NONE',  ( -17.34997331854206237, -0.1941918491731542684, 3.614444224982700682 ) ) ;
#21644 = EDGE_CURVE ( 'NONE', #55726, #55546, #188, .T. ) ;
#21645 = VERTEX_POINT ( 'NONE', #25778 ) ;
#21646 = DIRECTION ( 'NONE',  ( 0.000000000000000000, -1.000000000000000000, 0.000000000000000000 ) ) ;
#21647 = ORIENTED_EDGE ( 'NONE', *, *, #34493, .T. ) ;
#21648 = CARTESIAN_POINT ( 'NONE',  ( -69.66297551618575312, -8.676591480033549075, 7.503902134509970345 ) ) ;
#21649 = LINE ( 'NONE', #43491, #2231 ) ;
#21650 = ADVANCED_FACE ( 'NONE', ( #4218 ), #21536, .F. ) ;
#21651 = AXIS2_PLACEMENT_3D ( 'NONE', #9148, #38413, #26462 ) ;
#21652 = VERTEX_POINT ( 'NONE', #1874 ) ;
#21653 = LINE ( 'NONE', #38697, #27735 ) ;
#21654 = EDGE_LOOP ( 'NONE', ( #21493, #33086, #20028, #2265 ) ) ;
#21655 = LINE ( 'NONE', #26191, #54467 ) ;
#21656 = ORIENTED_EDGE ( 'NONE', *, *, #17398, .F. ) ;
#21657 = CARTESIAN_POINT ( 'NONE',  ( -17.19692215154019621, 0.000000000000000000, 4.886582757186834769 ) ) ;
#21658 = DIRECTION ( 'NONE',  ( -0.5364919789714478471, 0.6444004775717705469, -0.5449076811759709926 ) ) ;
#21659 = FACE_OUTER_BOUND ( 'NONE', #5548, .T. ) ;
#21660 = ORIENTED_EDGE ( 'NONE', *, *, #25254, .T. ) ;
#21661 = CARTESIAN_POINT ( 'NONE',  ( -23.33849165029409889, 0.000000000000000000, 5.946783852668351855 ) ) ;
#21662 = FACE_OUTER_BOUND ( 'NONE', #21192, .T. ) ;
#21663 = DIRECTION ( 'NONE',  ( 0.7660212471507180654, -0.6427876096865404731, 0.005961354470445141482 ) ) ;
#21664 = DIRECTION ( 'NONE',  ( -0.9999697198139514409, -0.000000000000000000, -0.007781995580013368816 ) ) ;
#21665 = CARTESIAN_POINT ( 'NONE',  ( -13.50974395553640761, 2.553033558614007603, 6.318927477965895712 ) ) ;
#21666 = CARTESIAN_POINT ( 'NONE',  ( -15.40103151951671734, 0.000000000000000000, 12.95233060667165681 ) ) ;
#21667 = PLANE ( 'NONE',  #24027 ) ;
#21668 = ORIENTED_EDGE ( 'NONE', *, *, #28923, .F. ) ;
#21669 = CARTESIAN_POINT ( 'NONE',  ( -15.83750010308032685, 0.000000000000000000, 9.329146931584036295 ) ) ;
#21670 = DIRECTION ( 'NONE',  ( 0.2113248654051873565, 0.7886751345948123104, 0.5773502691896265082 ) ) ;
#21671 = LINE ( 'NONE', #38984, #54104 ) ;
#21672 = ORIENTED_EDGE ( 'NONE', *, *, #36461, .T. ) ;
#21673 = LINE ( 'NONE', #9437, #38383 ) ;
#21674 = LINE ( 'NONE', #12862, #47662 ) ;
#21675 = ORIENTED_EDGE ( 'NONE', *, *, #22066, .T. ) ;
#21676 = EDGE_CURVE ( 'NONE', #26864, #4402, #775, .T. ) ;
#21677 = DIRECTION ( 'NONE',  ( 0.007781995580012663651, 0.000000000000000000, -0.9999697198139515519 ) ) ;
#21678 = FACE_OUTER_BOUND ( 'NONE', #24680, .T. ) ;
#21679 = ADVANCED_FACE ( 'NONE', ( #23215 ), #27449, .F. ) ;
#21680 = CARTESIAN_POINT ( 'NONE',  ( -11.17388681363777181, 0.000000000000000000, 7.149447829717543890 ) ) ;
#21681 = CARTESIAN_POINT ( 'NONE',  ( -67.26848159797359017, 2.000000000007965184, -1.381457631268952602 ) ) ;
#21682 = ORIENTED_EDGE ( 'NONE', *, *, #54678, .F. ) ;
#21683 = ORIENTED_EDGE ( 'NONE', *, *, #41885, .F. ) ;
#21684 = ADVANCED_FACE ( 'NONE', ( #31462 ), #5589, .F. ) ;
#21685 = LINE ( 'NONE', #13992, #22177 ) ;
#21686 = PLANE ( 'NONE',  #1382 ) ;
#21687 = DIRECTION ( 'NONE',  ( 0.6427681459581294776, -0.7660444431189769032, 0.005002170337467562802 ) ) ;
#21688 = EDGE_CURVE ( 'NONE', #45145, #27973, #36529, .T. ) ;
#21689 = ADVANCED_FACE ( 'NONE', ( #39951 ), #26917, .F. ) ;
#21690 = ADVANCED_FACE ( 'NONE', ( #9874 ), #13827, .F. ) ;
#21691 = DIRECTION ( 'NONE',  ( 0.005002170337468016433, -0.7660444431189770143, -0.6427681459581293666 ) ) ;
#21692 = DIRECTION ( 'NONE',  ( 0.5364919789714477361, 0.6444004775717706579, 0.5449076811759711036 ) ) ;
#21693 = CARTESIAN_POINT ( 'NONE',  ( 2.072287782118878319, 0.000000000000000000, -2.950529333540147015 ) ) ;
#21695 = EDGE_CURVE ( 'NONE', #28180, #40645, #27176, .T. ) ;
#21694 = ORIENTED_EDGE ( 'NONE', *, *, #32776, .F. ) ;
#21696 = CARTESIAN_POINT ( 'NONE',  ( -11.87243407472968926, 0.000000000000000000, 11.50246268866867361 ) ) ;
#21697 = LINE ( 'NONE', #35055, #34219 ) ;
#21698 = ORIENTED_EDGE ( 'NONE', *, *, #26350, .T. ) ;
#21699 = CARTESIAN_POINT ( 'NONE',  ( -27.06552663992790997, 0.000000000000000000, 7.195101427592543786 ) ) ;
#21700 = LINE ( 'NONE', #373, #35949 ) ;
#21701 = DIRECTION ( 'NONE',  ( 0.000000000000000000, 1.000000000000000000, 0.000000000000000000 ) ) ;
#21702 = ORIENTED_EDGE ( 'NONE', *, *, #40617, .F. ) ;
#21703 = CARTESIAN_POINT ( 'NONE',  ( -18.86354292863559579, 0.000000000000000000, 14.21804678658176080 ) ) ;
#21704 = ORIENTED_EDGE ( 'NONE', *, *, #50385, .T. ) ;
#21706 = EDGE_LOOP ( 'NONE', ( #12912, #11255, #3955, #25594 ) ) ;
#21705 = EDGE_CURVE ( 'NONE', #3673, #44974, #10130, .T. ) ;
#21707 = VERTEX_POINT ( 'NONE', #19196 ) ;
#21708 = EDGE_CURVE ( 'NONE', #32088, #42922, #23484, .T. ) ;
#21709 = ORIENTED_EDGE ( 'NONE', *, *, #32964, .T. ) ;
#21710 = PLANE ( 'NONE',  #39341 ) ;
#21711 = EDGE_LOOP ( 'NONE', ( #46069, #48969, #9190, #40226 ) ) ;
#21712 = CARTESIAN_POINT ( 'NONE',  ( -14.32726051673741452, 22.65437732222383360, -3.841877719209101372 ) ) ;
#21713 = EDGE_CURVE ( 'NONE', #27123, #2, #36268, .T. ) ;
#21714 = ORIENTED_EDGE ( 'NONE', *, *, #44121, .F. ) ;
#21715 = LINE ( 'NONE', #51538, #23182 ) ;
#21716 = VERTEX_POINT ( 'NONE', #26609 ) ;
#21717 = DIRECTION ( 'NONE',  ( 0.5364919789714477361, 0.6444004775717706579, 0.5449076811759711036 ) ) ;
#21718 = VERTEX_POINT ( 'NONE', #53567 ) ;
#21719 = EDGE_CURVE ( 'NONE', #42734, #21652, #5053, .T. ) ;
#21720 = DIRECTION ( 'NONE',  ( 0.6246952433987893460, 0.7422098413412802076, -0.2426528472758539279 ) ) ;
#21721 = CARTESIAN_POINT ( 'NONE',  ( -9.844706253474519997, -0.1191753592594185784, 2.627803954389000829 ) ) ;
#21722 = LINE ( 'NONE', #47554, #46726 ) ;
#21723 = DIRECTION ( 'NONE',  ( -0.5364919789714478471, 0.6444004775717705469, -0.5449076811759709926 ) ) ;
#21724 = FACE_OUTER_BOUND ( 'NONE', #54839, .T. ) ;
#21725 = ORIENTED_EDGE ( 'NONE', *, *, #289, .T. ) ;
#21726 = PRODUCT_DEFINITION_FORMATION_WITH_SPECIFIED_SOURCE ( 'ANY', '', #4656, .NOT_KNOWN. ) ;
#21727 = ORIENTED_EDGE ( 'NONE', *, *, #33743, .T. ) ;
#21728 = DIRECTION ( 'NONE',  ( -0.3313982828793700652, 0.4028455766673916250, -0.8531650599175529814 ) ) ;
#21729 = DIRECTION ( 'NONE',  ( 0.7660212471507180654, -0.6427876096865404731, 0.005961354470445141482 ) ) ;
#21730 = CARTESIAN_POINT ( 'NONE',  ( -19.66652065306912789, -1.813211359398156919, 7.296864978363813314 ) ) ;
#21731 = CARTESIAN_POINT ( 'NONE',  ( -10.94028622754223967, 0.000000000000000000, 11.14038480894692995 ) ) ;
#21732 = CARTESIAN_POINT ( 'NONE',  ( -17.93139508144814442, 0.000000000000000000, 13.85596890686001537 ) ) ;
#21733 = PLANE ( 'NONE',  #35029 ) ;
#21734 = ORIENTED_EDGE ( 'NONE', *, *, #2169, .T. ) ;
#21735 = CARTESIAN_POINT ( 'NONE',  ( -19.60834386242827776, 0.000000000000000000, 4.298478389818581213 ) ) ;
#21736 = CARTESIAN_POINT ( 'NONE',  ( -14.90535225589287549, 0.000000000000000000, 8.967069051862290863 ) ) ;
#21737 = VERTEX_POINT ( 'NONE', #31727 ) ;
#21738 = LINE ( 'NONE', #33953, #5283 ) ;
#21739 = DIRECTION ( 'NONE',  ( 0.5449076811759707706, 0.6444004775717708799, -0.5364919789714476250 ) ) ;
#21740 = CYLINDRICAL_SURFACE ( 'NONE', #15965, 2.750000000000001776 ) ;
#21741 = LINE ( 'NONE', #4433, #29570 ) ;
#21742 = CARTESIAN_POINT ( 'NONE',  ( -14.93495759592298988, 0.000000000000000000, 12.77129166681078409 ) ) ;
#21743 = VERTEX_POINT ( 'NONE', #44774 ) ;
#21744 = ORIENTED_EDGE ( 'NONE', *, *, #23803, .T. ) ;
#21745 = CARTESIAN_POINT ( 'NONE',  ( 2.072287782118878319, 0.000000000000000000, -2.950529333540147015 ) ) ;
#21746 = FACE_OUTER_BOUND ( 'NONE', #2029, .T. ) ;
#21747 = CARTESIAN_POINT ( 'NONE',  ( -9.808144436391993182, 0.000000000000000000, 10.77986332834118777 ) ) ;
#21748 = EDGE_CURVE ( 'NONE', #32511, #14988, #9288, .T. ) ;
#21749 = EDGE_CURVE ( 'NONE', #25259, #695, #5332, .T. ) ;
#21750 = LINE ( 'NONE', #13240, #23744 ) ;
#21751 = DIRECTION ( 'NONE',  ( -0.9999697198139514409, -0.000000000000000000, -0.007781995580013368816 ) ) ;
#21752 = EDGE_CURVE ( 'NONE', #39181, #9112, #6182, .T. ) ;
#21753 = DIRECTION ( 'NONE',  ( 0.5364919789714477361, 0.6444004775717706579, 0.5449076811759711036 ) ) ;
#21754 = FACE_OUTER_BOUND ( 'NONE', #46765, .T. ) ;
#21755 = ORIENTED_EDGE ( 'NONE', *, *, #51872, .T. ) ;
#21756 = CARTESIAN_POINT ( 'NONE',  ( -15.10957658656220737, 4.495856970884013037, 2.407563025325826445 ) ) ;
#21757 = PLANE ( 'NONE',  #30575 ) ;
#21758 = ORIENTED_EDGE ( 'NONE', *, *, #35861, .T. ) ;
#21759 = FACE_OUTER_BOUND ( 'NONE', #2356, .T. ) ;
#21760 = ORIENTED_EDGE ( 'NONE', *, *, #14952, .T. ) ;
#21761 = LINE ( 'NONE', #39076, #17727 ) ;
#21762 = VERTEX_POINT ( 'NONE', #35704 ) ;
#21763 = ORIENTED_EDGE ( 'NONE', *, *, #19730, .F. ) ;
#21764 = VERTEX_POINT ( 'NONE', #36012 ) ;
#21765 = EDGE_LOOP ( 'NONE', ( #46450, #12230, #45432, #13338, #28539 ) ) ;
#21766 = ORIENTED_EDGE ( 'NONE', *, *, #43366, .F. ) ;
#21767 = VERTEX_POINT ( 'NONE', #53021 ) ;
#21768 = CARTESIAN_POINT ( 'NONE',  ( -10.20725032438692992, 0.000000000000000000, 2.355653510902626646 ) ) ;
#21769 = CARTESIAN_POINT ( 'NONE',  ( -9.837237150914331707, -0.1191753592594208266, 1.668040315669363949 ) ) ;
#21770 = LINE ( 'NONE', #39375, #41255 ) ;
#21771 = VERTEX_POINT ( 'NONE', #44483 ) ;
#21772 = DIRECTION ( 'NONE',  ( 0.007781995580012662783, 0.000000000000000000, -0.9999697198139514409 ) ) ;
#21773 = VERTEX_POINT ( 'NONE', #49030 ) ;
#21774 = ORIENTED_EDGE ( 'NONE', *, *, #44760, .T. ) ;
#21775 = EDGE_CURVE ( 'NONE', #12727, #19669, #32816, .T. ) ;
#21776 = DIRECTION ( 'NONE',  ( -0.9999697198139514409, -0.000000000000000000, -0.007781995580013368816 ) ) ;
#21777 = ADVANCED_FACE ( 'NONE', ( #50438 ), #28025, .F. ) ;
#21778 = FACE_OUTER_BOUND ( 'NONE', #2785, .T. ) ;
#21779 = ADVANCED_FACE ( 'NONE', ( #41884 ), #24313, .F. ) ;
#21780 = VERTEX_POINT ( 'NONE', #33121 ) ;
#21781 = DIRECTION ( 'NONE',  ( 0.5449076811759707706, 0.6444004775717708799, -0.5364919789714476250 ) ) ;
#21782 = VERTEX_POINT ( 'NONE', #37351 ) ;
#21783 = CARTESIAN_POINT ( 'NONE',  ( -19.15181445782265257, -0.1191753592594170796, 4.402034235317630717 ) ) ;
#21784 = ADVANCED_FACE ( 'NONE', ( #24570 ), #20029, .F. ) ;
#21785 = CARTESIAN_POINT ( 'NONE',  ( -11.20636620717317378, 0.000000000000000000, 11.32298014792380414 ) ) ;
#21786 = VECTOR ( 'NONE', #6719, 999.9999999999998863 ) ;
#21787 = DIRECTION ( 'NONE',  ( -0.7660212471507179544, -0.6427876096865405842, -0.005961354470445141482 ) ) ;
#21788 = CARTESIAN_POINT ( 'NONE',  ( -17.74404816805336793, 0.000000000000000000, 3.574322630375089460 ) ) ;
#21789 = FACE_OUTER_BOUND ( 'NONE', #55274, .T. ) ;
#21790 = CARTESIAN_POINT ( 'NONE',  ( -19.72872274022425643, 0.000000000000000000, 5.974875909004076391 ) ) ;
#21791 = DIRECTION ( 'NONE',  ( 0.5449076811759707706, 0.6444004775717708799, -0.5364919789714476250 ) ) ;
#21792 = CARTESIAN_POINT ( 'NONE',  ( -69.74732653341585831, -11.70592520059384256, -8.307376767094716286 ) ) ;
#21793 = ORIENTED_EDGE ( 'NONE', *, *, #46284, .F. ) ;
#21794 = CARTESIAN_POINT ( 'NONE',  ( -56.75000000000000711, 6.050000000000001599, -2.449489742783172108 ) ) ;
#21795 = LINE ( 'NONE', #55586, #12030 ) ;
#21796 = DIRECTION ( 'NONE',  ( -0.000000000000000000, -0.000000000000000000, 1.000000000000000000 ) ) ;
#21797 = LINE ( 'NONE', #9028, #43547 ) ;
#21798 = CARTESIAN_POINT ( 'NONE',  ( -35.53815943785284759, 10.40825912036386214, -4.912923275970548787 ) ) ;
#21799 = LINE ( 'NONE', #25787, #38590 ) ;
#21800 = DIRECTION ( 'NONE',  ( 0.9999697198139515519, 0.000000000000000000, 0.007781995580013368816 ) ) ;
#21801 = DIRECTION ( 'NONE',  ( 0.007781995580012663651, -3.146120232559066537E-19, -0.9999697198139514409 ) ) ;
#21802 = ORIENTED_EDGE ( 'NONE', *, *, #42215, .F. ) ;
#21803 = CARTESIAN_POINT ( 'NONE',  ( -19.65908866086925144, 19.57604490793647400, 4.314202863308498337 ) ) ;
#21804 = CARTESIAN_POINT ( 'NONE',  ( 2.072287782118878319, 0.000000000000000000, -2.950529333540147015 ) ) ;
#21805 = EDGE_CURVE ( 'NONE', #10121, #41600, #15777, .T. ) ;
#21806 = CARTESIAN_POINT ( 'NONE',  ( -14.88655153574517520, 0.000000000000000000, 6.551216888352914047 ) ) ;
#21807 = EDGE_CURVE ( 'NONE', #27886, #48080, #28860, .T. ) ;
#21808 = DIRECTION ( 'NONE',  ( 0.9999697198139515519, 0.000000000000000000, 0.007781995580013368816 ) ) ;
#21809 = DIRECTION ( 'NONE',  ( 0.005961354470445682716, -0.6427876096865404731, -0.7660212471507180654 ) ) ;
#21810 = PLANE ( 'NONE',  #20606 ) ;
#21811 = EDGE_CURVE ( 'NONE', #45157, #41193, #2704, .T. ) ;
#21812 = EDGE_CURVE ( 'NONE', #49751, #46200, #36835, .T. ) ;
#21813 = PLANE ( 'NONE',  #30154 ) ;
#21814 = DIRECTION ( 'NONE',  ( 0.007781995580012662783, 0.000000000000000000, -0.9999697198139514409 ) ) ;
#21815 = FACE_OUTER_BOUND ( 'NONE', #7737, .T. ) ;
#21816 = ORIENTED_EDGE ( 'NONE', *, *, #37957, .F. ) ;
#21817 = DIRECTION ( 'NONE',  ( 0.9999697198139515519, 0.000000000000000000, 0.007781995580013368816 ) ) ;
#21818 = ORIENTED_EDGE ( 'NONE', *, *, #56142, .T. ) ;
#21819 = ADVANCED_FACE ( 'NONE', ( #7264 ), #2455, .F. ) ;
#21820 = VECTOR ( 'NONE', #6310, 999.9999999999998863 ) ;
#21821 = ORIENTED_EDGE ( 'NONE', *, *, #32626, .F. ) ;
#21822 = ORIENTED_EDGE ( 'NONE', *, *, #30660, .T. ) ;
#21823 = ORIENTED_EDGE ( 'NONE', *, *, #2464, .T. ) ;
#21824 = ORIENTED_EDGE ( 'NONE', *, *, #19158, .F. ) ;
#21825 = DIRECTION ( 'NONE',  ( 0.5449076811759707706, 0.6444004775717708799, -0.5364919789714476250 ) ) ;
#21826 = CARTESIAN_POINT ( 'NONE',  ( -13.93715936752603213, 0.000000000000000000, 3.973280789084581599 ) ) ;
#21827 = ORIENTED_EDGE ( 'NONE', *, *, #17303, .T. ) ;
#21828 = ORIENTED_EDGE ( 'NONE', *, *, #2563, .T. ) ;
#21829 = DIRECTION ( 'NONE',  ( 0.007781995580012663651, 0.000000000000000000, -0.9999697198139515519 ) ) ;
#21830 = ORIENTED_EDGE ( 'NONE', *, *, #7959, .T. ) ;
#21831 = LINE ( 'NONE', #46855, #54507 ) ;
#21832 = LINE ( 'NONE', #43161, #41438 ) ;
#21833 = ORIENTED_EDGE ( 'NONE', *, *, #18834, .T. ) ;
#21834 = DIRECTION ( 'NONE',  ( -0.005961354470445682716, -0.6427876096865404731, 0.7660212471507180654 ) ) ;
#21835 = EDGE_LOOP ( 'NONE', ( #22784, #31117, #31301, #19341 ) ) ;
#21836 = VECTOR ( 'NONE', #14510, 1000.000000000000227 ) ;
#21837 = LINE ( 'NONE', #29824, #3754 ) ;
#21838 = ADVANCED_FACE ( 'NONE', ( #19776 ), #32562, .F. ) ;
#21839 = CARTESIAN_POINT ( 'NONE',  ( -13.93009360612618508, 0.000000000000000000, 3.065345623274078779 ) ) ;
#21840 = ORIENTED_EDGE ( 'NONE', *, *, #15012, .F. ) ;
#21841 = CARTESIAN_POINT ( 'NONE',  ( -20.54204810873173415, 0.000000000000000000, 4.860550213503115558 ) ) ;
#21842 = CARTESIAN_POINT ( 'NONE',  ( -14.40699345105622697, 2.553033558614008047, 2.196642114320274786 ) ) ;
#21843 = CARTESIAN_POINT ( 'NONE',  ( -14.96720833274759244, -0.1191753592594192307, 4.065267737971954176 ) ) ;
#21844 = ORIENTED_EDGE ( 'NONE', *, *, #11879, .F. ) ;
#21845 = LINE ( 'NONE', #8521, #19236 ) ;
#21846 = EDGE_LOOP ( 'NONE', ( #38517, #30804, #19608, #36242, #37056 ) ) ;
#21847 = EDGE_CURVE ( 'NONE', #39433, #20494, #14755, .T. ) ;
#21848 = VECTOR ( 'NONE', #39162, 999.9999999999998863 ) ;
#21849 = CARTESIAN_POINT ( 'NONE',  ( -15.86710544311044302, 0.000000000000000000, 13.13336954653252953 ) ) ;
#21850 = CARTESIAN_POINT ( 'NONE',  ( -29.86352658060627618, 0.000000000000000000, 8.481329010720569883 ) ) ;
#21851 = LINE ( 'NONE', #38913, #20359 ) ;
#21852 = LINE ( 'NONE', #5393, #51356 ) ;
#21853 = CARTESIAN_POINT ( 'NONE',  ( -9.342070512798265725, 0.000000000000000000, 10.59882438848031505 ) ) ;
#21854 = EDGE_CURVE ( 'NONE', #36639, #16314, #49613, .T. ) ;
#21855 = DIRECTION ( 'NONE',  ( -1.000000000000000000, 0.000000000000000000, 0.000000000000000000 ) ) ;
#21857 = ADVANCED_FACE ( 'NONE', ( #23742 ), #41066, .F. ) ;
#21856 = DIRECTION ( 'NONE',  ( 0.005961354470445682716, -0.6427876096865404731, -0.7660212471507180654 ) ) ;
#21858 = AXIS2_PLACEMENT_3D ( 'NONE', #1341, #6727, #6452 ) ;
#21859 = DIRECTION ( 'NONE',  ( 0.5364919789714477361, 0.6444004775717706579, 0.5449076811759711036 ) ) ;
#21860 = CARTESIAN_POINT ( 'NONE',  ( -19.96228687206401631, 0.2864062442990046309, 5.105392700718557109 ) ) ;
#21861 = LINE ( 'NONE', #9673, #25085 ) ;
#21862 = ORIENTED_EDGE ( 'NONE', *, *, #21566, .F. ) ;
#21863 = DIRECTION ( 'NONE',  ( -0.005002170337468016433, -0.7660444431189770143, 0.6427681459581293666 ) ) ;
#21864 = EDGE_CURVE ( 'NONE', #37895, #46706, #49864, .T. ) ;
#21865 = CARTESIAN_POINT ( 'NONE',  ( -18.95841281422621094, -0.1191753592594164968, 8.835524169308294873 ) ) ;
#21866 = CARTESIAN_POINT ( 'NONE',  ( -11.93265391726099445, -1.489407457353155717, 3.761351127055128973 ) ) ;
#21867 = EDGE_CURVE ( 'NONE', #34742, #53438, #45600, .T. ) ;
#21868 = DIRECTION ( 'NONE',  ( 0.5364919789714477361, 0.6444004775717706579, 0.5449076811759711036 ) ) ;
#21869 = LINE ( 'NONE', #51434, #52304 ) ;
#21870 = EDGE_CURVE ( 'NONE', #24071, #10102, #50134, .T. ) ;
#21871 = CARTESIAN_POINT ( 'NONE',  ( -13.73672976910459909, 0.000000000000000000, 12.22661844811216270 ) ) ;
#21872 = ORIENTED_EDGE ( 'NONE', *, *, #28139, .F. ) ;
#21873 = ORIENTED_EDGE ( 'NONE', *, *, #51382, .F. ) ;
#21874 = FACE_OUTER_BOUND ( 'NONE', #23141, .T. ) ;
#21875 = CARTESIAN_POINT ( 'NONE',  ( -15.87975247367846166, 0.000000000000000000, 2.850166870931599927 ) ) ;
#21876 = EDGE_LOOP ( 'NONE', ( #35614, #40126, #38572, #39226 ) ) ;
#21877 = DIRECTION ( 'NONE',  ( 0.007781995580012663651, 0.000000000000000000, -0.9999697198139515519 ) ) ;
#21878 = EDGE_CURVE ( 'NONE', #34403, #31401, #28571, .T. ) ;
#21879 = VECTOR ( 'NONE', #21868, 999.9999999999998863 ) ;
#21880 = AXIS2_PLACEMENT_3D ( 'NONE', #34086, #38902, #4530 ) ;
#21881 = ORIENTED_EDGE ( 'NONE', *, *, #36688, .T. ) ;
#21882 = FACE_OUTER_BOUND ( 'NONE', #17185, .T. ) ;
#21883 = EDGE_LOOP ( 'NONE', ( #51777, #4075, #32999, #37154 ) ) ;
#21884 = CARTESIAN_POINT ( 'NONE',  ( -12.33850799832341849, 0.000000000000000000, 11.68350162852954632 ) ) ;
#21885 = EDGE_CURVE ( 'NONE', #1428, #12623, #55512, .T. ) ;
#21886 = ORIENTED_EDGE ( 'NONE', *, *, #5751, .F. ) ;
#21887 = ORIENTED_EDGE ( 'NONE', *, *, #34669, .F. ) ;
#21888 = ORIENTED_EDGE ( 'NONE', *, *, #37856, .T. ) ;
#21889 = DIRECTION ( 'NONE',  ( -0.005002170337468016433, -0.7660444431189770143, 0.6427681459581293666 ) ) ;
#21890 = CARTESIAN_POINT ( 'NONE',  ( -20.54049170961573267, 0.000000000000000000, 4.660556269540326646 ) ) ;
#21891 = CARTESIAN_POINT ( 'NONE',  ( -17.33903557990779021, -0.1159828484229830647, 9.953443831026842048 ) ) ;
#21892 = DIRECTION ( 'NONE',  ( -0.8531650599175527594, 0.4028455766673922356, 0.3313982828793700652 ) ) ;
#21893 = ORIENTED_EDGE ( 'NONE', *, *, #39223, .F. ) ;
#21894 = VERTEX_POINT ( 'NONE', #26267 ) ;
#21895 = VECTOR ( 'NONE', #14184, 999.9999999999998863 ) ;
#21896 = ORIENTED_EDGE ( 'NONE', *, *, #37981, .F. ) ;
#21897 = CARTESIAN_POINT ( 'NONE',  ( -31.72782227498118601, 0.000000000000000000, 9.205484770164058972 ) ) ;
#21898 = EDGE_LOOP ( 'NONE', ( #21881, #2597, #169, #12802 ) ) ;
#21899 = CARTESIAN_POINT ( 'NONE',  ( -20.98941955928877334, 2.067327705546508021, 4.768976514551538592 ) ) ;
#21900 = ORIENTED_EDGE ( 'NONE', *, *, #10574, .T. ) ;
#21901 = CARTESIAN_POINT ( 'NONE',  ( -18.19747506107908563, 0.000000000000000000, 14.03856424583689311 ) ) ;
#21902 = DIRECTION ( 'NONE',  ( 0.000000000000000000, -0.000000000000000000, -1.000000000000000000 ) ) ;
#21903 = VERTEX_POINT ( 'NONE', #3566 ) ;
#21904 = DIRECTION ( 'NONE',  ( 0.005961354470445682716, -0.6427876096865404731, -0.7660212471507180654 ) ) ;
#21905 = EDGE_CURVE ( 'NONE', #21764, #38457, #47014, .T. ) ;
#21906 = ORIENTED_EDGE ( 'NONE', *, *, #45337, .F. ) ;
#21907 = PLANE ( 'NONE',  #2865 ) ;
#21908 = VERTEX_POINT ( 'NONE', #43577 ) ;
#21909 = CYLINDRICAL_SURFACE ( 'NONE', #24112, 3.000000000000001332 ) ;
#21910 = DIRECTION ( 'NONE',  ( -0.005002170337468016433, -0.7660444431189770143, 0.6427681459581293666 ) ) ;
#21911 = CARTESIAN_POINT ( 'NONE',  ( -9.034769606752719895, 0.000000000000000000, 5.119428529189977262 ) ) ;
#21912 = ORIENTED_EDGE ( 'NONE', *, *, #12821, .T. ) ;
#21914 = CARTESIAN_POINT ( 'NONE',  ( -13.16292975041053026, -4.565544526780660917, 9.287697036052362520 ) ) ;
#21913 = AXIS2_PLACEMENT_3D ( 'NONE', #436, #43880, #38502 ) ;
#21915 = VECTOR ( 'NONE', #20925, 999.9999999999998863 ) ;
#21916 = FACE_OUTER_BOUND ( 'NONE', #1125, .T. ) ;
#21917 = DIRECTION ( 'NONE',  ( -0.5449076811759708816, 0.6444004775717707689, 0.5364919789714475140 ) ) ;
#21918 = DIRECTION ( 'NONE',  ( 0.000000000000000000, -0.000000000000000000, -1.000000000000000000 ) ) ;
#21919 = PLANE ( 'NONE',  #45789 ) ;
#21921 = EDGE_CURVE ( 'NONE', #53352, #12064, #20873, .T. ) ;
#21920 = DIRECTION ( 'NONE',  ( 0.9999697198139515519, 0.000000000000000000, 0.007781995580013368816 ) ) ;
#21922 = SURFACE_SIDE_STYLE ('',( #52027 ) ) ;
#21923 = VECTOR ( 'NONE', #16945, 1000.000000000000227 ) ;
#21924 = EDGE_LOOP ( 'NONE', ( #37535, #46259, #10999, #14838 ) ) ;
#21925 = LINE ( 'NONE', #55738, #28895 ) ;
#21926 = FACE_OUTER_BOUND ( 'NONE', #48298, .T. ) ;
#21927 = LINE ( 'NONE', #27305, #44130 ) ;
#21928 = ORIENTED_EDGE ( 'NONE', *, *, #41738, .T. ) ;
#21929 = CARTESIAN_POINT ( 'NONE',  ( -18.19747506107908563, 0.000000000000000000, 14.03856424583689311 ) ) ;
#21930 = CARTESIAN_POINT ( 'NONE',  ( -17.36532418587302473, -0.1191753592594177458, 13.67570816655714516 ) ) ;
#21931 = ORIENTED_EDGE ( 'NONE', *, *, #54485, .T. ) ;
#21932 = LINE ( 'NONE', #52341, #33435 ) ;
#21933 = EDGE_CURVE ( 'NONE', #18224, #13159, #38194, .T. ) ;
#21934 = LINE ( 'NONE', #1186, #17589 ) ;
#21935 = VECTOR ( 'NONE', #7594, 1000.000000000000114 ) ;
#21936 = DIRECTION ( 'NONE',  ( -0.005002170337468016433, -0.7660444431189770143, 0.6427681459581293666 ) ) ;
#21937 = AXIS2_PLACEMENT_3D ( 'NONE', #16377, #11839, #3345 ) ;
#21938 = EDGE_CURVE ( 'NONE', #41541, #39671, #55814, .T. ) ;
#21939 = LINE ( 'NONE', #35035, #6633 ) ;
#21940 = ORIENTED_EDGE ( 'NONE', *, *, #3982, .F. ) ;
#21941 = ORIENTED_EDGE ( 'NONE', *, *, #27597, .F. ) ;
#21942 = CARTESIAN_POINT ( 'NONE',  ( -16.35824496976556830, -0.1191753592594197164, 3.685110299410161439 ) ) ;
#21943 = DIRECTION ( 'NONE',  ( -0.5449076811759708816, 0.6444004775717707689, 0.5364919789714475140 ) ) ;
#21944 = CARTESIAN_POINT ( 'NONE',  ( -23.33849165029409889, 0.000000000000000000, 5.946783852668351855 ) ) ;
#21945 = FACE_OUTER_BOUND ( 'NONE', #17686, .T. ) ;
#21946 = EDGE_CURVE ( 'NONE', #21366, #40198, #42732, .T. ) ;
#21947 = LINE ( 'NONE', #55760, #8344 ) ;
#21948 = PLANE ( 'NONE',  #53949 ) ;
#21949 = ORIENTED_EDGE ( 'NONE', *, *, #42422, .T. ) ;
#21950 = LINE ( 'NONE', #39280, #25598 ) ;
#21951 = EDGE_CURVE ( 'NONE', #47914, #26746, #118, .T. ) ;
#21952 = DIRECTION ( 'NONE',  ( -0.6427681459581293666, -0.7660444431189770143, -0.005002170337467561935 ) ) ;
#21953 = ORIENTED_EDGE ( 'NONE', *, *, #48359, .T. ) ;
#21954 = B_SPLINE_CURVE_WITH_KNOTS ( 'NONE', 3,
 ( #40259, #22936, #14984, #31746 ),
 .UNSPECIFIED., .F., .F.,
 ( 4, 4 ),
 ( 0.000000000000000000, 0.0002393041340872677626 ),
 .UNSPECIFIED. ) ;
#21955 = FACE_OUTER_BOUND ( 'NONE', #31933, .T. ) ;
#21956 = PLANE ( 'NONE',  #579 ) ;
#21957 = LINE ( 'NONE', #30781, #36643 ) ;
#21958 = ORIENTED_EDGE ( 'NONE', *, *, #46105, .F. ) ;
#21959 = VECTOR ( 'NONE', #14304, 999.9999999999998863 ) ;
#21960 = VECTOR ( 'NONE', #6292, 1000.000000000000227 ) ;
#21961 = CARTESIAN_POINT ( 'NONE',  ( -19.60990026154428278, 0.000000000000000000, 4.498472333781370125 ) ) ;
#21962 = ORIENTED_EDGE ( 'NONE', *, *, #39939, .T. ) ;
#21963 = VERTEX_POINT ( 'NONE', #29716 ) ;
#21964 = VECTOR ( 'NONE', #11268, 1000.000000000000227 ) ;
#21965 = ORIENTED_EDGE ( 'NONE', *, *, #12443, .T. ) ;
#21966 = VECTOR ( 'NONE', #53628, 1000.000000000000227 ) ;
#21967 = ORIENTED_EDGE ( 'NONE', *, *, #7300, .F. ) ;
#21968 = PLANE ( 'NONE',  #13036 ) ;
#21970 = EDGE_CURVE ( 'NONE', #52222, #9899, #25424, .T. ) ;
#21969 = VERTEX_POINT ( 'NONE', #16330 ) ;
#21971 = LINE ( 'NONE', #4944, #12225 ) ;
#21972 = ORIENTED_EDGE ( 'NONE', *, *, #32420, .F. ) ;
#21973 = CARTESIAN_POINT ( 'NONE',  ( -22.04728230093569152, 19.65758605842115969, -4.422151119964278010 ) ) ;
#21974 = VERTEX_POINT ( 'NONE', #3831 ) ;
#21976 = VECTOR ( 'NONE', #27433, 1000.000000000000114 ) ;
#21975 = LINE ( 'NONE', #694, #41135 ) ;
#21977 = ADVANCED_FACE ( 'NONE', ( #8119 ), #51556, .F. ) ;
#21978 = ORIENTED_EDGE ( 'NONE', *, *, #29109, .T. ) ;
#21979 = EDGE_CURVE ( 'NONE', #20361, #13581, #43330, .T. ) ;
#21980 = CARTESIAN_POINT ( 'NONE',  ( -16.73360290908838977, 0.000000000000000000, 5.059514428249818785 ) ) ;
#21981 = CARTESIAN_POINT ( 'NONE',  ( -23.44701637808619665, 18.93456746265863799, 4.495868649597294819 ) ) ;
#21982 = EDGE_CURVE ( 'NONE', #15779, #41229, #38788, .T. ) ;
#21983 = DIRECTION ( 'NONE',  ( 0.9999697198139515519, 0.000000000000000000, 0.007781995580013368816 ) ) ;
#21984 = DIRECTION ( 'NONE',  ( 0.000000000000000000, -5.782411586589354681E-16, 1.000000000000000000 ) ) ;
#21985 = CARTESIAN_POINT ( 'NONE',  ( -19.05009385693719537, 0.000000000000000000, 4.181329822281151465 ) ) ;
#21986 = VERTEX_POINT ( 'NONE', #16927 ) ;
#21987 = EDGE_CURVE ( 'NONE', #4219, #26092, #52889, .T. ) ;
#21988 = ADVANCED_FACE ( 'NONE', ( #34252 ), #12655, .F. ) ;
#21989 = EDGE_CURVE ( 'NONE', #50478, #50472, #13219, .T. ) ;
#21990 = EDGE_LOOP ( 'NONE', ( #31191, #24212, #13508, #13881 ) ) ;
#21991 = DIRECTION ( 'NONE',  ( 0.9999697198139515519, 0.000000000000000000, 0.007781995580013368816 ) ) ;
#21992 = FACE_OUTER_BOUND ( 'NONE', #20822, .T. ) ;
#21993 = VECTOR ( 'NONE', #28933, 1000.000000000000000 ) ;
#21994 = LINE ( 'NONE', #706, #4312 ) ;
#21995 = DIRECTION ( 'NONE',  ( 0.6427681459581294776, -0.7660444431189769032, 0.005002170337467562802 ) ) ;
#21996 = DIRECTION ( 'NONE',  ( -0.9321478471874540261, 0.000000000000000000, 0.3620778797217457656 ) ) ;
#21997 = PLANE ( 'NONE',  #5999 ) ;
#21998 = ORIENTED_EDGE ( 'NONE', *, *, #54975, .F. ) ;
#22000 = DIRECTION ( 'NONE',  ( 2.551063935260010306E-17, -5.102127870520020982E-16, 1.000000000000000000 ) ) ;
#21999 = AXIS2_PLACEMENT_3D ( 'NONE', #2404, #54094, #49823 ) ;
#22001 = DIRECTION ( 'NONE',  ( 0.000000000000000000, 0.000000000000000000, 1.000000000000000000 ) ) ;
#22002 = ORIENTED_EDGE ( 'NONE', *, *, #15401, .T. ) ;
#22003 = VECTOR ( 'NONE', #55071, 999.9999999999998863 ) ;
#22004 = VECTOR ( 'NONE', #45077, 1000.000000000000114 ) ;
#22005 = CARTESIAN_POINT ( 'NONE',  ( -11.40636015113596180, 0.000000000000000000, 11.32142374880780089 ) ) ;
#22006 = CARTESIAN_POINT ( 'NONE',  ( -22.15667627784559812, -4.727446477803161073, 13.04688230017630346 ) ) ;
#22007 = EDGE_CURVE ( 'NONE', #45145, #28385, #50965, .T. ) ;
#22008 = CARTESIAN_POINT ( 'NONE',  ( -15.54543426953848595, 0.000000000000000000, 5.807425170953373517 ) ) ;
#22009 = LINE ( 'NONE', #47870, #55013 ) ;
#22010 = EDGE_CURVE ( 'NONE', #11344, #30714, #7850, .T. ) ;
#22011 = DIRECTION ( 'NONE',  ( -0.6427681459581293666, -0.7660444431189770143, -0.005002170337467561935 ) ) ;
#22012 = ORIENTED_EDGE ( 'NONE', *, *, #45164, .T. ) ;
#22013 = VECTOR ( 'NONE', #32524, 999.9999999999998863 ) ;
#22014 = VECTOR ( 'NONE', #20389, 1000.000000000000227 ) ;
#22015 = ORIENTED_EDGE ( 'NONE', *, *, #23716, .F. ) ;
#22016 = ADVANCED_FACE ( 'NONE', ( #43030 ), #4142, .F. ) ;
#22017 = LINE ( 'NONE', #31403, #13990 ) ;
#22018 = CARTESIAN_POINT ( 'NONE',  ( -20.54126990917373519, -0.1191753592594197858, 4.760553241521720658 ) ) ;
#22019 = FACE_OUTER_BOUND ( 'NONE', #37485, .T. ) ;
#22020 = ADVANCED_FACE ( 'NONE', ( #40160 ), #39331, .F. ) ;
#22021 = PLANE ( 'NONE',  #45462 ) ;
#22022 = VECTOR ( 'NONE', #22690, 999.9999999999998863 ) ;
#22023 = CARTESIAN_POINT ( 'NONE',  ( -46.52156441860518754, 5.799038105676674881, 5.000000000000000000 ) ) ;
#22025 = VECTOR ( 'NONE', #2339, 1000.000000000000227 ) ;
#22024 = CARTESIAN_POINT ( 'NONE',  ( 2.072287782118878319, 0.000000000000000000, -2.950529333540147015 ) ) ;
#22026 = CARTESIAN_POINT ( 'NONE',  ( -26.13493519185646008, 0.000000000000000000, 7.033017491833586377 ) ) ;
#22027 = ORIENTED_EDGE ( 'NONE', *, *, #18691, .F. ) ;
#22028 = DIRECTION ( 'NONE',  ( -0.000000000000000000, -0.000000000000000000, 1.000000000000000000 ) ) ;
#22029 = PLANE ( 'NONE',  #45082 ) ;
#22030 = EDGE_LOOP ( 'NONE', ( #44668, #1807, #36517, #38167 ) ) ;
#22031 = FACE_OUTER_BOUND ( 'NONE', #14180, .T. ) ;
#22032 = EDGE_LOOP ( 'NONE', ( #1992, #4584, #50108, #47547 ) ) ;
#22033 = LINE ( 'NONE', #18059, #27749 ) ;
#22034 = AXIS2_PLACEMENT_3D ( 'NONE', #31976, #40784, #31134 ) ;
#22035 = CARTESIAN_POINT ( 'NONE',  ( -19.60990026154428278, 0.000000000000000000, 4.498472333781370125 ) ) ;
#22036 = ORIENTED_EDGE ( 'NONE', *, *, #41643, .T. ) ;
#22037 = VECTOR ( 'NONE', #852, 1000.000000000000227 ) ;
#22038 = ORIENTED_EDGE ( 'NONE', *, *, #4342, .T. ) ;
#22039 = ORIENTED_EDGE ( 'NONE', *, *, #44959, .T. ) ;
#22040 = ORIENTED_EDGE ( 'NONE', *, *, #4648, .F. ) ;
#22041 = ORIENTED_EDGE ( 'NONE', *, *, #47821, .F. ) ;
#22042 = EDGE_LOOP ( 'NONE', ( #40824, #2550, #12418, #56129 ) ) ;
#22043 = VECTOR ( 'NONE', #46307, 1000.000000000000114 ) ;
#22044 = DIRECTION ( 'NONE',  ( -0.7660212471507179544, -0.6427876096865405842, -0.005961354470445141482 ) ) ;
#22045 = DIRECTION ( 'NONE',  ( 0.007781995580012663651, -3.146120232559066537E-19, -0.9999697198139514409 ) ) ;
#22046 = CARTESIAN_POINT ( 'NONE',  ( -19.60990026154428278, 0.000000000000000000, 4.498472333781370125 ) ) ;
#22047 = VECTOR ( 'NONE', #3054, 999.9999999999998863 ) ;
#22048 = VECTOR ( 'NONE', #50058, 1000.000000000000227 ) ;
#22049 = ORIENTED_EDGE ( 'NONE', *, *, #40054, .T. ) ;
#22050 = LINE ( 'NONE', #30851, #4077 ) ;
#22051 = EDGE_LOOP ( 'NONE', ( #31057, #41665, #42443, #43068 ) ) ;
#22052 = EDGE_LOOP ( 'NONE', ( #54057, #21755, #39601, #27491 ) ) ;
#22053 = VECTOR ( 'NONE', #17640, 1000.000000000000000 ) ;
#22054 = AXIS2_PLACEMENT_3D ( 'NONE', #28285, #45603, #6717 ) ;
#22055 = DIRECTION ( 'NONE',  ( 0.007781995580012663651, 0.000000000000000000, -0.9999697198139515519 ) ) ;
#22056 = DIRECTION ( 'NONE',  ( -0.005961354470445682716, -0.6427876096865404731, 0.7660212471507180654 ) ) ;
#22057 = LINE ( 'NONE', #35402, #24123 ) ;
#22058 = ORIENTED_EDGE ( 'NONE', *, *, #35705, .F. ) ;
#22059 = PLANE ( 'NONE',  #50049 ) ;
#22060 = EDGE_LOOP ( 'NONE', ( #5562, #11794, #25748, #51037 ) ) ;
#22061 = EDGE_CURVE ( 'NONE', #48671, #47896, #27676, .T. ) ;
#22062 = EDGE_CURVE ( 'NONE', #45380, #4591, #1556, .T. ) ;
#22063 = CARTESIAN_POINT ( 'NONE',  ( -16.99924723426068951, 0.000000000000000000, 13.49389102713827171 ) ) ;
#22064 = VECTOR ( 'NONE', #20732, 1000.000000000000227 ) ;
#22065 = LINE ( 'NONE', #17236, #23007 ) ;
#22066 = EDGE_CURVE ( 'NONE', #7431, #22114, #48706, .T. ) ;
#22067 = VECTOR ( 'NONE', #43746, 1000.000000000000227 ) ;
#22068 = DIRECTION ( 'NONE',  ( 0.005961354470445682716, -0.6427876096865404731, -0.7660212471507180654 ) ) ;
#22069 = LINE ( 'NONE', #18088, #33147 ) ;
#22070 = CARTESIAN_POINT ( 'NONE',  ( -28.93137873341882127, 0.000000000000000000, 8.119251130998824451 ) ) ;
#22071 = CARTESIAN_POINT ( 'NONE',  ( -21.93567689722629765, 19.99370688441071309, -4.657437592157546824 ) ) ;
#22072 = CARTESIAN_POINT ( 'NONE',  ( -20.84574850008768010, -5.375054281893163477, 13.60050816780225347 ) ) ;
#22073 = LINE ( 'NONE', #39405, #45817 ) ;
#22074 = VERTEX_POINT ( 'NONE', #10355 ) ;
#22075 = CARTESIAN_POINT ( 'NONE',  ( -63.56784591066751489, 8.775889882925216767, -3.000000000000000000 ) ) ;
#22076 = VECTOR ( 'NONE', #13481, 999.9999999999998863 ) ;
#22077 = CARTESIAN_POINT ( 'NONE',  ( -21.06965149344186372, 20.49370688441071664, -4.356725136697556344 ) ) ;
#22078 = DIRECTION ( 'NONE',  ( -0.7660212471507179544, -0.6427876096865405842, -0.005961354470445141482 ) ) ;
#22079 = DIRECTION ( 'NONE',  ( 0.5449076811759707706, 0.6444004775717708799, -0.5364919789714476250 ) ) ;
#22080 = AXIS2_PLACEMENT_3D ( 'NONE', #3238, #20570, #37891 ) ;
#22081 = CARTESIAN_POINT ( 'NONE',  ( -42.10458952830071411, 6.617128940028910833, -4.991983769317021924 ) ) ;
#22082 = PLANE ( 'NONE',  #25914 ) ;
#22083 = ADVANCED_FACE ( 'NONE', ( #6118 ), #9513, .F. ) ;
#22084 = CARTESIAN_POINT ( 'NONE',  ( -14.46888367232926420, 0.000000000000000000, 12.59025272694991315 ) ) ;
#22085 = PLANE ( 'NONE',  #21190 ) ;
#22086 = VERTEX_POINT ( 'NONE', #36201 ) ;
#22087 = EDGE_CURVE ( 'NONE', #44387, #38521, #10062, .T. ) ;
#22088 = VECTOR ( 'NONE', #6146, 1000.000000000000000 ) ;
#22089 = CARTESIAN_POINT ( 'NONE',  ( -26.13337879274045505, 0.000000000000000000, 6.833023547870798353 ) ) ;
#22090 = CARTESIAN_POINT ( 'NONE',  ( -17.21129241906660923, 0.000000000000000000, 6.733131273475654766 ) ) ;
#22091 = CARTESIAN_POINT ( 'NONE',  ( -11.30636317915456779, -0.1191753592594197858, 11.32220194836580340 ) ) ;
#22092 = VECTOR ( 'NONE', #35010, 999.9999999999998863 ) ;
#22093 = AXIS2_PLACEMENT_3D ( 'NONE', #32374, #27241, #28085 ) ;
#22094 = EDGE_CURVE ( 'NONE', #40769, #5645, #52945, .T. ) ;
#22095 = DIRECTION ( 'NONE',  ( 0.7660212471507180654, -0.6427876096865404731, 0.005961354470445141482 ) ) ;
#22096 = DIRECTION ( 'NONE',  ( 0.007781995580012662783, 0.000000000000000000, -0.9999697198139514409 ) ) ;
#22097 = DIRECTION ( 'NONE',  ( -0.9321478471874540261, 0.000000000000000000, 0.3620778797217457656 ) ) ;
#22098 = LINE ( 'NONE', #5074, #41054 ) ;
#22099 = AXIS2_PLACEMENT_3D ( 'NONE', #42554, #51058, #25504 ) ;
#22100 = VECTOR ( 'NONE', #31794, 1000.000000000000227 ) ;
#22101 = LINE ( 'NONE', #8791, #40503 ) ;
#22102 = LINE ( 'NONE', #30354, #24710 ) ;
#22103 = ADVANCED_FACE ( 'NONE', ( #31663 ), #18291, .F. ) ;
#22104 = EDGE_LOOP ( 'NONE', ( #34213, #11506, #34276, #39058 ) ) ;
#22105 = ORIENTED_EDGE ( 'NONE', *, *, #36952, .T. ) ;
#22106 = ORIENTED_EDGE ( 'NONE', *, *, #37856, .F. ) ;
#22107 = ORIENTED_EDGE ( 'NONE', *, *, #1289, .F. ) ;
#22108 = VECTOR ( 'NONE', #52076, 1000.000000000000000 ) ;
#22109 = ORIENTED_EDGE ( 'NONE', *, *, #55023, .F. ) ;
#22110 = CARTESIAN_POINT ( 'NONE',  ( -16.82288186660665374, -0.1191753592594196887, 3.681494387642152422 ) ) ;
#22111 = DIRECTION ( 'NONE',  ( -0.9999697198139514409, -0.000000000000000000, -0.007781995580013368816 ) ) ;
#22112 = VECTOR ( 'NONE', #31774, 999.9999999999998863 ) ;
#22113 = ORIENTED_EDGE ( 'NONE', *, *, #21176, .T. ) ;
#22114 = VERTEX_POINT ( 'NONE', #18590 ) ;
#22115 = VECTOR ( 'NONE', #6711, 999.9999999999998863 ) ;
#22116 = CARTESIAN_POINT ( 'NONE',  ( -65.59431828190201941, -5.464378949326942347E-14, 0.3363546178748699211 ) ) ;
#22117 = EDGE_LOOP ( 'NONE', ( #43751, #44977, #21163, #26430 ) ) ;
#22118 = VECTOR ( 'NONE', #46609, 1000.000000000000000 ) ;
#22119 = CARTESIAN_POINT ( 'NONE',  ( -16.53317331066696383, 0.000000000000000000, 13.31285208727739899 ) ) ;
#22120 = CARTESIAN_POINT ( 'NONE',  ( 2.072287782118878319, 0.000000000000000000, -2.950529333540147015 ) ) ;
#22121 = ORIENTED_EDGE ( 'NONE', *, *, #17648, .T. ) ;
#22122 = LINE ( 'NONE', #53072, #39290 ) ;
#22123 = VECTOR ( 'NONE', #11378, 1000.000000000000227 ) ;
#22125 = ORIENTED_EDGE ( 'NONE', *, *, #46750, .T. ) ;
#22124 = EDGE_CURVE ( 'NONE', #30466, #46454, #23138, .T. ) ;
#22126 = DIRECTION ( 'NONE',  ( -0.9999697198139514409, -0.000000000000000000, -0.007781995580013368816 ) ) ;
#22127 = ADVANCED_FACE ( 'NONE', ( #5522 ), #40467, .F. ) ;
#22128 = ADVANCED_FACE ( 'NONE', ( #48967 ), #13498, .F. ) ;
#22129 = VECTOR ( 'NONE', #10104, 999.9999999999998863 ) ;
#22130 = CARTESIAN_POINT ( 'NONE',  ( -11.59385650878361673, 0.000000000000000000, 1.406192425120281309 ) ) ;
#22131 = DIRECTION ( 'NONE',  ( -0.7660212471507179544, -0.6427876096865405842, -0.005961354470445141482 ) ) ;
#22132 = VECTOR ( 'NONE', #131, 999.9999999999998863 ) ;
#22133 = ORIENTED_EDGE ( 'NONE', *, *, #11573, .F. ) ;
#22134 = FACE_OUTER_BOUND ( 'NONE', #19091, .T. ) ;
#22135 = DIRECTION ( 'NONE',  ( -0.9999697198139514409, -0.000000000000000000, -0.007781995580013368816 ) ) ;
#22136 = PLANE ( 'NONE',  #32985 ) ;
#22137 = ORIENTED_EDGE ( 'NONE', *, *, #3582, .T. ) ;
#22138 = CARTESIAN_POINT ( 'NONE',  ( 1.086233639165236964, 0.000000000000000000, 2.796443541562362078 ) ) ;
#22139 = VERTEX_POINT ( 'NONE', #26837 ) ;
#22140 = CARTESIAN_POINT ( 'NONE',  ( -21.47263955680318404, 0.000000000000000000, 5.022634149262071190 ) ) ;
#22141 = CARTESIAN_POINT ( 'NONE',  ( -12.15546023705834244, 3.200641362704010007, 1.301408072064137222 ) ) ;
#22142 = PLANE ( 'NONE',  #468 ) ;
#22143 = LINE ( 'NONE', #52257, #40460 ) ;
#22144 = CARTESIAN_POINT ( 'NONE',  ( -16.99924723426068951, 0.000000000000000000, 13.49389102713827171 ) ) ;
#22145 = PLANE ( 'NONE',  #46688 ) ;
#22146 = CARTESIAN_POINT ( 'NONE',  ( -22.02230563637845151, 19.67040402849924163, -4.420763475398227449 ) ) ;
#22147 = ADVANCED_FACE ( 'NONE', ( #35629 ), #39634, .F. ) ;
#22148 = VECTOR ( 'NONE', #7249, 1000.000000000000114 ) ;
#22149 = PLANE ( 'NONE',  #7528 ) ;
#22150 = VECTOR ( 'NONE', #51778, 1000.000000000000114 ) ;
#22151 =( NAMED_UNIT ( * ) SI_UNIT ( $, .STERADIAN. ) SOLID_ANGLE_UNIT ( ) );
#22152 = LINE ( 'NONE', #5133, #11457 ) ;
#22153 = ORIENTED_EDGE ( 'NONE', *, *, #17947, .F. ) ;
#22154 = FACE_OUTER_BOUND ( 'NONE', #55485, .T. ) ;
#22155 = DIRECTION ( 'NONE',  ( -0.005961354470445682716, -0.6427876096865404731, 0.7660212471507180654 ) ) ;
#22156 = VECTOR ( 'NONE', #40457, 1000.000000000000227 ) ;
#22157 = CARTESIAN_POINT ( 'NONE',  ( -12.51706054884368413, -1.651309408375659871, 1.690687099836828411 ) ) ;
#22158 = DIRECTION ( 'NONE',  ( 0.005961354470445682716, -0.6427876096865404731, -0.7660212471507180654 ) ) ;
#22159 = EDGE_CURVE ( 'NONE', #2187, #9472, #44164, .T. ) ;
#22160 = CARTESIAN_POINT ( 'NONE',  ( -11.20636620717317378, 0.000000000000000000, 11.32298014792380414 ) ) ;
#22161 = DIRECTION ( 'NONE',  ( -0.8531650599175527594, 0.4028455766673922356, 0.3313982828793700652 ) ) ;
#22162 = ORIENTED_EDGE ( 'NONE', *, *, #55468, .T. ) ;
#22163 = VERTEX_POINT ( 'NONE', #35098 ) ;
#22164 = ADVANCED_FACE ( 'NONE', ( #31922 ), #967, .F. ) ;
#22165 = DIRECTION ( 'NONE',  ( -0.3620778797217455991, 0.000000000000000000, -0.9321478471874540261 ) ) ;
#22166 = VECTOR ( 'NONE', #8212, 1000.000000000000000 ) ;
#22167 = CARTESIAN_POINT ( 'NONE',  ( -14.14733187112066837, 0.000000000000000000, 5.279647443704662102 ) ) ;
#22168 = AXIS2_PLACEMENT_3D ( 'NONE', #11464, #2905, #50352 ) ;
#22169 = PLANE ( 'NONE',  #52921 ) ;
#22170 = VERTEX_POINT ( 'NONE', #711 ) ;
#22171 = LINE ( 'NONE', #26418, #35849 ) ;
#22172 = EDGE_CURVE ( 'NONE', #18484, #38141, #18031, .T. ) ;
#22173 = ORIENTED_EDGE ( 'NONE', *, *, #41357, .T. ) ;
#22174 = CARTESIAN_POINT ( 'NONE',  ( -19.07115766082023356, 0.000000000000000000, 6.887983385698593253 ) ) ;
#22175 = VECTOR ( 'NONE', #35119, 1000.000000000000227 ) ;
#22176 = ORIENTED_EDGE ( 'NONE', *, *, #2516, .T. ) ;
#22177 = VECTOR ( 'NONE', #18238, 1000.000000000000227 ) ;
#22178 = ORIENTED_EDGE ( 'NONE', *, *, #13363, .F. ) ;
#22179 = ORIENTED_EDGE ( 'NONE', *, *, #28227, .T. ) ;
#22180 = LINE ( 'NONE', #42626, #48350 ) ;
#22181 = DIRECTION ( 'NONE',  ( -0.9983709377222390602, -0.05705673239519638146, 0.000000000000000000 ) ) ;
#22182 = FACE_OUTER_BOUND ( 'NONE', #27434, .T. ) ;
#22183 = CARTESIAN_POINT ( 'NONE',  ( 0.000000000000000000, 2.000000000000000000, -2.125000000000000000 ) ) ;
#22184 = ORIENTED_EDGE ( 'NONE', *, *, #21401, .T. ) ;
#22185 = EDGE_LOOP ( 'NONE', ( #52747, #42113, #39936, #43513 ) ) ;
#22186 = EDGE_CURVE ( 'NONE', #47891, #52648, #32503, .T. ) ;
#22187 = VECTOR ( 'NONE', #32309, 1000.000000000000227 ) ;
#22188 = DIRECTION ( 'NONE',  ( -0.005961354470445682716, -0.6427876096865404731, 0.7660212471507180654 ) ) ;
#22189 = VECTOR ( 'NONE', #41480, 1000.000000000000227 ) ;
#22190 = ORIENTED_EDGE ( 'NONE', *, *, #16662, .T. ) ;
#22191 = PLANE ( 'NONE',  #4676 ) ;
#22192 = EDGE_CURVE ( 'NONE', #17429, #12259, #49804, .T. ) ;
#22193 = ORIENTED_EDGE ( 'NONE', *, *, #24928, .F. ) ;
#22194 = AXIS2_PLACEMENT_3D ( 'NONE', #44610, #5727, #1170 ) ;
#22195 = LINE ( 'NONE', #39531, #2449 ) ;
#22196 = CARTESIAN_POINT ( 'NONE',  ( -18.67697421479882181, -0.1191753592594197858, 4.036397482078229793 ) ) ;
#22197 = ORIENTED_EDGE ( 'NONE', *, *, #54878, .F. ) ;
#22198 = EDGE_CURVE ( 'NONE', #3650, #5725, #16014, .T. ) ;
#22199 = DIRECTION ( 'NONE',  ( 0.005961354470445682716, -0.6427876096865404731, -0.7660212471507180654 ) ) ;
#22200 = AXIS2_PLACEMENT_3D ( 'NONE', #39463, #564, #35215 ) ;
#22201 = EDGE_LOOP ( 'NONE', ( #38133, #26654, #14844, #35558 ) ) ;
#22202 = EDGE_CURVE ( 'NONE', #46872, #51258, #23672, .T. ) ;
#22203 = DIRECTION ( 'NONE',  ( -0.2426528472758541499, 0.7422098413412800966, -0.6246952433987894571 ) ) ;
#22204 = AXIS2_PLACEMENT_3D ( 'NONE', #48943, #23107, #13728 ) ;
#22205 = MECHANICAL_DESIGN_GEOMETRIC_PRESENTATION_REPRESENTATION (  '', ( #18602 ), #53937 ) ;
#22206 = EDGE_LOOP ( 'NONE', ( #16049, #19388, #37192, #54223 ) ) ;
#22207 = CARTESIAN_POINT ( 'NONE',  ( -25.20123094555300369, 0.000000000000000000, 6.470945668149052032 ) ) ;
#22208 = LINE ( 'NONE', #14269, #31200 ) ;
#22209 = VECTOR ( 'NONE', #47465, 1000.000000000000000 ) ;
#22210 = CARTESIAN_POINT ( 'NONE',  ( -16.81345671998191449, 0.000000000000000000, 3.412238694616132495 ) ) ;
#22211 = ORIENTED_EDGE ( 'NONE', *, *, #15614, .T. ) ;
#22212 = VECTOR ( 'NONE', #30935, 1000.000000000000114 ) ;
#22213 = ADVANCED_FACE ( 'NONE', ( #33339 ), #19131, .F. ) ;
#22214 = LINE ( 'NONE', #27820, #18389 ) ;
#22215 = FACE_OUTER_BOUND ( 'NONE', #14038, .T. ) ;
#22216 = CARTESIAN_POINT ( 'NONE',  ( -19.25965539076188904, 0.000000000000000000, 5.409188173551533474 ) ) ;
#22217 = PLANE ( 'NONE',  #51307 ) ;
#22218 = DIRECTION ( 'NONE',  ( -0.6427681459581293666, -0.7660444431189770143, -0.005002170337467561935 ) ) ;
#22219 = CARTESIAN_POINT ( 'NONE',  ( 2.072287782118878319, -1.000000000000000000, -2.950529333540147015 ) ) ;
#22220 = EDGE_CURVE ( 'NONE', #33548, #17624, #33043, .T. ) ;
#22221 = VECTOR ( 'NONE', #983, 1000.000000000000227 ) ;
#22222 = VECTOR ( 'NONE', #4970, 999.9999999999998863 ) ;
#22223 = EDGE_LOOP ( 'NONE', ( #25337, #41376, #27328, #5970 ) ) ;
#22224 = LINE ( 'NONE', #4611, #28016 ) ;
#22225 = CARTESIAN_POINT ( 'NONE',  ( -9.808144436391993182, 0.000000000000000000, 10.77986332834118777 ) ) ;
#22226 = DIRECTION ( 'NONE',  ( 0.007781995580012663651, -3.146120232559066537E-19, -0.9999697198139514409 ) ) ;
#22227 = VERTEX_POINT ( 'NONE', #2644 ) ;
#22228 = PLANE ( 'NONE',  #33844 ) ;
#22229 = DIRECTION ( 'NONE',  ( 0.6427681459581294776, -0.7660444431189769032, 0.005002170337467562802 ) ) ;
#22230 = ORIENTED_EDGE ( 'NONE', *, *, #34646, .T. ) ;
#22231 = CARTESIAN_POINT ( 'NONE',  ( -12.21285141497871152, 2.714935509636508204, 1.339197314243185222 ) ) ;
#22232 = DIRECTION ( 'NONE',  ( -0.6427681459581293666, -0.7660444431189770143, -0.005002170337467561935 ) ) ;
#22233 = DIRECTION ( 'NONE',  ( -0.6427681459581293666, -0.7660444431189770143, -0.005002170337467561935 ) ) ;
#22234 = CARTESIAN_POINT ( 'NONE',  ( -69.97056075661562602, 2.000000000000000000, -7.659292557883846442 ) ) ;
#22235 = AXIS2_PLACEMENT_3D ( 'NONE', #50657, #11488, #46668 ) ;
#22236 = ORIENTED_EDGE ( 'NONE', *, *, #24653, .T. ) ;
#22237 = ORIENTED_EDGE ( 'NONE', *, *, #39489, .F. ) ;
#22238 = CLOSED_SHELL ( 'NONE', ( #4720, #11070, #50560, #11603, #4554, #43545, #14961, #4754, #42672, #3543, #47158, #25743, #1433, #8404, #46671, #9169, #22666, #37325, #14083, #7259, #30764, #51005, #23889, #27562, #14167, #11358, #28979, #22426, #34042, #42458, #14343, #44129, #10014, #11904, #18875, #55667, #11871, #55142, #53594, #30829, #48666, #22698, #52190, #6132, #13568, #29046, #2041, #34746, #6949, #55215, #43275, #15971, #51580, #50626, #50142, #26417, #22128, #14444, #22642, #16129, #38109, #53099, #10012, #3094, #45843, #4358, #2225, #18153, #1284, #52224, #17786, #44345, #53493, #26470, #7359, #22361, #21838, #29918, #39702, #33671, #4310, #23597, #11281, #24256, #14856, #48945, #22593, #56013, #48096, #27063, #2930, #22684, #39054, #54749, #18956, #9780, #55213, #452, #38361, #34555, #1754, #27020, #6047, #40920, #30369, #46958, #36088, #45361, #32159, #40279, #26908, #27249, #15533, #16352, #41162, #21650, #24118, #22016, #33199, #37715, #51150, #34134, #43022, #40561, #47674, #48972, #5582, #40727, #19998, #38317, #33778, #49639, #9067, #21563, #37131, #123, #16179, #9265, #5941, #28906, #30684, #8188, #17447, #3522, #12645, #18392, #4174, #31569, #40261, #17121, #39518, #32708, #42073, #46217, #55318, #2649, #24613, #5636, #5138, #41716, #44214, #13138, #29804, #39707, #11618, #20191, #31833, #16847, #27310, #36410, #20563, #31644, #6903, #18310, #11299, #22584, #17363, #25451, #37853, #36969, #27252, #34265, #6812, #46785, #10604, #50765, #45767, #43687, #10346, #11637, #6093, #29635, #27813, #45350, #31021, #34359, #19516, #11898, #46620, #51100, #27268, #39680, #33771, #37334, #26745, #2688, #34396, #12586, #6565, #38757, #10550, #56214, #54615, #54203, #53185, #17189, #1589, #13582, #8750, #33458, #52522, #108, #36610, #50334, #13791, #9680, #31947, #34125, #31478, #56003, #49560, #15542, #6359, #25049, #19769, #19095, #8912, #46007, #55633, #41024, #8689, #23239, #1357, #30116, #38314, #46373, #16100, #6694, #12333, #13646, #21315, #54180, #3390, #51264, #27454, #5786, #31313, #11028, #4814, #9301, #31372, #9519, #41055, #55922, #32656, #11234, #23113, #24761, #36264, #25282, #41808, #19453, #32063, #7685, #36597, #43347, #19510, #50822, #35508, #15317, #47448, #49305, #12746, #7192, #9017, #28885, #15835, #35105, #17848, #1681, #3003, #11621, #38477, #16358, #3080, #7310, #24916, #49984, #51070, #6311, #52071, #33777, #27931, #22147, #1139, #50463, #31058, #17854, #23585, #51565, #49059, #14571, #8470, #39565, #38329, #40693, #20346, #23305, #48886, #28057, #12843, #51086, #36314, #20586, #38794, #51786, #26562, #55022, #39493, #50730, #30863, #7631, #25726, #40955, #16570, #34383, #14353, #32931, #54095, #31962, #30644, #45331, #28259, #3930, #53116, #47377, #9008, #16048, #2347, #7780, #14537, #32810, #42534, #20463, #16228, #30761, #8499, #54979, #34816, #10345, #42374, #3612, #17280, #34486, #32204, #26807, #44503, #11833, #43152, #30448, #56040, #46361, #19812, #29293, #47178, #27015, #14143, #48514, #23175, #22409, #44193, #17068, #34323, #32975, #54253, #47167, #1354, #49712, #51855, #28562, #48476, #38114, #28951, #45927, #21638, #7409, #26008, #38287, #19948, #33724, #18234, #24274, #27684, #2058, #23125, #13561, #21615, #16277, #13854, #55384, #37675, #28207, #40719, #34554, #34329, #42627, #43372, #10994, #47372, #13907, #5699, #28881, #32753, #34596, #32948, #14864, #13894, #14394, #51172, #33737, #27068, #30614, #34973, #43979, #14969, #51714, #13241, #18380, #6673, #38674, #32061, #9070, #12891, #53790, #47703, #7809, #32850, #22083, #53036, #46231, #7150, #54191, #23453, #54397, #13591, #17708, #16250, #15790, #41956, #37918, #48327, #27800, #15698, #36068, #40599, #25452, #42519, #20482, #9486, #15999, #1082, #19631, #3904, #2781, #6198, #5826, #30797, #44434, #41040, #18356, #32532, #3772, #38283, #30564, #53558, #13939, #23018, #53166, #10904, #49067, #41510, #33473, #896, #44281, #11395, #28719, #44753, #24975, #48404, #44052, #28632, #854, #51711, #35483, #9155, #42833, #8170, #49594, #32463, #4315, #31095, #52049, #36491, #10991, #16288, #7099, #9988, #20687, #29811, #3489, #3383, #42763, #15347, #18777, #20844, #48141, #20781, #25088, #32744, #22759, #6350, #32339, #44371, #31743, #20599, #26674, #33925, #43414, #12334, #48773, #51734, #1848, #4558, #9686, #24075, #38043, #51396, #49881, #4405, #22980, #36875, #46998, #24372, #40439, #5043, #17726, #45388, #20983, #29142, #26874, #48254, #35968, #3857, #47183, #37118, #54433, #40750, #16933, #28108, #15164, #17310, #45161, #45745, #53983, #54392, #36535, #20605, #25220, #4056, #30343, #2341, #35498, #6485, #1750, #22892, #31370, #17702, #25419, #24376, #48345, #37639, #55747, #54857, #14558, #39302, #41893, #26232, #49896, #46478, #12406, #46469, #5568, #52838, #41730, #33077, #38569, #51965, #55711, #51753, #34445, #27096, #6542, #19890, #47482, #48015, #42513, #30519, #31216, #9898, #32958, #22794, #1975, #37840, #39177, #52062, #8245, #17710, #25344, #43591, #47516, #50567, #28332, #22585, #45997, #36889, #53235, #19592, #50045, #11578, #18629, #6161, #32855, #44947, #42540, #3126, #26002, #14424, #35530, #28924, #32496, #42699, #33478, #31985, #2170, #49363, #8112, #25621, #27654, #12358, #50975, #29504, #34060, #50549, #50192, #18940, #50146, #631, #3892, #55588, #55984, #37254, #23428, #12817, #55453, #13545, #31719, #21485, #43434, #46404, #52745, #10193, #23345, #487, #5301, #24605, #44986, #24953, #9536, #9234, #7064, #21288, #7660, #24126, #15444, #34294, #48602, #33663, #955, #28715, #40562, #35175, #814, #48637, #13917, #25219, #55985, #4321, #47478, #13997, #39723, #44426, #53619, #21093, #5009, #28556, #24812, #40681, #33414, #27699, #53303, #6486, #195, #41930, #18222, #8493, #18810, #36168, #43422, #32714, #29073, #32012, #15283, #16913, #27203, #45084, #48643, #54182, #48751, #26469, #39724, #30187, #32468, #21857, #1397, #54557, #48852, #15986, #33319, #41093, #3351, #13457, #38930, #29377, #38469, #856, #44181, #28328, #36115, #35583, #29808, #13327, #25257, #14214, #55822, #19431, #20388, #22432, #18827, #10473, #15230, #39010, #50843, #2655, #11812, #32782, #15570, #48349, #37073, #3211, #52702, #49093, #41424, #31812, #51137, #12191, #10916, #44766, #52885, #53547, #28003, #15606, #34702, #19562, #11141, #54907, #13689, #776, #52879, #1508, #11218, #8981, #30919, #1138, #24407, #38137, #6757, #34924, #32687, #47594, #45702, #37562, #50102, #25382, #50466, #5126, #8661, #36909, #45153, #39524, #29725, #10689, #28134, #17877, #40820, #29327, #47871, #48201, #52530, #5342, #21304, #7036, #25724, #43159, #6226, #34385, #52746, #6586, #33555, #4824, #54710, #50144, #37458, #5315, #33385, #15831, #15652, #5738, #14331, #21977, #28981, #24189, #14057, #24620, #9350, #18401, #8975, #40141, #54578, #7712, #41776, #7247, #16170, #13306, #46903, #4340, #53189, #35211, #6253, #221, #49817, #21988, #36414, #53000, #16973, #41705, #54877, #51193, #28623, #8033, #24122, #31875, #43655, #42771, #27264, #38939, #14392, #5933, #4229, #4503, #56070, #50221, #16488, #3352, #8544, #55629, #44474, #5222, #49607, #7312, #28819, #47664, #26402, #56152, #35975, #39072, #3534, #26365, #51233, #16061, #35282, #42798, #14273, #17031, #13256, #22291, #9186, #36827, #28703, #42929, #34367, #4621, #19871, #44869, #56231, #7421, #20510, #49110, #12331, #10571, #53590, #21679, #35699, #19704, #7644, #32846, #15382, #1168, #12767, #19885, #1332, #3419, #2967, #31006, #40069, #47905, #20614, #49928, #51495, #13093, #6418, #382, #35844, #31020, #51844, #7131, #42574, #54954, #17918, #4420, #33358, #43203, #32892, #4010, #6889, #47139, #11796, #18273, #13539, #9769, #11503, #11859, #32089, #6388, #20581, #43936, #49653, #13651, #9499, #10933, #41277, #47536, #4583, #15395, #13541, #47716, #28531, #36257, #4710, #45258, #48242, #17525, #43037, #49660, #52961, #28450, #5491, #7198, #50887, #6629, #48735, #26983, #19884, #22407, #5599, #1245, #50228, #2177, #38153, #16397, #9233, #26323, #6016, #52454, #32153, #6057, #5054, #17797, #30159, #10684, #29902, #4413, #2663, #30491, #28598, #43031, #4965, #43660, #43520, #27558, #7798, #46160, #36723, #40725, #52696, #42134, #46613, #35383, #178, #15724, #14478, #16696, #25542, #5834, #40659, #44785, #35733, #32885, #15090, #18840, #4612, #32464, #41495, #6446, #46222, #23650, #54472, #17530, #28271, #23010, #9826, #32092, #38890, #17006, #6243, #40084, #43109, #44410, #36211, #50623, #43467, #1315, #49555, #36370, #46542, #25583, #47005, #29041, #35361, #2562, #39796, #11020, #38989, #51111, #3045, #54817, #54808, #32096, #49641, #37527, #2549, #15397, #44733, #35941, #47506, #47324, #19022, #31469, #43804, #23962, #35820, #41382, #18465, #19861, #28676, #45103, #56220, #53245, #7501, #27400, #25849, #32163, #46098, #5930, #23098, #10537, #31450, #46353, #1836, #40216, #37750, #51585, #31138, #603, #31016, #24679, #55500, #15038, #42349, #39941, #43095, #33806, #38542, #6347, #45747, #36047, #48607, #75, #53653, #49647, #7767, #1542, #27579, #35802, #55148, #15016, #53414, #52455, #50071, #5462, #41448, #30914, #13172, #24193, #37495, #42994, #36298, #33360, #35860, #48765, #9389, #33499, #24623, #27935, #36840, #26428, #32739, #14619, #30102, #35319, #12236, #31236, #45664, #10101, #4417, #7573, #16809, #14684, #40029, #10856, #60, #1738, #453, #15229, #19946, #4686, #44543, #30046, #16104, #43165, #29317, #10921, #11775, #9804, #12507, #12570, #46267, #17253, #42810, #45602, #13602, #5140, #7158, #32021, #36637, #34126, #33029, #1999, #8115, #17443, #51383, #6269, #1211, #20592, #56117, #43092, #40206, #50785, #47226, #44882, #25315, #29151, #7762, #48021, #23539, #52992, #10740, #16338, #10788, #6195, #14039, #3751, #25160, #43874, #22330, #5310, #10841, #40792, #14585, #19443, #12833, #8414, #19017, #1724, #50234, #24011, #26115, #53608, #4098, #1215, #32653, #12134, #23486, #48740, #31679, #16887, #28093, #13128, #16227, #1021, #29443, #19326, #30212, #54109, #35893, #604, #54456, #46043, #40392, #26766, #18964, #26158, #40653, #43790, #20721, #22862, #14560, #22804, #33983, #35241, #27880, #4912, #55881, #34514, #15796, #17867, #46587, #47786, #18614, #52567, #29500, #18126, #6518, #2390, #49063, #12580, #51988, #36129, #23508, #12959, #53172, #36553, #10457, #47254, #40403, #30204, #39959, #34613, #31324, #9271, #54589, #25112, #21690, #6888, #35621, #36076, #28255, #32595, #34751, #25336, #53420, #830, #38982, #35964, #50707, #22164, #45874, #20435, #200, #28629, #39069, #22546, #33711, #1976, #38752, #21777, #22436, #44780, #54296, #12628, #2118, #16348, #52825, #50117, #51487, #32243, #37425, #34222, #20911, #20132, #24594, #45381, #35089, #37963, #37930, #49045, #34901, #24437, #55523, #17578, #38367, #35115, #5273, #45982, #33089, #48079, #50752, #44211, #9582, #1351, #2471, #17348, #41969, #19254, #14340, #48926, #44566, #28142, #34461, #17325, #3907, #4895, #50847, #39048, #5095, #52508, #14609, #42221, #55740, #37302, #25653, #40962, #55827, #3936, #39831, #13644, #23384, #37627, #48115, #25031, #53340, #20394, #37983, #33124, #19094, #31869, #1832, #15785, #26421, #18763, #41583, #53910, #42630, #25781, #10030, #47124, #53530, #50067, #33970, #39267, #13369, #32942, #15876, #20627, #44629, #42116, #5642, #18301, #44425, #13600, #51156, #53389, #29523, #43983, #11997, #24215, #22337, #48101, #829, #8846, #11497, #18555, #31912, #26926, #9644, #54132, #34674, #13431, #38493, #18272, #52693, #6257, #40688, #1127, #20052, #1560, #8806, #18451, #12320, #43410, #8503, #24064, #48935, #25087, #15469, #21784, #24314, #29825, #10616, #2528, #27383, #2952, #28620, #8273, #27423, #29612, #54103, #42745, #9164, #10433, #34709, #51101, #54671, #50012, #7702, #15770, #5217, #17081, #27696, #55341, #6433, #1027, #49702, #27916, #55869, #50676, #39952, #49756, #35537, #38777, #23307, #17092, #32531, #8586, #38082, #26253, #51501, #50921, #12108, #21553, #55408, #16842, #31010, #43810, #13816, #14896, #56051, #50410, #27146, #23487, #47291, #55201, #50952, #24004, #29897, #37490, #28223, #52038, #48044, #47297, #19479, #45634, #52664, #22989, #15513, #14753, #36494, #8452, #47857, #55749, #42646, #4001, #2220, #22213, #2725, #28462, #37640, #20326, #50052, #39230, #24432, #12975, #23712, #21182, #4128, #15989, #3866, #47645, #46459, #17418, #35230, #33856, #51234, #2660, #55320, #12660, #41325, #48269, #42967, #38881, #6728, #28939, #40334, #48146, #34634, #6302, #51309, #10772, #24836, #27500, #14419, #25029, #43548, #38263, #38928, #50312, #44646, #794, #15115, #12643, #859, #53399, #24511, #37952, #55270, #6411, #14056, #33474, #47608, #25971, #43262, #11648, #29006, #10486, #23811, #26697, #36204, #55640, #23023, #15560, #9523, #16333, #15260, #53660, #8679, #32399, #32527, #40981, #5364, #20879, #8815, #1419, #12181, #48260, #4889, #7572, #4509, #16923, #30854, #22531, #24509, #42737, #18867, #17085, #14179, #23042, #40632, #30819, #55417, #16886, #35517, #4943, #9693, #42715, #52344, #43155, #1565, #6449, #23094, #13786, #39229, #665, #24691, #35577, #50558, #21511, #55257, #33765, #24729, #37498, #28516, #4352, #45517, #26890, #3466, #43517, #28748, #43202, #8699, #54421, #16483, #6428, #14581, #32338, #41630, #23024, #17426, #34848, #20681, #21779, #39597, #37128, #36336, #6512, #14202, #10645, #12808, #23211, #27119, #39007, #39859, #36404, #6525, #55786, #13673, #20948, #35882, #39142, #54480, #18136, #11784, #22924, #13792, #40484, #30078, #412, #18714, #18686, #3239, #45639, #55932, #7224, #32003, #25799, #2929, #37178, #22400, #23675, #19251, #4431, #10095, #29994, #3834, #48552, #26841, #25814, #14081, #14043, #35799, #9118, #31615, #51046, #8781, #11129, #53394, #2796, #41431, #53939, #29517, #50533, #53956, #48822, #41854, #17374, #33415, #10181, #3588, #55313, #41914, #43458, #5163, #21819, #28393, #37203, #37120, #36759, #25407, #39378, #30487, #49265, #7130, #43708, #22833, #4780, #44217, #38618, #22798, #52199, #39792, #41107, #18655, #31710, #19027, #20527, #13552, #46011, #21689, #32273, #25810, #42890, #11564, #6480, #21370, #40620, #15765, #36686, #1910, #20177, #26477, #20021, #32697, #14655, #49000, #48590, #15110, #40557, #22917, #8431, #9799, #30754, #50456, #12008, #5040, #27202, #53894, #34898, #36308, #53199, #19822, #36126, #5831, #29895, #30543, #25446, #45042, #17272, #19377, #47824, #21062, #32405, #28399, #53466, #12354, #39190, #3939, #8085, #30668, #41420, #12085, #36243, #19824, #5431, #48196, #56181, #6767, #17486, #40405, #49107, #41976, #4640, #27207, #6287, #36119, #1672, #19107, #43005, #52585, #11217, #26341, #22277, #49976, #28440, #34507, #16096, #13550, #742, #43592, #55626, #11313, #5868, #19366, #56144, #51663, #32209, #53606, #54302, #7731, #10863, #34659, #14623, #26332, #15195, #42231, #16191, #19220, #8615, #48677, #23377, #32450, #25187, #55227, #23364, #43192, #43268, #50714, #54631, #6760, #50538, #13285, #8279, #8541, #27575, #15531, #31938, #41316, #54699, #12530, #10436, #48752, #28166, #8886, #34434, #8708, #23699, #26024, #19506, #30007, #33374, #2273, #6741, #43621, #21516, #23373, #54947, #44992, #48354, #7032, #16384, #15407, #19497, #29973, #2585, #19330, #25534, #19928, #30749, #53722, #24302, #50452, #34823, #51019, #31689, #51646, #22127, #53900, #10315, #13228, #23978, #33299, #14058, #1730, #34763, #18943, #48698, #7235, #20136, #41330, #55413, #42001, #15224, #16807, #45569, #17096, #50593, #24322, #34511, #28302, #51559, #17510, #17254, #54941, #19292, #43424, #32227, #16415, #6061, #22874, #14265, #53836, #27134, #3594, #49009, #45104, #2460, #36651, #23907, #2354, #7971, #2097, #18297, #39894, #11558, #49324, #18416, #11817, #5006, #2576, #7446, #9649, #1695, #51431, #16197, #3009, #28675, #6166, #18393, #23048, #32893, #38514, #55559, #9920, #47004, #20104, #35184, #26486, #17217, #41974, #3781, #20227, #21323, #50767, #15930, #49752, #8772, #21022, #19224, #35939, #51368, #20650, #20267, #597, #36539, #5664, #11900, #26174, #45139, #1971, #49722, #51238, #44764, #8347, #55052, #47604, #17811, #47366, #24883, #53477, #14173, #14626, #35789, #2875, #30798, #52293, #45272, #29655, #21684, #12664, #926, #43918, #42680, #33240, #24260, #47196, #42101, #39382, #26565, #31574, #38122, #24333, #50399, #2159, #3746, #30557, #50609, #47678, #32839, #2807, #47003, #16998, #52759, #45303, #35515, #27161, #50829, #47793, #790 ) ) ;
#22239 = FACE_OUTER_BOUND ( 'NONE', #25635, .T. ) ;
#22240 = CARTESIAN_POINT ( 'NONE',  ( -18.62826334475414924, 0.000000000000000000, 9.685474233794316490 ) ) ;
#22241 = DIRECTION ( 'NONE',  ( 0.000000000000000000, -0.000000000000000000, -1.000000000000000000 ) ) ;
#22242 = AXIS2_PLACEMENT_3D ( 'NONE', #37936, #46421, #54206 ) ;
#22243 = DIRECTION ( 'NONE',  ( -0.005961354470445682716, -0.6427876096865404731, 0.7660212471507180654 ) ) ;
#22244 = CARTESIAN_POINT ( 'NONE',  ( -21.27557641678912148, -4.241740624735661491, 11.90750714001334920 ) ) ;
#22245 = DIRECTION ( 'NONE',  ( 0.000000000000000000, -0.000000000000000000, -1.000000000000000000 ) ) ;
#22246 = EDGE_CURVE ( 'NONE', #51326, #40968, #54337, .T. ) ;
#22247 = VECTOR ( 'NONE', #51875, 999.9999999999998863 ) ;
#22248 = ORIENTED_EDGE ( 'NONE', *, *, #27155, .T. ) ;
#22249 = DIRECTION ( 'NONE',  ( -0.5449076811759708816, 0.6444004775717707689, 0.5364919789714475140 ) ) ;
#22250 = DIRECTION ( 'NONE',  ( 0.007781995580012662783, 0.000000000000000000, -0.9999697198139514409 ) ) ;
#22251 = VECTOR ( 'NONE', #33463, 1000.000000000000000 ) ;
#22253 = ORIENTED_EDGE ( 'NONE', *, *, #51364, .F. ) ;
#22252 = VECTOR ( 'NONE', #24766, 1000.000000000000227 ) ;
#22254 = VECTOR ( 'NONE', #17174, 1000.000000000000114 ) ;
#22255 = CARTESIAN_POINT ( 'NONE',  ( -24.53375310857961367, 18.49370688441070953, 4.657440554554202805 ) ) ;
#22256 = DIRECTION ( 'NONE',  ( -0.9999697198139514409, -0.000000000000000000, -0.007781995580013368816 ) ) ;
#22257 = DIRECTION ( 'NONE',  ( -0.5449076811759708816, 0.6444004775717707689, 0.5364919789714475140 ) ) ;
#22258 = VECTOR ( 'NONE', #28288, 1000.000000000000227 ) ;
#22259 = EDGE_CURVE ( 'NONE', #53756, #26056, #45524, .T. ) ;
#22260 = EDGE_LOOP ( 'NONE', ( #44134, #37014, #25577, #28000 ) ) ;
#22261 = VECTOR ( 'NONE', #25332, 1000.000000000000227 ) ;
#22262 = DIRECTION ( 'NONE',  ( 0.7660212471507180654, -0.6427876096865404731, 0.005961354470445141482 ) ) ;
#22263 = EDGE_LOOP ( 'NONE', ( #30134, #24742, #12621, #4316 ) ) ;
#22264 = EDGE_CURVE ( 'NONE', #7467, #5490, #46097, .T. ) ;
#22265 = B_SPLINE_CURVE_WITH_KNOTS ( 'NONE', 3,
 ( #10533, #27856, #36636, #2259, #53948, #27263 ),
 .UNSPECIFIED., .F., .F.,
 ( 4, 2, 4 ),
 ( 0.000000000000000000, 0.0002007373455692541874, 0.0004014746911385083748 ),
 .UNSPECIFIED. ) ;
#22266 = EDGE_CURVE ( 'NONE', #47757, #3399, #20244, .T. ) ;
#22267 = VECTOR ( 'NONE', #39781, 999.9999999999998863 ) ;
#22268 = ORIENTED_EDGE ( 'NONE', *, *, #23221, .T. ) ;
#22269 = VECTOR ( 'NONE', #9997, 999.9999999999998863 ) ;
#22270 = ORIENTED_EDGE ( 'NONE', *, *, #52180, .F. ) ;
#22271 = ORIENTED_EDGE ( 'NONE', *, *, #41610, .F. ) ;
#22272 = CARTESIAN_POINT ( 'NONE',  ( -23.33849165029409889, 0.000000000000000000, 5.946783852668351855 ) ) ;
#22273 = ORIENTED_EDGE ( 'NONE', *, *, #51327, .F. ) ;
#22274 = DIRECTION ( 'NONE',  ( 0.9999697198139515519, 0.000000000000000000, 0.007781995580013368816 ) ) ;
#22275 = VERTEX_POINT ( 'NONE', #41822 ) ;
#22276 = LINE ( 'NONE', #35601, #21390 ) ;
#22277 = ADVANCED_FACE ( 'NONE', ( #36754 ), #53770, .F. ) ;
#22278 = ORIENTED_EDGE ( 'NONE', *, *, #55662, .T. ) ;
#22279 = DIRECTION ( 'NONE',  ( -0.7660212471507179544, -0.6427876096865405842, -0.005961354470445141482 ) ) ;
#22280 = ORIENTED_EDGE ( 'NONE', *, *, #40716, .T. ) ;
#22281 = EDGE_CURVE ( 'NONE', #9065, #44931, #14889, .T. ) ;
#22282 = AXIS2_PLACEMENT_3D ( 'NONE', #21620, #8256, #56236 ) ;
#22283 = LINE ( 'NONE', #44983, #34759 ) ;
#22284 = VECTOR ( 'NONE', #46400, 1000.000000000000114 ) ;
#22285 = LINE ( 'NONE', #10045, #25954 ) ;
#22286 = LINE ( 'NONE', #26252, #5033 ) ;
#22287 = DIRECTION ( 'NONE',  ( -0.1139275668495183524, 0.9934890585767659488, 4.694855797473114533E-16 ) ) ;
#22288 = CARTESIAN_POINT ( 'NONE',  ( -12.50255982302408775, -4.403642575758163424, 1.597240687396138892 ) ) ;
#22289 = VECTOR ( 'NONE', #33340, 999.9999999999998863 ) ;
#22290 = ORIENTED_EDGE ( 'NONE', *, *, #45867, .F. ) ;
#22291 = ADVANCED_FACE ( 'NONE', ( #37579 ), #54903, .F. ) ;
#22292 = EDGE_LOOP ( 'NONE', ( #44527, #40171, #38813, #43651 ) ) ;
#22293 = CARTESIAN_POINT ( 'NONE',  ( -19.59569683186026268, 0.000000000000000000, 14.58168106541950948 ) ) ;
#22294 = FACE_OUTER_BOUND ( 'NONE', #51463, .T. ) ;
#22295 = AXIS2_PLACEMENT_3D ( 'NONE', #40080, #26455, #13680 ) ;
#22296 = LINE ( 'NONE', #31070, #14293 ) ;
#22297 = EDGE_CURVE ( 'NONE', #19093, #33398, #19969, .T. ) ;
#22298 = VECTOR ( 'NONE', #55161, 1000.000000000000227 ) ;
#22299 = VECTOR ( 'NONE', #52067, 999.9999999999998863 ) ;
#22300 = DIRECTION ( 'NONE',  ( -0.2426528472758542054, 0.7422098413412800966, -0.6246952433987894571 ) ) ;
#22301 = LINE ( 'NONE', #17759, #8605 ) ;
#22302 = CARTESIAN_POINT ( 'NONE',  ( -70.03639332226748593, -0.2499667854710889425, -7.502502568033361463 ) ) ;
#22303 = ORIENTED_EDGE ( 'NONE', *, *, #41088, .F. ) ;
#22304 = DIRECTION ( 'NONE',  ( 0.9999697198139515519, 0.000000000000000000, 0.007781995580013368816 ) ) ;
#22305 = DIRECTION ( 'NONE',  ( 1.000000000000000000, 0.000000000000000000, 0.000000000000000000 ) ) ;
#22306 = ORIENTED_EDGE ( 'NONE', *, *, #34753, .F. ) ;
#22307 = AXIS2_PLACEMENT_3D ( 'NONE', #44424, #124, #52406 ) ;
#22308 = CARTESIAN_POINT ( 'NONE',  ( -66.62919651559374756, -8.730421935648388754, 1.346828299457899725 ) ) ;
#22309 = LINE ( 'NONE', #17462, #17881 ) ;
#22310 = AXIS2_PLACEMENT_3D ( 'NONE', #22120, #39454, #39739 ) ;
#22311 = VECTOR ( 'NONE', #22658, 1000.000000000000000 ) ;
#22312 = DIRECTION ( 'NONE',  ( -0.005002170337468016433, -0.7660444431189770143, 0.6427681459581293666 ) ) ;
#22313 = PLANE ( 'NONE',  #51329 ) ;
#22314 = VECTOR ( 'NONE', #32252, 1000.000000000000000 ) ;
#22315 = CARTESIAN_POINT ( 'NONE',  ( -14.20280369269832832, 0.000000000000000000, 12.40765738797303719 ) ) ;
#22316 = ORIENTED_EDGE ( 'NONE', *, *, #29521, .F. ) ;
#22317 = VECTOR ( 'NONE', #37943, 1000.000000000000000 ) ;
#22318 = ORIENTED_EDGE ( 'NONE', *, *, #15337, .T. ) ;
#22319 = CARTESIAN_POINT ( 'NONE',  ( -20.54204810873173415, 0.000000000000000000, 4.860550213503115558 ) ) ;
#22320 = PLANE ( 'NONE',  #43985 ) ;
#22321 = FACE_OUTER_BOUND ( 'NONE', #23029, .T. ) ;
#22322 = CARTESIAN_POINT ( 'NONE',  ( -20.54049170961573267, 0.000000000000000000, 4.660556269540326646 ) ) ;
#22323 = FACE_OUTER_BOUND ( 'NONE', #53006, .T. ) ;
#22324 = EDGE_CURVE ( 'NONE', #53756, #51780, #41288, .T. ) ;
#22325 = CARTESIAN_POINT ( 'NONE',  ( -18.67619601524082285, 0.000000000000000000, 3.936400510096834893 ) ) ;
#22326 = LINE ( 'NONE', #51833, #45623 ) ;
#22327 = VECTOR ( 'NONE', #10378, 1000.000000000000227 ) ;
#22328 = CARTESIAN_POINT ( 'NONE',  ( -22.36868959911851462, 19.74370688441071309, -4.657437592157546824 ) ) ;
#22329 = DIRECTION ( 'NONE',  ( 0.005002170337468016433, -0.7660444431189770143, -0.6427681459581293666 ) ) ;
#22330 = ADVANCED_FACE ( 'NONE', ( #32218 ), #49541, .F. ) ;
#22331 = ORIENTED_EDGE ( 'NONE', *, *, #48838, .F. ) ;
#22332 = DIRECTION ( 'NONE',  ( -0.7660212471507179544, -0.6427876096865405842, -0.005961354470445141482 ) ) ;
#22333 = ORIENTED_EDGE ( 'NONE', *, *, #54005, .T. ) ;
#22334 = CARTESIAN_POINT ( 'NONE',  ( -21.06965149344186372, 20.49370688441071664, -4.356725136697556344 ) ) ;
#22335 = VECTOR ( 'NONE', #1803, 999.9999999999998863 ) ;
#22336 = EDGE_CURVE ( 'NONE', #17295, #47436, #28497, .T. ) ;
#22337 = ADVANCED_FACE ( 'NONE', ( #40995 ), #55966, .F. ) ;
#22338 = DIRECTION ( 'NONE',  ( 0.9999697198139515519, 0.000000000000000000, 0.007781995580013368816 ) ) ;
#22339 = EDGE_CURVE ( 'NONE', #34418, #47950, #56224, .T. ) ;
#22340 = ORIENTED_EDGE ( 'NONE', *, *, #6360, .F. ) ;
#22341 = FACE_OUTER_BOUND ( 'NONE', #27805, .T. ) ;
#22342 = VECTOR ( 'NONE', #37423, 1000.000000000000000 ) ;
#22343 = ORIENTED_EDGE ( 'NONE', *, *, #7920, .T. ) ;
#22344 = EDGE_CURVE ( 'NONE', #37937, #10254, #12786, .T. ) ;
#22345 = EDGE_LOOP ( 'NONE', ( #42143, #28746, #49189, #9420 ) ) ;
#22346 = AXIS2_PLACEMENT_3D ( 'NONE', #19267, #28080, #36603 ) ;
#22347 = ORIENTED_EDGE ( 'NONE', *, *, #48544, .T. ) ;
#22348 = VECTOR ( 'NONE', #33021, 1000.000000000000227 ) ;
#22349 = VERTEX_POINT ( 'NONE', #52263 ) ;
#22350 = ORIENTED_EDGE ( 'NONE', *, *, #56233, .T. ) ;
#22351 = CARTESIAN_POINT ( 'NONE',  ( -12.42791540084058255, 3.524445264749011208, 1.396907870518687256 ) ) ;
#22352 = LINE ( 'NONE', #55859, #3142 ) ;
#22353 = CIRCLE ( 'NONE', #29605, 0.5000000000000004441 ) ;
#22354 = VECTOR ( 'NONE', #51480, 1000.000000000000114 ) ;
#22355 = ORIENTED_EDGE ( 'NONE', *, *, #7998, .T. ) ;
#22356 = DIRECTION ( 'NONE',  ( -0.000000000000000000, -0.000000000000000000, 1.000000000000000000 ) ) ;
#22357 = EDGE_CURVE ( 'NONE', #30292, #11776, #3985, .T. ) ;
#22358 = EDGE_LOOP ( 'NONE', ( #52762, #37360, #3031, #13052 ) ) ;
#22359 = EDGE_LOOP ( 'NONE', ( #26409, #45308, #34064, #21793 ) ) ;
#22360 = AXIS2_PLACEMENT_3D ( 'NONE', #20196, #16505, #33551 ) ;
#22361 = ADVANCED_FACE ( 'NONE', ( #26395 ), #43450, .F. ) ;
#22362 = AXIS2_PLACEMENT_3D ( 'NONE', #56044, #17137, #51757 ) ;
#22363 = FACE_OUTER_BOUND ( 'NONE', #39708, .T. ) ;
#22364 = FACE_OUTER_BOUND ( 'NONE', #52138, .T. ) ;
#22365 = EDGE_CURVE ( 'NONE', #12432, #50295, #5131, .T. ) ;
#22366 = DIRECTION ( 'NONE',  ( -0.7660212471507179544, -0.6427876096865405842, -0.005961354470445141482 ) ) ;
#22367 = ORIENTED_EDGE ( 'NONE', *, *, #28403, .T. ) ;
#22368 = CARTESIAN_POINT ( 'NONE',  ( -17.74482636761137044, -0.1191753592594197858, 3.674319602356483916 ) ) ;
#22369 = ORIENTED_EDGE ( 'NONE', *, *, #47036, .T. ) ;
#22370 = EDGE_CURVE ( 'NONE', #9163, #43762, #4827, .T. ) ;
#22371 = CARTESIAN_POINT ( 'NONE',  ( -16.49482643775764146, 0.000000000000000000, 8.385361270221707741 ) ) ;
#22372 = VECTOR ( 'NONE', #3525, 1000.000000000000114 ) ;
#22373 = FACE_OUTER_BOUND ( 'NONE', #16193, .T. ) ;
#22374 = LINE ( 'NONE', #1029, #37688 ) ;
#22375 = LINE ( 'NONE', #1030, #25818 ) ;
#22376 = CARTESIAN_POINT ( 'NONE',  ( 5.284380629179495692, -1.088761635349915657, -2.393572233197383881 ) ) ;
#22377 = CARTESIAN_POINT ( 'NONE',  ( -18.67775241435682432, 0.000000000000000000, 4.136394454059623804 ) ) ;
#22378 = DIRECTION ( 'NONE',  ( 0.005002170337468016433, -0.7660444431189770143, -0.6427681459581293666 ) ) ;
#22379 = ORIENTED_EDGE ( 'NONE', *, *, #52558, .T. ) ;
#22380 = CARTESIAN_POINT ( 'NONE',  ( -16.06709938707323460, 0.000000000000000000, 13.13181314741652628 ) ) ;
#22381 = PRODUCT ( 'Curved Precision Cutting Blades', 'Curved Precision Cutting Blades', '', ( #3637 ) ) ;
#22382 = AXIS2_PLACEMENT_3D ( 'NONE', #51960, #6245, #44555 ) ;
#22383 = FACE_OUTER_BOUND ( 'NONE', #51020, .T. ) ;
#22384 = PLANE ( 'NONE',  #42311 ) ;
#22386 = DIRECTION ( 'NONE',  ( 0.005961354470445682716, -0.6427876096865404731, -0.7660212471507180654 ) ) ;
#22385 = AXIS2_PLACEMENT_3D ( 'NONE', #4376, #4919, #21687 ) ;
#22387 = CARTESIAN_POINT ( 'NONE',  ( -15.88066920543382921, 21.75751639764346024, -4.011138004292909898 ) ) ;
#22388 = DIRECTION ( 'NONE',  ( 0.007781995580012663651, -3.146120232559066537E-19, -0.9999697198139514409 ) ) ;
#22389 = CARTESIAN_POINT ( 'NONE',  ( -20.34342856960166657, -4.241740624735661491, 11.54542926029160377 ) ) ;
#22390 = AXIS2_PLACEMENT_3D ( 'NONE', #51350, #7078, #55893 ) ;
#22391 = DIRECTION ( 'NONE',  ( 0.007781995580012663651, -3.146120232559066537E-19, -0.9999697198139514409 ) ) ;
#22392 = VERTEX_POINT ( 'NONE', #4293 ) ;
#22393 = DIRECTION ( 'NONE',  ( -0.8531650599175529814, -0.4028455766673920135, 0.3313982828793697877 ) ) ;
#22394 = DIRECTION ( 'NONE',  ( 0.6427681459581294776, -0.7660444431189769032, 0.005002170337467562802 ) ) ;
#22395 = FACE_OUTER_BOUND ( 'NONE', #46453, .T. ) ;
#22396 = EDGE_CURVE ( 'NONE', #4104, #46046, #17313, .T. ) ;
#22397 = VECTOR ( 'NONE', #7910, 999.9999999999998863 ) ;
#22398 = CARTESIAN_POINT ( 'NONE',  ( -9.075990533167328067, 0.000000000000000000, 10.41622904950343909 ) ) ;
#22399 = CARTESIAN_POINT ( 'NONE',  ( -14.41329247838824124, 0.000000000000000000, 5.446903690347632221 ) ) ;
#22400 = ADVANCED_FACE ( 'NONE', ( #17909 ), #22149, .F. ) ;
#22401 = DIRECTION ( 'NONE',  ( -0.000000000000000000, -1.000000000000000000, -0.000000000000000000 ) ) ;
#22402 = CARTESIAN_POINT ( 'NONE',  ( -14.62921308899344730, 0.000000000000000000, 7.491889751483238769 ) ) ;
#22403 = VECTOR ( 'NONE', #29220, 1000.000000000000227 ) ;
#22404 = VECTOR ( 'NONE', #19072, 1000.000000000000227 ) ;
#22405 = LINE ( 'NONE', #30351, #4343 ) ;
#22406 = CARTESIAN_POINT ( 'NONE',  ( -12.23010465924184764, -4.079838673713163111, 1.501740888941589303 ) ) ;
#22407 = ADVANCED_FACE ( 'NONE', ( #47421 ), #48246, .F. ) ;
#22408 = EDGE_CURVE ( 'NONE', #32474, #13470, #31227, .T. ) ;
#22409 = ADVANCED_FACE ( 'NONE', ( #13072 ), #30400, .F. ) ;
#22410 = ORIENTED_EDGE ( 'NONE', *, *, #11737, .T. ) ;
#22411 = EDGE_CURVE ( 'NONE', #37913, #34403, #8530, .T. ) ;
#22412 = AXIS2_PLACEMENT_3D ( 'NONE', #31571, #48029, #52835 ) ;
#22413 = ORIENTED_EDGE ( 'NONE', *, *, #32629, .F. ) ;
#22414 = VERTEX_POINT ( 'NONE', #8838 ) ;
#22415 = VERTEX_POINT ( 'NONE', #38919 ) ;
#22416 = ORIENTED_EDGE ( 'NONE', *, *, #38336, .F. ) ;
#22417 = FACE_OUTER_BOUND ( 'NONE', #24272, .T. ) ;
#22418 = DIRECTION ( 'NONE',  ( 0.000000000000000000, -0.000000000000000000, -1.000000000000000000 ) ) ;
#22419 = ORIENTED_EDGE ( 'NONE', *, *, #56180, .F. ) ;
#22420 = AXIS2_PLACEMENT_3D ( 'NONE', #42141, #11196, #20577 ) ;
#22421 = ORIENTED_EDGE ( 'NONE', *, *, #43336, .F. ) ;
#22422 = EDGE_CURVE ( 'NONE', #39021, #49471, #26142, .T. ) ;
#22423 = AXIS2_PLACEMENT_3D ( 'NONE', #23677, #22846, #39891 ) ;
#22424 = CARTESIAN_POINT ( 'NONE',  ( -19.25813676402126617, -5.698858183938163791, 13.51524322189348659 ) ) ;
#22425 = ORIENTED_EDGE ( 'NONE', *, *, #39586, .T. ) ;
#22426 = ADVANCED_FACE ( 'NONE', ( #39179 ), #39761, .F. ) ;
#22427 = CARTESIAN_POINT ( 'NONE',  ( -16.45426279964252458, 0.000000000000000000, 3.173020884834126587 ) ) ;
#22428 = DIRECTION ( 'NONE',  ( 0.7660212471507180654, -0.6427876096865404731, 0.005961354470445141482 ) ) ;
#22429 = ORIENTED_EDGE ( 'NONE', *, *, #20430, .F. ) ;
#22430 = PLANE ( 'NONE',  #31009 ) ;
#22431 = EDGE_LOOP ( 'NONE', ( #30912, #42795, #39124, #36013, #33556, #12280, #2198, #1569 ) ) ;
#22432 = ADVANCED_FACE ( 'NONE', ( #35484 ), #52791, .F. ) ;
#22433 = VECTOR ( 'NONE', #49231, 1000.000000000000227 ) ;
#22434 = CARTESIAN_POINT ( 'NONE',  ( -15.62813556599864562, 0.000000000000000000, 2.852125011887896910 ) ) ;
#22435 = DIRECTION ( 'NONE',  ( 0.005002170337468016433, -0.7660444431189770143, -0.6427681459581293666 ) ) ;
#22436 = ADVANCED_FACE ( 'NONE', ( #23549 ), #40609, .F. ) ;
#22437 = FACE_OUTER_BOUND ( 'NONE', #7951, .T. ) ;
#22438 = CARTESIAN_POINT ( 'NONE',  ( -19.12492725574397312, -0.04999193034575387384, 8.406842698057740648 ) ) ;
#22439 = EDGE_LOOP ( 'NONE', ( #29508, #53309, #19463, #43959 ) ) ;
#22440 = CARTESIAN_POINT ( 'NONE',  ( -22.40478740399063895, 0.000000000000000000, 5.384712028983816623 ) ) ;
#22441 = LINE ( 'NONE', #26972, #11144 ) ;
#22442 = CARTESIAN_POINT ( 'NONE',  ( -17.46532115785441519, 0.000000000000000000, 13.67492996699914265 ) ) ;
#22443 = ORIENTED_EDGE ( 'NONE', *, *, #52407, .T. ) ;
#22444 = CARTESIAN_POINT ( 'NONE',  ( -25.20123094555300369, 0.000000000000000000, 6.470945668149052032 ) ) ;
#22445 = ORIENTED_EDGE ( 'NONE', *, *, #52527, .T. ) ;
#22446 = CARTESIAN_POINT ( 'NONE',  ( -28.92982233430281980, 0.000000000000000000, 7.919257187036034651 ) ) ;
#22447 = DIRECTION ( 'NONE',  ( -0.5449076811759708816, 0.6444004775717707689, 0.5364919789714475140 ) ) ;
#22448 = DIRECTION ( 'NONE',  ( -0.9999697198139514409, -0.000000000000000000, -0.007781995580013368816 ) ) ;
#22449 = DIRECTION ( 'NONE',  ( 0.000000000000000000, -0.000000000000000000, -1.000000000000000000 ) ) ;
#22450 = CARTESIAN_POINT ( 'NONE',  ( -27.99767448711536133, 0.000000000000000000, 7.557179307314289218 ) ) ;
#22451 = DIRECTION ( 'NONE',  ( 0.007781995580012663651, 0.000000000000000000, -0.9999697198139515519 ) ) ;
#22452 = CARTESIAN_POINT ( 'NONE',  ( 2.072287782118878319, 0.000000000000000000, -2.950529333540147015 ) ) ;
#22453 = DIRECTION ( 'NONE',  ( 0.5449076811759707706, 0.6444004775717708799, -0.5364919789714476250 ) ) ;
#22454 =( NAMED_UNIT ( * ) SI_UNIT ( $, .STERADIAN. ) SOLID_ANGLE_UNIT ( ) );
#22455 = CARTESIAN_POINT ( 'NONE',  ( -50.45472955569960760, 3.742236127018431890, 5.000000000000000000 ) ) ;
#22456 = VERTEX_POINT ( 'NONE', #22706 ) ;
#22457 = DIRECTION ( 'NONE',  ( 0.6246952433987893460, 0.7422098413412802076, -0.2426528472758539279 ) ) ;
#22458 = DIRECTION ( 'NONE',  ( 0.005961354470445682716, -0.6427876096865404731, -0.7660212471507180654 ) ) ;
#22459 = PLANE ( 'NONE',  #32678 ) ;
#22460 = PLANE ( 'NONE',  #48650 ) ;
#22461 = DIRECTION ( 'NONE',  ( -0.005002170337468016433, -0.7660444431189770143, 0.6427681459581293666 ) ) ;
#22462 = CARTESIAN_POINT ( 'NONE',  ( 2.072287782118878319, 0.000000000000000000, -2.950529333540147015 ) ) ;
#22463 = CARTESIAN_POINT ( 'NONE',  ( -21.47419595591918906, 0.000000000000000000, 5.222628093224860102 ) ) ;
#22464 = VERTEX_POINT ( 'NONE', #53100 ) ;
#22465 = AXIS2_PLACEMENT_3D ( 'NONE', #10079, #35956, #1572 ) ;
#22466 = ORIENTED_EDGE ( 'NONE', *, *, #208, .T. ) ;
#22467 = CARTESIAN_POINT ( 'NONE',  ( -64.10539783498545319, 7.375519243179410545, 5.000000000000000000 ) ) ;
#22468 = CARTESIAN_POINT ( 'NONE',  ( -27.06708303904391144, 0.000000000000000000, 7.395095371555332697 ) ) ;
#22469 = EDGE_CURVE ( 'NONE', #49361, #5782, #48554, .T. ) ;
#22470 = VECTOR ( 'NONE', #11996, 999.9999999999998863 ) ;
#22471 = ORIENTED_EDGE ( 'NONE', *, *, #22957, .F. ) ;
#22472 = DIRECTION ( 'NONE',  ( -0.000000000000000000, 0.000000000000000000, -1.000000000000000000 ) ) ;
#22473 = EDGE_LOOP ( 'NONE', ( #1485, #55707, #39660, #17728 ) ) ;
#22474 = FACE_OUTER_BOUND ( 'NONE', #33485, .T. ) ;
#22475 = EDGE_CURVE ( 'NONE', #11984, #36837, #18751, .T. ) ;
#22476 = EDGE_CURVE ( 'NONE', #25453, #52834, #19272, .T. ) ;
#22477 = ORIENTED_EDGE ( 'NONE', *, *, #20117, .T. ) ;
#22478 = VERTEX_POINT ( 'NONE', #9672 ) ;
#22479 = ORIENTED_EDGE ( 'NONE', *, *, #30136, .T. ) ;
#22480 = CARTESIAN_POINT ( 'NONE',  ( -17.84275124703420090, 2.714935509636508204, 8.267723343481110376 ) ) ;
#22481 = DIRECTION ( 'NONE',  ( -0.9999697198139514409, -0.000000000000000000, -0.007781995580013368816 ) ) ;
#22482 = LINE ( 'NONE', #27271, #23941 ) ;
#22483 = DIRECTION ( 'NONE',  ( -0.9999697198139514409, -0.000000000000000000, -0.007781995580013368816 ) ) ;
#22484 = ORIENTED_EDGE ( 'NONE', *, *, #33185, .T. ) ;
#22485 = ORIENTED_EDGE ( 'NONE', *, *, #17522, .F. ) ;
#22486 = CARTESIAN_POINT ( 'NONE',  ( -12.90532805278843398, 2.391131607591506114, 5.818443131337661001 ) ) ;
#22487 = ORIENTED_EDGE ( 'NONE', *, *, #11359, .F. ) ;
#22488 = DIRECTION ( 'NONE',  ( 0.007781995580012663651, -3.146120232559066537E-19, -0.9999697198139514409 ) ) ;
#22489 = ORIENTED_EDGE ( 'NONE', *, *, #47669, .F. ) ;
#22490 = DIRECTION ( 'NONE',  ( 0.000000000000000000, -1.000000000000000000, 0.000000000000000000 ) ) ;
#22491 = LINE ( 'NONE', #39802, #14005 ) ;
#22492 = ORIENTED_EDGE ( 'NONE', *, *, #24731, .T. ) ;
#22493 = CARTESIAN_POINT ( 'NONE',  ( -3.638205267667341758, -7.220147766006030032, -1.805171095730843112 ) ) ;
#22494 = ORIENTED_EDGE ( 'NONE', *, *, #12549, .T. ) ;
#22495 = EDGE_CURVE ( 'NONE', #10709, #4830, #53636, .T. ) ;
#22496 = PLANE ( 'NONE',  #7337 ) ;
#22498 = EDGE_CURVE ( 'NONE', #7889, #53576, #26986, .T. ) ;
#22497 = EDGE_LOOP ( 'NONE', ( #40455, #32248, #47389, #35356 ) ) ;
#22499 = FACE_OUTER_BOUND ( 'NONE', #41031, .T. ) ;
#22500 = LINE ( 'NONE', #10260, #13051 ) ;
#22501 = DIRECTION ( 'NONE',  ( -0.005961354470445682716, -0.6427876096865404731, 0.7660212471507180654 ) ) ;
#22502 = ORIENTED_EDGE ( 'NONE', *, *, #34113, .T. ) ;
#22503 = DIRECTION ( 'NONE',  ( 0.000000000000000000, -1.000000000000000000, 0.000000000000000000 ) ) ;
#22504 = AXIS2_PLACEMENT_3D ( 'NONE', #42875, #42032, #28988 ) ;
#22505 = CARTESIAN_POINT ( 'NONE',  ( -17.46532115785441519, 0.000000000000000000, 13.67492996699914265 ) ) ;
#22506 = EDGE_CURVE ( 'NONE', #29959, #51712, #31791, .T. ) ;
#22507 = CARTESIAN_POINT ( 'NONE',  ( -69.53969258253385988, 1.152504438008073340, 7.491856536230704577 ) ) ;
#22508 = CARTESIAN_POINT ( 'NONE',  ( -8.875996589204540044, 0.000000000000000000, 10.41778544861944233 ) ) ;
#22509 = CARTESIAN_POINT ( 'NONE',  ( -19.69569380384165669, -0.1191753592594177458, 14.58090286586150697 ) ) ;
#22510 = DIRECTION ( 'NONE',  ( 0.000000000000000000, -0.000000000000000000, -1.000000000000000000 ) ) ;
#22511 = CARTESIAN_POINT ( 'NONE',  ( -14.00280974873554030, 0.000000000000000000, 12.40921378708904044 ) ) ;
#22512 = ORIENTED_EDGE ( 'NONE', *, *, #17358, .F. ) ;
#22513 = DIRECTION ( 'NONE',  ( 0.000000000000000000, -1.000000000000000000, 0.000000000000000000 ) ) ;
#22514 = CARTESIAN_POINT ( 'NONE',  ( -10.37421533196711465, -0.1191753592594197858, 10.96012406864405975 ) ) ;
#22515 = DIRECTION ( 'NONE',  ( 0.5449076811759707706, 0.6444004775717708799, -0.5364919789714476250 ) ) ;
#22516 = ORIENTED_EDGE ( 'NONE', *, *, #11237, .F. ) ;
#22517 = FACE_OUTER_BOUND ( 'NONE', #46047, .T. ) ;
#22518 = LINE ( 'NONE', #27308, #36341 ) ;
#22519 = ORIENTED_EDGE ( 'NONE', *, *, #16463, .T. ) ;
#22520 = LINE ( 'NONE', #22231, #39803 ) ;
#22521 = DIRECTION ( 'NONE',  ( 0.000000000000000000, -0.000000000000000000, -1.000000000000000000 ) ) ;
#22522 = CARTESIAN_POINT ( 'NONE',  ( -7.594507926423646360, 5.304312555146883490, -0.2684087864660597567 ) ) ;
#22523 = CARTESIAN_POINT ( 'NONE',  ( -21.47341775636118655, -0.1191753592594197858, 5.122631121243466090 ) ) ;
#22524 = EDGE_LOOP ( 'NONE', ( #44430, #52941, #255, #53627 ) ) ;
#22525 = EDGE_LOOP ( 'NONE', ( #22236, #32830, #28432, #38097 ) ) ;
#22526 = CARTESIAN_POINT ( 'NONE',  ( 2.072287782118878319, 0.000000000000000000, -2.950529333540147015 ) ) ;
#22527 = CARTESIAN_POINT ( 'NONE',  ( -10.27421835998572064, 0.000000000000000000, 10.96090226820206048 ) ) ;
#22528 = CARTESIAN_POINT ( 'NONE',  ( -67.15417979359860112, 2.000000000000000444, 6.891331229949076764 ) ) ;
#22529 = EDGE_CURVE ( 'NONE', #50240, #24558, #26495, .T. ) ;
#22530 = FACE_OUTER_BOUND ( 'NONE', #15653, .T. ) ;
#22531 = ADVANCED_FACE ( 'NONE', ( #14476 ), #49681, .F. ) ;
#22532 = LINE ( 'NONE', #13706, #28283 ) ;
#22533 = FACE_OUTER_BOUND ( 'NONE', #52166, .T. ) ;
#22534 = ORIENTED_EDGE ( 'NONE', *, *, #32406, .T. ) ;
#22535 = PLANE ( 'NONE',  #43752 ) ;
#22536 = EDGE_CURVE ( 'NONE', #49583, #47620, #10508, .T. ) ;
#22537 = LINE ( 'NONE', #14561, #16981 ) ;
#22538 = ORIENTED_EDGE ( 'NONE', *, *, #12472, .F. ) ;
#22539 = CARTESIAN_POINT ( 'NONE',  ( -15.80588551452221857, 0.000000000000000000, 5.266740195748627507 ) ) ;
#22540 = DIRECTION ( 'NONE',  ( 0.5364919789714477361, 0.6444004775717706579, 0.5449076811759711036 ) ) ;
#22541 = LINE ( 'NONE', #36164, #45698 ) ;
#22542 = EDGE_LOOP ( 'NONE', ( #32142, #6682, #11233, #10658 ) ) ;
#22543 = VECTOR ( 'NONE', #19007, 1000.000000000000227 ) ;
#22544 = CARTESIAN_POINT ( 'NONE',  ( -19.60912206198628027, -0.1191753592594197858, 4.398475361799976113 ) ) ;
#22545 = EDGE_LOOP ( 'NONE', ( #25330, #41426, #35448, #26424 ) ) ;
#22546 = ADVANCED_FACE ( 'NONE', ( #10203 ), #1105, .F. ) ;
#22547 = ORIENTED_EDGE ( 'NONE', *, *, #25582, .T. ) ;
#22548 = ORIENTED_EDGE ( 'NONE', *, *, #35772, .F. ) ;
#22549 = ORIENTED_EDGE ( 'NONE', *, *, #49046, .F. ) ;
#22550 = DIRECTION ( 'NONE',  ( 0.5449076811759707706, 0.6444004775717708799, -0.5364919789714476250 ) ) ;
#22551 = EDGE_LOOP ( 'NONE', ( #51616, #5858, #10429, #46983 ) ) ;
#22552 = CARTESIAN_POINT ( 'NONE',  ( -18.69292566799212807, -0.1191753592594172323, 5.144269553601169775 ) ) ;
#22553 = FACE_OUTER_BOUND ( 'NONE', #53639, .T. ) ;
#22554 = ORIENTED_EDGE ( 'NONE', *, *, #31867, .T. ) ;
#22555 = LINE ( 'NONE', #944, #5952 ) ;
#22556 = ORIENTED_EDGE ( 'NONE', *, *, #4221, .T. ) ;
#22557 = CARTESIAN_POINT ( 'NONE',  ( -15.13495153988577968, 0.000000000000000000, 12.76973526769478084 ) ) ;
#22558 = EDGE_LOOP ( 'NONE', ( #45056, #913, #15194, #47700 ) ) ;
#22559 = CARTESIAN_POINT ( 'NONE',  ( -17.83139810946674686, -0.1191753592594197858, 13.85674710641801788 ) ) ;
#22560 = CARTESIAN_POINT ( 'NONE',  ( -9.490784343077956819, 0.000000000000000000, 4.007883507648673849 ) ) ;
#22561 = PLANE ( 'NONE',  #21408 ) ;
#22562 = CARTESIAN_POINT ( 'NONE',  ( -10.19994581826036040, 0.000000000000000000, 1.417040160424308359 ) ) ;
#22563 = DIRECTION ( 'NONE',  ( -0.005002170337468016433, -0.7660444431189770143, 0.6427681459581293666 ) ) ;
#22564 = LINE ( 'NONE', #43015, #37406 ) ;
#22565 = VERTEX_POINT ( 'NONE', #27834 ) ;
#22566 = EDGE_LOOP ( 'NONE', ( #34912, #29553, #13233, #26801 ) ) ;
#22567 = DIRECTION ( 'NONE',  ( 0.9999697198139515519, 0.000000000000000000, 0.007781995580013368816 ) ) ;
#22568 = EDGE_CURVE ( 'NONE', #34236, #42663, #36911, .T. ) ;
#22569 = CARTESIAN_POINT ( 'NONE',  ( -21.47263955680318404, 0.000000000000000000, 5.022634149262071190 ) ) ;
#22570 = CARTESIAN_POINT ( 'NONE',  ( -14.94760462649100496, 0.000000000000000000, 2.488088991209854051 ) ) ;
#22571 = CARTESIAN_POINT ( 'NONE',  ( -13.46102625666381059, 0.000000000000000000, 2.499657887821534086 ) ) ;
#22572 = ORIENTED_EDGE ( 'NONE', *, *, #49047, .T. ) ;
#22573 = DIRECTION ( 'NONE',  ( 0.6246952433987894571, -0.7422098413412800966, -0.2426528472758541777 ) ) ;
#22574 = DIRECTION ( 'NONE',  ( 0.007781995580012663651, -3.146120232559066537E-19, -0.9999697198139514409 ) ) ;
#22575 = EDGE_LOOP ( 'NONE', ( #13937, #19676, #31429, #24985, #44160, #29858 ) ) ;
#22576 = DIRECTION ( 'NONE',  ( 0.007781995580012663651, -3.146120232559066537E-19, -0.9999697198139514409 ) ) ;
#22577 = DIRECTION ( 'NONE',  ( 0.9999697198139515519, 0.000000000000000000, 0.007781995580013368816 ) ) ;
#22578 = ORIENTED_EDGE ( 'NONE', *, *, #42529, .T. ) ;
#22579 = EDGE_CURVE ( 'NONE', #4939, #10700, #14219, .T. ) ;
#22580 = AXIS2_PLACEMENT_3D ( 'NONE', #40671, #1478, #23608 ) ;
#22581 = CARTESIAN_POINT ( 'NONE',  ( -68.91359625414428081, -8.992215709865041262, 7.224037831218169003 ) ) ;
#22582 = PLANE ( 'NONE',  #37820 ) ;
#22583 = CARTESIAN_POINT ( 'NONE',  ( -14.12565709746768761, 0.000000000000000000, 2.494485576937521820 ) ) ;
#22584 = ADVANCED_FACE ( 'NONE', ( #32074 ), #45143, .F. ) ;
#22585 = ADVANCED_FACE ( 'NONE', ( #27527 ), #5662, .F. ) ;
#22586 = PLANE ( 'NONE',  #34106 ) ;
#22587 = CARTESIAN_POINT ( 'NONE',  ( -18.18100488926467762, -1.165603555308155626, 5.657005471572626121 ) ) ;
#22588 = EDGE_LOOP ( 'NONE', ( #36349, #12483, #50876, #54705 ) ) ;
#22589 = EDGE_LOOP ( 'NONE', ( #36171, #39462, #39663, #20148 ) ) ;
#22590 = CARTESIAN_POINT ( 'NONE',  ( -20.56204410600856747, -4.565544526780663581, 4.722652564258249974 ) ) ;
#22591 = CARTESIAN_POINT ( 'NONE',  ( -14.10280672071693431, -0.1191753592594197858, 12.40843558753103792 ) ) ;
#22592 = FACE_OUTER_BOUND ( 'NONE', #54513, .T. ) ;
#22593 = ADVANCED_FACE ( 'NONE', ( #22991 ), #44848, .F. ) ;
#22594 = DIRECTION ( 'NONE',  ( 0.9999697198139515519, 0.000000000000000000, 0.007781995580013368816 ) ) ;
#22595 = EDGE_CURVE ( 'NONE', #40269, #14453, #25239, .T. ) ;
#22596 = CARTESIAN_POINT ( 'NONE',  ( -11.77243710274829525, -0.1191753592594197858, 11.50324088822667612 ) ) ;
#22597 = ORIENTED_EDGE ( 'NONE', *, *, #20617, .T. ) ;
#22598 = PLANE ( 'NONE',  #30997 ) ;
#22599 = DIRECTION ( 'NONE',  ( 0.6427681459581294776, -0.7660444431189769032, 0.005002170337467562802 ) ) ;
#22600 = EDGE_CURVE ( 'NONE', #14438, #49029, #51047, .T. ) ;
#22601 = CARTESIAN_POINT ( 'NONE',  ( -15.95869604799166375, -4.079838673713163111, 2.950052407828571255 ) ) ;
#22602 = CARTESIAN_POINT ( 'NONE',  ( 2.072287782118878319, 0.000000000000000000, -2.950529333540147015 ) ) ;
#22603 = ORIENTED_EDGE ( 'NONE', *, *, #10484, .F. ) ;
#22604 = CARTESIAN_POINT ( 'NONE',  ( -14.20280369269832832, 0.000000000000000000, 12.40765738797303719 ) ) ;
#22605 = ORIENTED_EDGE ( 'NONE', *, *, #30015, .T. ) ;
#22606 = FACE_OUTER_BOUND ( 'NONE', #20715, .T. ) ;
#22607 = DIRECTION ( 'NONE',  ( 0.007781995580012662783, 0.000000000000000000, -0.9999697198139514409 ) ) ;
#22608 = EDGE_CURVE ( 'NONE', #54876, #35486, #32894, .T. ) ;
#22609 = ORIENTED_EDGE ( 'NONE', *, *, #14564, .T. ) ;
#22610 = CARTESIAN_POINT ( 'NONE',  ( -12.80458192191714595, 0.000000000000000000, 11.86454056839041726 ) ) ;
#22611 = EDGE_LOOP ( 'NONE', ( #44174, #32542, #5866, #46586 ) ) ;
#22612 = EDGE_CURVE ( 'NONE', #26046, #50963, #2771, .T. ) ;
#22613 = VERTEX_POINT ( 'NONE', #37737 ) ;
#22614 = ORIENTED_EDGE ( 'NONE', *, *, #35409, .T. ) ;
#22615 = DIRECTION ( 'NONE',  ( 0.7660212471507180654, -0.6427876096865404731, 0.005961354470445141482 ) ) ;
#22616 = ORIENTED_EDGE ( 'NONE', *, *, #24669, .F. ) ;
#22617 = ORIENTED_EDGE ( 'NONE', *, *, #19814, .F. ) ;
#22618 = CARTESIAN_POINT ( 'NONE',  ( -19.39860431275360853, 21.26603824944626808, -4.250162336171596777 ) ) ;
#22619 = LINE ( 'NONE', #54865, #39439 ) ;
#22620 = ORIENTED_EDGE ( 'NONE', *, *, #35399, .T. ) ;
#22621 = ORIENTED_EDGE ( 'NONE', *, *, #13636, .F. ) ;
#22622 = DIRECTION ( 'NONE',  ( 0.005961354470445682716, -0.6427876096865404731, -0.7660212471507180654 ) ) ;
#22623 = ORIENTED_EDGE ( 'NONE', *, *, #23993, .T. ) ;
#22624 = VERTEX_POINT ( 'NONE', #46812 ) ;
#22625 = FACE_OUTER_BOUND ( 'NONE', #43474, .T. ) ;
#22626 = CARTESIAN_POINT ( 'NONE',  ( -16.53317331066696383, 0.000000000000000000, 13.31285208727739899 ) ) ;
#22627 = DIRECTION ( 'NONE',  ( 0.000000000000000000, -1.000000000000000000, 0.000000000000000000 ) ) ;
#22628 = FACE_OUTER_BOUND ( 'NONE', #28493, .T. ) ;
#22629 = ORIENTED_EDGE ( 'NONE', *, *, #56058, .T. ) ;
#22630 = PLANE ( 'NONE',  #34660 ) ;
#22631 = ORIENTED_EDGE ( 'NONE', *, *, #7641, .T. ) ;
#22632 = EDGE_CURVE ( 'NONE', #30203, #33225, #3636, .T. ) ;
#22633 = CARTESIAN_POINT ( 'NONE',  ( -16.79925329029790149, 0.000000000000000000, 13.49544742625427496 ) ) ;
#22634 = PLANE ( 'NONE',  #34232 ) ;
#22635 = DIRECTION ( 'NONE',  ( 0.7660212471507180654, -0.6427876096865404731, 0.005961354470445141482 ) ) ;
#22636 = CARTESIAN_POINT ( 'NONE',  ( -22.03910228076049904, -5.213152330870665097, 5.275730040889094141 ) ) ;
#22637 = CARTESIAN_POINT ( 'NONE',  ( 5.907100548706921472, -1.017206782221826478, 1.544798379698097079 ) ) ;
#22638 = DIRECTION ( 'NONE',  ( -0.005961354470445682716, -0.6427876096865404731, 0.7660212471507180654 ) ) ;
#22639 = LINE ( 'NONE', #31725, #24101 ) ;
#22640 = ORIENTED_EDGE ( 'NONE', *, *, #25658, .T. ) ;
#22641 = CARTESIAN_POINT ( 'NONE',  ( -17.74560456716937296, 0.000000000000000000, 3.774316574337878372 ) ) ;
#22642 = ADVANCED_FACE ( 'NONE', ( #50773 ), #38272, .F. ) ;
#22643 = DIRECTION ( 'NONE',  ( 0.9335804264972041855, -0.3583679495452941066, 0.000000000000000000 ) ) ;
#22644 = FACE_OUTER_BOUND ( 'NONE', #50548, .T. ) ;
#22645 = DIRECTION ( 'NONE',  ( 0.000000000000000000, -1.000000000000000000, 0.000000000000000000 ) ) ;
#22646 = DIRECTION ( 'NONE',  ( 0.005002170337468016433, -0.7660444431189770143, -0.6427681459581293666 ) ) ;
#22647 = CARTESIAN_POINT ( 'NONE',  ( -17.26532721389163072, 0.000000000000000000, 13.67648636611514590 ) ) ;
#22648 = EDGE_CURVE ( 'NONE', #4507, #9909, #15562, .T. ) ;
#22649 = FACE_OUTER_BOUND ( 'NONE', #17871, .T. ) ;
#22650 = CARTESIAN_POINT ( 'NONE',  ( -69.30403031588791407, -1.000000000000000666, -6.450409451741321298 ) ) ;
#22651 = ORIENTED_EDGE ( 'NONE', *, *, #40840, .T. ) ;
#22652 = FACE_OUTER_BOUND ( 'NONE', #11434, .T. ) ;
#22653 = DIRECTION ( 'NONE',  ( 0.000000000000000000, -0.000000000000000000, -1.000000000000000000 ) ) ;
#22654 = DIRECTION ( 'NONE',  ( 0.000000000000000000, -0.000000000000000000, -1.000000000000000000 ) ) ;
#22655 = LINE ( 'NONE', #49049, #30988 ) ;
#22656 = EDGE_CURVE ( 'NONE', #50804, #28121, #16406, .T. ) ;
#22657 = DIRECTION ( 'NONE',  ( 0.007781995580012662783, 0.000000000000000000, -0.9999697198139514409 ) ) ;
#22658 = DIRECTION ( 'NONE',  ( -0.000000000000000000, -0.000000000000000000, 1.000000000000000000 ) ) ;
#22659 = DIRECTION ( 'NONE',  ( -0.9999697198139514409, -0.000000000000000000, -0.007781995580013368816 ) ) ;
#22660 = ADVANCED_FACE ( 'NONE', ( #12156 ), #29191, .F. ) ;
#22661 = CARTESIAN_POINT ( 'NONE',  ( -67.57495167298797867, -9.577535775341699420, 4.288727116335238065 ) ) ;
#22662 = EDGE_CURVE ( 'NONE', #1435, #16888, #46500, .T. ) ;
#22663 = FACE_OUTER_BOUND ( 'NONE', #29619, .T. ) ;
#22664 = EDGE_CURVE ( 'NONE', #43677, #5292, #41007, .T. ) ;
#22665 = ORIENTED_EDGE ( 'NONE', *, *, #22246, .F. ) ;
#22666 = ADVANCED_FACE ( 'NONE', ( #41440 ), #11610, .F. ) ;
#22667 = ORIENTED_EDGE ( 'NONE', *, *, #23780, .T. ) ;
#22668 = ORIENTED_EDGE ( 'NONE', *, *, #28916, .T. ) ;
#22669 = VERTEX_POINT ( 'NONE', #7618 ) ;
#22670 = VERTEX_POINT ( 'NONE', #15854 ) ;
#22671 = FACE_OUTER_BOUND ( 'NONE', #50602, .T. ) ;
#22672 = CARTESIAN_POINT ( 'NONE',  ( -18.23691093166689114, -0.1191753592594171213, 6.255814575142474077 ) ) ;
#22673 = ORIENTED_EDGE ( 'NONE', *, *, #29835, .F. ) ;
#22674 = ORIENTED_EDGE ( 'NONE', *, *, #7426, .F. ) ;
#22675 = VECTOR ( 'NONE', #22079, 1000.000000000000114 ) ;
#22676 = ORIENTED_EDGE ( 'NONE', *, *, #40051, .T. ) ;
#22677 = PLANE ( 'NONE',  #7376 ) ;
#22678 = LINE ( 'NONE', #14719, #13271 ) ;
#22679 = ORIENTED_EDGE ( 'NONE', *, *, #38751, .F. ) ;
#22680 = CARTESIAN_POINT ( 'NONE',  ( -27.06708303904391144, 0.000000000000000000, 7.395095371555332697 ) ) ;
#22681 = EDGE_CURVE ( 'NONE', #39740, #36296, #20945, .T. ) ;
#22682 = ORIENTED_EDGE ( 'NONE', *, *, #50634, .F. ) ;
#22683 = LINE ( 'NONE', #31511, #7362 ) ;
#22684 = ADVANCED_FACE ( 'NONE', ( #54459 ), #33201, .F. ) ;
#22685 = CARTESIAN_POINT ( 'NONE',  ( -16.81190032086591302, 0.000000000000000000, 3.212244750653343583 ) ) ;
#22686 = CARTESIAN_POINT ( 'NONE',  ( -21.47341775636118655, -0.1191753592594197858, 5.122631121243466090 ) ) ;
#22687 = PLANE ( 'NONE',  #51406 ) ;
#22688 = ORIENTED_EDGE ( 'NONE', *, *, #55280, .T. ) ;
#22689 = DIRECTION ( 'NONE',  ( 0.000000000000000000, -1.000000000000000000, 0.000000000000000000 ) ) ;
#22690 = DIRECTION ( 'NONE',  ( 0.5364919789714477361, 0.6444004775717706579, 0.5449076811759711036 ) ) ;
#22691 = LINE ( 'NONE', #18427, #18517 ) ;
#22692 = EDGE_CURVE ( 'NONE', #3186, #15388, #24947, .T. ) ;
#22693 = ORIENTED_EDGE ( 'NONE', *, *, #51788, .T. ) ;
#22694 = CARTESIAN_POINT ( 'NONE',  ( -19.60990026154428278, 0.000000000000000000, 4.498472333781370125 ) ) ;
#22695 = EDGE_LOOP ( 'NONE', ( #2602, #31879, #29090, #35297 ) ) ;
#22696 = EDGE_CURVE ( 'NONE', #34917, #47902, #2521, .T. ) ;
#22697 = EDGE_CURVE ( 'NONE', #41830, #7042, #7082, .T. ) ;
#22698 = ADVANCED_FACE ( 'NONE', ( #34576 ), #48188, .F. ) ;
#22699 = PLANE ( 'NONE',  #12894 ) ;
#22700 = CARTESIAN_POINT ( 'NONE',  ( -14.20280369269832832, 0.000000000000000000, 12.40765738797303719 ) ) ;
#22701 = LINE ( 'NONE', #5392, #18592 ) ;
#22702 = FACE_OUTER_BOUND ( 'NONE', #6627, .T. ) ;
#22703 = DIRECTION ( 'NONE',  ( 0.7660212471507180654, -0.6427876096865404731, 0.005961354470445141482 ) ) ;
#22704 = CARTESIAN_POINT ( 'NONE',  ( -25.20278734466900517, 0.000000000000000000, 6.670939612111840944 ) ) ;
#22705 = CARTESIAN_POINT ( 'NONE',  ( -11.87243407472968926, 0.000000000000000000, 11.50246268866867361 ) ) ;
#22706 = CARTESIAN_POINT ( 'NONE',  ( -70.10169143752739274, -0.9999999999999995559, 7.503902134509972122 ) ) ;
#22707 = SHAPE_REPRESENTATION_RELATIONSHIP ( 'NONE' , 'NONE' ,  #24540, #27288 ) ;
#22708 = CARTESIAN_POINT ( 'NONE',  ( -17.82299174236657180, -4.079838673713163111, 3.674208167272060788 ) ) ;
#22709 = ORIENTED_EDGE ( 'NONE', *, *, #42963, .T. ) ;
#22710 = DIRECTION ( 'NONE',  ( -0.7660212471507179544, -0.6427876096865405842, -0.005961354470445141482 ) ) ;
#22711 = PLANE ( 'NONE',  #13157 ) ;
#22712 = DIRECTION ( 'NONE',  ( -0.005002170337468016433, -0.7660444431189770143, 0.6427681459581293666 ) ) ;
#22713 = LINE ( 'NONE', #14226, #55904 ) ;
#22714 = LINE ( 'NONE', #26403, #39995 ) ;
#22715 = EDGE_CURVE ( 'NONE', #37895, #2677, #24797, .T. ) ;
#22716 = PLANE ( 'NONE',  #33294 ) ;
#22717 = CARTESIAN_POINT ( 'NONE',  ( -25.20123094555300369, 0.000000000000000000, 6.470945668149052032 ) ) ;
#22718 = ORIENTED_EDGE ( 'NONE', *, *, #45981, .F. ) ;
#22719 = VECTOR ( 'NONE', #13079, 999.9999999999998863 ) ;
#22720 = EDGE_CURVE ( 'NONE', #13435, #16069, #8462, .T. ) ;
#22721 = EDGE_LOOP ( 'NONE', ( #31517, #37202, #50346, #10685 ) ) ;
#22722 = EDGE_CURVE ( 'NONE', #53290, #8704, #26621, .T. ) ;
#22723 = LINE ( 'NONE', #40035, #591 ) ;
#22724 = LINE ( 'NONE', #39503, #1388 ) ;
#22725 = EDGE_CURVE ( 'NONE', #16370, #52808, #47936, .T. ) ;
#22726 = ORIENTED_EDGE ( 'NONE', *, *, #32616, .F. ) ;
#22727 = DIRECTION ( 'NONE',  ( 0.005002170337468016433, -0.7660444431189770143, -0.6427681459581293666 ) ) ;
#22728 = VERTEX_POINT ( 'NONE', #17545 ) ;
#22729 = LINE ( 'NONE', #292, #36555 ) ;
#22730 = EDGE_CURVE ( 'NONE', #24292, #37046, #43116, .T. ) ;
#22731 = ORIENTED_EDGE ( 'NONE', *, *, #45998, .T. ) ;
#22732 = EDGE_LOOP ( 'NONE', ( #37917, #41613, #35389, #40876 ) ) ;
#22733 = ORIENTED_EDGE ( 'NONE', *, *, #48258, .T. ) ;
#22734 = DIRECTION ( 'NONE',  ( 0.7660212471507180654, -0.6427876096865404731, 0.005961354470445141482 ) ) ;
#22735 = LINE ( 'NONE', #26170, #44110 ) ;
#22736 = DIRECTION ( 'NONE',  ( 0.9999697198139515519, 0.000000000000000000, 0.007781995580013368816 ) ) ;
#22737 = VECTOR ( 'NONE', #8219, 1000.000000000000227 ) ;
#22738 = CARTESIAN_POINT ( 'NONE',  ( -16.53317331066696383, 0.000000000000000000, 13.31285208727739899 ) ) ;
#22739 = ORIENTED_EDGE ( 'NONE', *, *, #7285, .F. ) ;
#22740 = ORIENTED_EDGE ( 'NONE', *, *, #30452, .F. ) ;
#22741 = LINE ( 'NONE', #618, #21836 ) ;
#22742 = EDGE_LOOP ( 'NONE', ( #54377, #24741, #7816, #14398 ) ) ;
#22743 = LINE ( 'NONE', #23034, #50909 ) ;
#22744 = VERTEX_POINT ( 'NONE', #13309 ) ;
#22745 = DIRECTION ( 'NONE',  ( -0.5364919789714478471, 0.6444004775717705469, -0.5449076811759709926 ) ) ;
#22746 = LINE ( 'NONE', #22196, #18542 ) ;
#22747 = ORIENTED_EDGE ( 'NONE', *, *, #5427, .F. ) ;
#22748 = AXIS2_PLACEMENT_3D ( 'NONE', #54803, #33254, #24696 ) ;
#22749 = DIRECTION ( 'NONE',  ( -0.5364919789714478471, 0.6444004775717705469, -0.5449076811759709926 ) ) ;
#22750 = ORIENTED_EDGE ( 'NONE', *, *, #44030, .T. ) ;
#22751 = AXIS2_PLACEMENT_3D ( 'NONE', #12163, #8193, #25244 ) ;
#22752 = DIRECTION ( 'NONE',  ( 0.007781995580012663651, -3.146120232559066537E-19, -0.9999697198139514409 ) ) ;
#22753 = EDGE_CURVE ( 'NONE', #15979, #24781, #12725, .T. ) ;
#22754 = EDGE_LOOP ( 'NONE', ( #55968, #15173, #18613, #38494 ) ) ;
#22755 = DIRECTION ( 'NONE',  ( 0.9999697198139515519, 0.000000000000000000, 0.007781995580013368816 ) ) ;
#22756 = DIRECTION ( 'NONE',  ( 0.9999697198139515519, 0.000000000000000000, 0.007781995580013368816 ) ) ;
#22757 = DIRECTION ( 'NONE',  ( 0.7660212471507180654, -0.6427876096865404731, 0.005961354470445141482 ) ) ;
#22758 = ORIENTED_EDGE ( 'NONE', *, *, #42445, .F. ) ;
#22759 = ADVANCED_FACE ( 'NONE', ( #4231 ), #21240, .F. ) ;
#22760 = EDGE_CURVE ( 'NONE', #7707, #15806, #42807, .T. ) ;
#22761 = FACE_OUTER_BOUND ( 'NONE', #54324, .T. ) ;
#22762 = FACE_OUTER_BOUND ( 'NONE', #53131, .T. ) ;
#22763 = DIRECTION ( 'NONE',  ( 1.000000000000000000, 0.000000000000000000, 0.000000000000000000 ) ) ;
#22764 = EDGE_CURVE ( 'NONE', #20837, #31183, #508, .T. ) ;
#22765 = CARTESIAN_POINT ( 'NONE',  ( -19.68728743674148163, -4.079838673713161334, 4.398363926715553873 ) ) ;
#22766 = DIRECTION ( 'NONE',  ( -0.5364919789714478471, 0.6444004775717705469, -0.5449076811759709926 ) ) ;
#22767 = CARTESIAN_POINT ( 'NONE',  ( -67.27407007597652466, -11.42230648536675908, 4.403654818465663645 ) ) ;
#22768 = ORIENTED_EDGE ( 'NONE', *, *, #48950, .F. ) ;
#22769 = DIRECTION ( 'NONE',  ( 0.000000000000000000, -1.000000000000000000, 0.000000000000000000 ) ) ;
#22770 = CARTESIAN_POINT ( 'NONE',  ( -13.76734565315850745, -4.727446477803162850, 9.788181382680596343 ) ) ;
#22771 = FACE_OUTER_BOUND ( 'NONE', #19195, .T. ) ;
#22772 = ORIENTED_EDGE ( 'NONE', *, *, #8278, .F. ) ;
#22773 = CARTESIAN_POINT ( 'NONE',  ( -16.43317633868556626, -0.1191753592594197858, 13.31363028683540151 ) ) ;
#22774 = DIRECTION ( 'NONE',  ( 0.007781995580012663651, -3.146120232559066537E-19, -0.9999697198139514409 ) ) ;
#22775 = ORIENTED_EDGE ( 'NONE', *, *, #37135, .T. ) ;
#22776 = LINE ( 'NONE', #48329, #16199 ) ;
#22777 = VECTOR ( 'NONE', #14227, 999.9999999999998863 ) ;
#22778 = VECTOR ( 'NONE', #48025, 1000.000000000000114 ) ;
#22779 = LINE ( 'NONE', #43791, #38426 ) ;
#22780 = CARTESIAN_POINT ( 'NONE',  ( -14.50831954291707504, -0.1191753592594190225, 4.807503056255493235 ) ) ;
#22781 = EDGE_CURVE ( 'NONE', #6333, #30167, #17001, .T. ) ;
#22782 = DIRECTION ( 'NONE',  ( 0.000000000000000000, -0.000000000000000000, -1.000000000000000000 ) ) ;
#22783 = EDGE_LOOP ( 'NONE', ( #51132, #37333, #37076, #38306 ) ) ;
#22784 = ORIENTED_EDGE ( 'NONE', *, *, #27866, .F. ) ;
#22785 = DIRECTION ( 'NONE',  ( 0.7660212471507180654, -0.6427876096865404731, 0.005961354470445141482 ) ) ;
#22786 = PLANE ( 'NONE',  #42251 ) ;
#22787 = CARTESIAN_POINT ( 'NONE',  ( -23.59415828741828136, 18.97399401843694022, -4.500635383149576896 ) ) ;
#22788 = CARTESIAN_POINT ( 'NONE',  ( -18.81381921406850211, 0.000000000000000000, 7.828656248828915309 ) ) ;
#22789 = EDGE_CURVE ( 'NONE', #15659, #22728, #21546, .T. ) ;
#22790 = LINE ( 'NONE', #49182, #15581 ) ;
#22791 = DIRECTION ( 'NONE',  ( -0.005961354470445682716, -0.6427876096865404731, 0.7660212471507180654 ) ) ;
#22792 = ORIENTED_EDGE ( 'NONE', *, *, #15241, .T. ) ;
#22793 = DIRECTION ( 'NONE',  ( 0.6427681459581294776, -0.7660444431189769032, 0.005002170337467562802 ) ) ;
#22794 = ADVANCED_FACE ( 'NONE', ( #25497 ), #30048, .F. ) ;
#22795 = AXIS2_PLACEMENT_3D ( 'NONE', #41723, #19615, #36948 ) ;
#22796 = FACE_OUTER_BOUND ( 'NONE', #20016, .T. ) ;
#22797 = ORIENTED_EDGE ( 'NONE', *, *, #14949, .F. ) ;
#22798 = ADVANCED_FACE ( 'NONE', ( #3915 ), #22085, .F. ) ;
#22799 = CARTESIAN_POINT ( 'NONE',  ( -18.67775241435682432, 0.000000000000000000, 4.136394454059623804 ) ) ;
#22800 = DIRECTION ( 'NONE',  ( 0.000000000000000000, -0.000000000000000000, -1.000000000000000000 ) ) ;
#22801 = LINE ( 'NONE', #13179, #54694 ) ;
#22802 = ORIENTED_EDGE ( 'NONE', *, *, #300, .F. ) ;
#22803 = LINE ( 'NONE', #4934, #10365 ) ;
#22804 = ADVANCED_FACE ( 'NONE', ( #47655 ), #8775, .F. ) ;
#22805 = ORIENTED_EDGE ( 'NONE', *, *, #44269, .T. ) ;
#22806 = ORIENTED_EDGE ( 'NONE', *, *, #44249, .F. ) ;
#22807 = ORIENTED_EDGE ( 'NONE', *, *, #44499, .T. ) ;
#22808 = VERTEX_POINT ( 'NONE', #43396 ) ;
#22809 = CARTESIAN_POINT ( 'NONE',  ( -68.87050791938486327, -8.585715889274698753, -6.450409451741323075 ) ) ;
#22810 = PRODUCT ( 'BR-836', 'BR-836', '', ( #47656 ) ) ;
#22811 = VERTEX_POINT ( 'NONE', #47353 ) ;
#22812 = PLANE ( 'NONE',  #476 ) ;
#22813 = FACE_OUTER_BOUND ( 'NONE', #44737, .T. ) ;
#22814 = VECTOR ( 'NONE', #42748, 1000.000000000000227 ) ;
#22815 = VECTOR ( 'NONE', #37143, 1000.000000000000227 ) ;
#22816 = ORIENTED_EDGE ( 'NONE', *, *, #19953, .T. ) ;
#22817 = DIRECTION ( 'NONE',  ( 0.007781995580012663651, 0.000000000000000000, -0.9999697198139515519 ) ) ;
#22818 = VERTEX_POINT ( 'NONE', #4493 ) ;
#22819 = FACE_OUTER_BOUND ( 'NONE', #34297, .T. ) ;
#22820 = ORIENTED_EDGE ( 'NONE', *, *, #55468, .F. ) ;
#22821 = CARTESIAN_POINT ( 'NONE',  ( -18.66354898467281132, 0.000000000000000000, 14.21960318569776582 ) ) ;
#22822 = CARTESIAN_POINT ( 'NONE',  ( -19.79569077582305070, 0.000000000000000000, 14.58012466630350445 ) ) ;
#22823 = VECTOR ( 'NONE', #12301, 999.9999999999998863 ) ;
#22824 = FACE_OUTER_BOUND ( 'NONE', #31696, .T. ) ;
#22825 = CARTESIAN_POINT ( 'NONE',  ( -10.32658747134729893, -0.1191753592594177180, 4.840046262167575719 ) ) ;
#22826 = DIRECTION ( 'NONE',  ( -0.5449076811759708816, 0.6444004775717707689, 0.5364919789714475140 ) ) ;
#22827 = DIRECTION ( 'NONE',  ( 0.9999697198139515519, 0.000000000000000000, 0.007781995580013368816 ) ) ;
#22828 = ORIENTED_EDGE ( 'NONE', *, *, #24153, .T. ) ;
#22829 = EDGE_CURVE ( 'NONE', #15522, #51817, #26336, .T. ) ;
#22830 = VERTEX_POINT ( 'NONE', #13569 ) ;
#22831 = DIRECTION ( 'NONE',  ( -0.9999697198139514409, -0.000000000000000000, -0.007781995580013368816 ) ) ;
#22832 = DIRECTION ( 'NONE',  ( 0.005961354470445682716, -0.6427876096865404731, -0.7660212471507180654 ) ) ;
#22833 = ADVANCED_FACE ( 'NONE', ( #27185 ), #26929, .F. ) ;
#22834 = EDGE_CURVE ( 'NONE', #21349, #5026, #10141, .T. ) ;
#22835 = VECTOR ( 'NONE', #2202, 999.9999999999998863 ) ;
#22836 = DIRECTION ( 'NONE',  ( -0.005961354470445682716, -0.6427876096865404731, 0.7660212471507180654 ) ) ;
#22837 = CARTESIAN_POINT ( 'NONE',  ( -15.37403964991131744, 2.553033558614007603, 7.043083237409386577 ) ) ;
#22838 = ORIENTED_EDGE ( 'NONE', *, *, #42963, .F. ) ;
#22839 = DIRECTION ( 'NONE',  ( 0.9999697198139515519, 0.000000000000000000, 0.007781995580013368816 ) ) ;
#22840 = FACE_OUTER_BOUND ( 'NONE', #21706, .T. ) ;
#22841 = ORIENTED_EDGE ( 'NONE', *, *, #2406, .T. ) ;
#22842 = CARTESIAN_POINT ( 'NONE',  ( -13.08330893211609869, 0.000000000000000000, 1.763933231766363630 ) ) ;
#22843 = PLANE ( 'NONE',  #43074 ) ;
#22844 = ORIENTED_EDGE ( 'NONE', *, *, #32289, .T. ) ;
#22845 = DIRECTION ( 'NONE',  ( 0.6427681459581294776, -0.7660444431189769032, 0.005002170337467562802 ) ) ;
#22846 = DIRECTION ( 'NONE',  ( 0.000000000000000000, -1.000000000000000000, 0.000000000000000000 ) ) ;
#22847 = FACE_OUTER_BOUND ( 'NONE', #2343, .T. ) ;
#22848 = CARTESIAN_POINT ( 'NONE',  ( -16.18500926415040553, -5.375054281893163477, 11.79011876919352630 ) ) ;
#22849 = ADVANCED_FACE ( 'NONE', ( #48486 ), #17329, .T. ) ;
#22850 = CARTESIAN_POINT ( 'NONE',  ( -11.40636015113596180, 0.000000000000000000, 11.32142374880780089 ) ) ;
#22851 = ORIENTED_EDGE ( 'NONE', *, *, #29591, .T. ) ;
#22852 = EDGE_LOOP ( 'NONE', ( #33375, #18058, #27364, #40124 ) ) ;
#22853 = LINE ( 'NONE', #35112, #25792 ) ;
#22854 = CARTESIAN_POINT ( 'NONE',  ( -19.60834386242827776, 0.000000000000000000, 4.298478389818581213 ) ) ;
#22855 = CARTESIAN_POINT ( 'NONE',  ( -29.86352658060627618, 0.000000000000000000, 8.481329010720569883 ) ) ;
#22856 = AXIS2_PLACEMENT_3D ( 'NONE', #35571, #23371, #5761 ) ;
#22857 = VECTOR ( 'NONE', #33864, 1000.000000000000227 ) ;
#22858 = FACE_OUTER_BOUND ( 'NONE', #22104, .T. ) ;
#22859 = CARTESIAN_POINT ( 'NONE',  ( 5.515141197255969630, -1.062154408800312755, -2.500037664106760094 ) ) ;
#22860 = EDGE_LOOP ( 'NONE', ( #34472, #41653, #1793, #25068 ) ) ;
#22861 = DIRECTION ( 'NONE',  ( 0.007781995580012662783, 0.000000000000000000, -0.9999697198139514409 ) ) ;
#22862 = ADVANCED_FACE ( 'NONE', ( #52729 ), #13836, .F. ) ;
#22863 = CARTESIAN_POINT ( 'NONE',  ( -13.46390031016909283, 0.000000000000000000, 2.868967591079298884 ) ) ;
#22864 = CARTESIAN_POINT ( 'NONE',  ( -17.79239240936278321, -0.1191753592594190225, 8.844598409714835796 ) ) ;
#22865 = CARTESIAN_POINT ( 'NONE',  ( -32.65997012216863737, 0.000000000000000000, 9.567562649885804404 ) ) ;
#22866 = VECTOR ( 'NONE', #19894, 1000.000000000000114 ) ;
#22867 = ORIENTED_EDGE ( 'NONE', *, *, #12731, .F. ) ;
#22868 = PLANE ( 'NONE',  #2981 ) ;
#22869 = ORIENTED_EDGE ( 'NONE', *, *, #41848, .F. ) ;
#22870 = PLANE ( 'NONE',  #35897 ) ;
#22871 = CARTESIAN_POINT ( 'NONE',  ( -21.47263955680318404, 0.000000000000000000, 5.022634149262071190 ) ) ;
#22872 = ORIENTED_EDGE ( 'NONE', *, *, #16092, .F. ) ;
#22873 = DIRECTION ( 'NONE',  ( 0.007781995580012663651, -3.146120232559066537E-19, -0.9999697198139514409 ) ) ;
#22874 = ADVANCED_FACE ( 'NONE', ( #6190 ), #49326, .F. ) ;
#22875 = VECTOR ( 'NONE', #11842, 999.9999999999998863 ) ;
#22876 = ORIENTED_EDGE ( 'NONE', *, *, #7430, .T. ) ;
#22877 = ORIENTED_EDGE ( 'NONE', *, *, #47970, .F. ) ;
#22878 = ORIENTED_EDGE ( 'NONE', *, *, #42845, .T. ) ;
#22879 = PLANE ( 'NONE',  #43855 ) ;
#22880 = ORIENTED_EDGE ( 'NONE', *, *, #24070, .T. ) ;
#22881 = ORIENTED_EDGE ( 'NONE', *, *, #959, .T. ) ;
#22882 = CARTESIAN_POINT ( 'NONE',  ( -14.16745024565764943, 0.000000000000000000, 7.864815366509013472 ) ) ;
#22883 = CARTESIAN_POINT ( 'NONE',  ( -12.26579185571406327, 0.000000000000000000, 2.339633464714584221 ) ) ;
#22884 = VERTEX_POINT ( 'NONE', #40809 ) ;
#22885 = EDGE_CURVE ( 'NONE', #43913, #8391, #1882, .T. ) ;
#22886 = ORIENTED_EDGE ( 'NONE', *, *, #40972, .F. ) ;
#22887 = DIRECTION ( 'NONE',  ( 0.007781995580012663651, -3.146120232559066537E-19, -0.9999697198139514409 ) ) ;
#22888 = ORIENTED_EDGE ( 'NONE', *, *, #29748, .T. ) ;
#22889 = VECTOR ( 'NONE', #20099, 999.9999999999998863 ) ;
#22890 = EDGE_CURVE ( 'NONE', #29145, #10401, #19205, .T. ) ;
#22891 = ORIENTED_EDGE ( 'NONE', *, *, #50647, .F. ) ;
#22892 = ADVANCED_FACE ( 'NONE', ( #34765 ), #25683, .F. ) ;
#22893 = FACE_OUTER_BOUND ( 'NONE', #31347, .T. ) ;
#22894 = DIRECTION ( 'NONE',  ( 0.007781995580012662783, 0.000000000000000000, -0.9999697198139514409 ) ) ;
#22895 = DIRECTION ( 'NONE',  ( 0.9999697198139515519, 0.000000000000000000, 0.007781995580013368816 ) ) ;
#22896 = CARTESIAN_POINT ( 'NONE',  ( -27.06552663992790997, 0.000000000000000000, 7.195101427592543786 ) ) ;
#22897 = VECTOR ( 'NONE', #54930, 1000.000000000000114 ) ;
#22898 = EDGE_CURVE ( 'NONE', #22811, #21349, #21445, .T. ) ;
#22899 = VERTEX_POINT ( 'NONE', #51540 ) ;
#22900 = CARTESIAN_POINT ( 'NONE',  ( 2.072287782118878319, 0.000000000000000000, -2.950529333540147015 ) ) ;
#22901 = ORIENTED_EDGE ( 'NONE', *, *, #47717, .T. ) ;
#22902 = VECTOR ( 'NONE', #41697, 999.9999999999998863 ) ;
#22903 = CIRCLE ( 'NONE', #31940, 2.000000000000002220 ) ;
#22904 = EDGE_CURVE ( 'NONE', #48219, #29153, #9485, .T. ) ;
#22905 = CARTESIAN_POINT ( 'NONE',  ( -13.76455401191414651, -4.241740624735664156, 2.092607607751481691 ) ) ;
#22906 = EDGE_CURVE ( 'NONE', #51591, #19370, #13735, .T. ) ;
#22907 = CARTESIAN_POINT ( 'NONE',  ( -17.46532115785441519, 0.000000000000000000, 13.67492996699914265 ) ) ;
#22908 = VECTOR ( 'NONE', #15516, 1000.000000000000227 ) ;
#22909 = VECTOR ( 'NONE', #43931, 1000.000000000000227 ) ;
#22910 = FACE_OUTER_BOUND ( 'NONE', #1585, .T. ) ;
#22911 = LINE ( 'NONE', #26075, #30361 ) ;
#22912 = DIRECTION ( 'NONE',  ( 0.005961354470445682716, -0.6427876096865404731, -0.7660212471507180654 ) ) ;
#22913 = CARTESIAN_POINT ( 'NONE',  ( 2.072287782118878319, 0.000000000000000000, -2.950529333540147015 ) ) ;
#22914 = ORIENTED_EDGE ( 'NONE', *, *, #22612, .F. ) ;
#22915 = CARTESIAN_POINT ( 'NONE',  ( -19.62661949931887762, 2.364828787826911416, 7.115266020801516156 ) ) ;
#22916 = ORIENTED_EDGE ( 'NONE', *, *, #53723, .F. ) ;
#22917 = ADVANCED_FACE ( 'NONE', ( #4116 ), #56084, .F. ) ;
#22918 = LINE ( 'NONE', #777, #3883 ) ;
#22919 = CARTESIAN_POINT ( 'NONE',  ( -31.72782227498118601, 0.000000000000000000, 9.205484770164058972 ) ) ;
#22920 = FACE_OUTER_BOUND ( 'NONE', #35811, .T. ) ;
#22921 = AXIS2_PLACEMENT_3D ( 'NONE', #51546, #11532, #24556 ) ;
#22922 = DIRECTION ( 'NONE',  ( -0.5364919789714478471, 0.6444004775717705469, -0.5449076811759709926 ) ) ;
#22923 = LINE ( 'NONE', #14970, #17776 ) ;
#22924 = ADVANCED_FACE ( 'NONE', ( #4950 ), #26247, .F. ) ;
#22925 = CARTESIAN_POINT ( 'NONE',  ( -71.02048890987401819, -1.000000000000000000, 8.554889286408840832 ) ) ;
#22926 = ORIENTED_EDGE ( 'NONE', *, *, #52415, .T. ) ;
#22927 = FACE_OUTER_BOUND ( 'NONE', #49894, .T. ) ;
#22928 = CARTESIAN_POINT ( 'NONE',  ( -20.58814680246558027, 3.200641362704007786, 10.13125426308755372 ) ) ;
#22929 = FACE_OUTER_BOUND ( 'NONE', #6916, .T. ) ;
#22930 = AXIS2_PLACEMENT_3D ( 'NONE', #27216, #32038, #44520 ) ;
#22931 = CARTESIAN_POINT ( 'NONE',  ( -68.61431715373868201, 1.786464687300608922, -7.472022508502793592 ) ) ;
#22932 = CARTESIAN_POINT ( 'NONE',  ( -15.55273877566505369, 0.000000000000000000, 6.746038521431690249 ) ) ;
#22933 = VECTOR ( 'NONE', #30119, 1000.000000000000227 ) ;
#22934 = CARTESIAN_POINT ( 'NONE',  ( -9.853328413990368517, -0.1191753592594190225, 3.735733064162294781 ) ) ;
#22935 = CARTESIAN_POINT ( 'NONE',  ( -27.34714091995699548, 16.86939667417711775, 4.665742070404716557 ) ) ;
#22936 = CARTESIAN_POINT ( 'NONE',  ( -23.25534986176962704, 19.16669654271327161, 4.483237965442247841 ) ) ;
#22937 = AXIS2_PLACEMENT_3D ( 'NONE', #55080, #19863, #28954 ) ;
#22938 = CARTESIAN_POINT ( 'NONE',  ( -16.46608590270481187, 0.000000000000000000, 4.692264237644060643 ) ) ;
#22939 = VECTOR ( 'NONE', #21488, 1000.000000000000227 ) ;
#22940 = AXIS2_PLACEMENT_3D ( 'NONE', #29180, #50506, #24368 ) ;
#22941 = EDGE_LOOP ( 'NONE', ( #54248, #52490, #46064, #52493, #49178 ) ) ;
#22942 = EDGE_CURVE ( 'NONE', #2673, #40139, #25991, .T. ) ;
#22943 = AXIS2_PLACEMENT_3D ( 'NONE', #48355, #9464, #44114 ) ;
#22944 = EDGE_LOOP ( 'NONE', ( #50873, #52506, #22688, #53742, #5525 ) ) ;
#22945 = ORIENTED_EDGE ( 'NONE', *, *, #29322, .T. ) ;
#22946 = AXIS2_PLACEMENT_3D ( 'NONE', #24718, #25028, #24187 ) ;
#22947 = ORIENTED_EDGE ( 'NONE', *, *, #26273, .F. ) ;
#22948 = ORIENTED_EDGE ( 'NONE', *, *, #53604, .T. ) ;
#22949 = DIRECTION ( 'NONE',  ( -0.7660212471507179544, -0.6427876096865405842, -0.005961354470445141482 ) ) ;
#22950 = DIRECTION ( 'NONE',  ( 0.005002170337468016433, -0.7660444431189770143, -0.6427681459581293666 ) ) ;
#22951 = EDGE_CURVE ( 'NONE', #15779, #15067, #21975, .T. ) ;
#22952 = EDGE_LOOP ( 'NONE', ( #25426, #7651, #26408, #35672 ) ) ;
#22953 = ORIENTED_EDGE ( 'NONE', *, *, #26249, .F. ) ;
#22954 = VECTOR ( 'NONE', #20929, 1000.000000000000227 ) ;
#22955 = ORIENTED_EDGE ( 'NONE', *, *, #5, .T. ) ;
#22956 = VECTOR ( 'NONE', #28838, 999.9999999999998863 ) ;
#22957 = EDGE_CURVE ( 'NONE', #45114, #34742, #39306, .T. ) ;
#22958 = CARTESIAN_POINT ( 'NONE',  ( -67.75126421527782838, -8.858758211978919661, -5.285932311690691776 ) ) ;
#22959 = DIRECTION ( 'NONE',  ( -0.5449076811759708816, 0.6444004775717707689, 0.5364919789714475140 ) ) ;
#22960 = DIRECTION ( 'NONE',  ( 0.005002170337468016433, -0.7660444431189770143, -0.6427681459581293666 ) ) ;
#22961 = EDGE_LOOP ( 'NONE', ( #13584, #30362, #12434, #25718 ) ) ;
#22962 = LINE ( 'NONE', #48527, #46402 ) ;
#22963 = VECTOR ( 'NONE', #40717, 1000.000000000000227 ) ;
#22964 = ORIENTED_EDGE ( 'NONE', *, *, #49549, .T. ) ;
#22965 = LINE ( 'NONE', #1662, #39113 ) ;
#22966 = EDGE_CURVE ( 'NONE', #18488, #53403, #8361, .T. ) ;
#22968 = VECTOR ( 'NONE', #12143, 1000.000000000000227 ) ;
#22967 = LINE ( 'NONE', #14457, #22112 ) ;
#22969 = EDGE_CURVE ( 'NONE', #21477, #29224, #38769, .T. ) ;
#22970 = DIRECTION ( 'NONE',  ( -0.5364919789714478471, 0.6444004775717705469, -0.5449076811759709926 ) ) ;
#22971 = DIRECTION ( 'NONE',  ( -0.005961354470445682716, -0.6427876096865404731, 0.7660212471507180654 ) ) ;
#22972 = DIRECTION ( 'NONE',  ( -0.5449076811759708816, 0.6444004775717707689, 0.5364919789714475140 ) ) ;
#22973 = CARTESIAN_POINT ( 'NONE',  ( -13.31992531437080274, -5.375054281893166142, 1.883740082759787882 ) ) ;
#22974 = DIRECTION ( 'NONE',  ( -0.2588190451025176864, -0.9659258262890692004, 0.000000000000000000 ) ) ;
#22975 = VECTOR ( 'NONE', #35890, 1000.000000000000114 ) ;
#22976 = ORIENTED_EDGE ( 'NONE', *, *, #23710, .T. ) ;
#22977 = FACE_OUTER_BOUND ( 'NONE', #1598, .T. ) ;
#22978 = ORIENTED_EDGE ( 'NONE', *, *, #32427, .F. ) ;
#22979 = AXIS2_PLACEMENT_3D ( 'NONE', #30165, #16837, #21910 ) ;
#22980 = ADVANCED_FACE ( 'NONE', ( #52084 ), #12633, .F. ) ;
#22981 = VECTOR ( 'NONE', #46730, 1000.000000000000114 ) ;
#22982 = CARTESIAN_POINT ( 'NONE',  ( -11.99778742911683871, 1.905425754524007642, 1.281486757967683632 ) ) ;
#22983 = DIRECTION ( 'NONE',  ( 0.007781995580012663651, -3.146120232559066537E-19, -0.9999697198139514409 ) ) ;
#22984 = CARTESIAN_POINT ( 'NONE',  ( -20.69764258542294399, 20.51603762622111304, 4.338448882013300256 ) ) ;
#22985 = CARTESIAN_POINT ( 'NONE',  ( -10.00813838035478298, 0.000000000000000000, 10.77830692922518452 ) ) ;
#22986 = FACE_OUTER_BOUND ( 'NONE', #49724, .T. ) ;
#22987 = LINE ( 'NONE', #1680, #49411 ) ;
#22988 = CARTESIAN_POINT ( 'NONE',  ( -11.88054826722768276, 25.79903810567671130, 5.000000000000000000 ) ) ;
#22989 = ADVANCED_FACE ( 'NONE', ( #9202 ), #5249, .F. ) ;
#22990 = VECTOR ( 'NONE', #2546, 1000.000000000000227 ) ;
#22991 = FACE_OUTER_BOUND ( 'NONE', #21592, .T. ) ;
#22992 = VECTOR ( 'NONE', #53332, 999.9999999999998863 ) ;
#22993 = CARTESIAN_POINT ( 'NONE',  ( -30.79411802867772607, 0.000000000000000000, 8.643412946479525516 ) ) ;
#22994 = VERTEX_POINT ( 'NONE', #29950 ) ;
#22995 = PLANE ( 'NONE',  #45673 ) ;
#22996 = DIRECTION ( 'NONE',  ( 0.007781995580012662783, 0.000000000000000000, -0.9999697198139514409 ) ) ;
#22997 = CARTESIAN_POINT ( 'NONE',  ( -68.93342745996714882, -0.9999999999999983347, -5.847034362371242189 ) ) ;
#22998 = DIRECTION ( 'NONE',  ( 0.6427681459581294776, -0.7660444431189769032, 0.005002170337467562802 ) ) ;
#22999 = DIRECTION ( 'NONE',  ( 0.5449076811759707706, 0.6444004775717708799, -0.5364919789714476250 ) ) ;
#23000 = DIRECTION ( 'NONE',  ( 0.5364919789714477361, 0.6444004775717706579, 0.5449076811759711036 ) ) ;
#23001 = FACE_OUTER_BOUND ( 'NONE', #41045, .T. ) ;
#23002 = ORIENTED_EDGE ( 'NONE', *, *, #55489, .F. ) ;
#23003 = ORIENTED_EDGE ( 'NONE', *, *, #45150, .F. ) ;
#23004 = AXIS2_PLACEMENT_3D ( 'NONE', #5434, #877, #5705 ) ;
#23005 = CARTESIAN_POINT ( 'NONE',  ( -23.33693525117809386, 0.000000000000000000, 5.746789908705562944 ) ) ;
#23006 = PLANE ( 'NONE',  #41334 ) ;
#23007 = VECTOR ( 'NONE', #51607, 1000.000000000000227 ) ;
#23008 = VERTEX_POINT ( 'NONE', #17170 ) ;
#23009 = DIRECTION ( 'NONE',  ( 0.005002170337468016433, -0.7660444431189770143, -0.6427681459581293666 ) ) ;
#23010 = ADVANCED_FACE ( 'NONE', ( #39867 ), #18013, .F. ) ;
#23011 = AXIS2_PLACEMENT_3D ( 'NONE', #40799, #23739, #19486 ) ;
#23012 = ORIENTED_EDGE ( 'NONE', *, *, #54140, .T. ) ;
#23013 = DIRECTION ( 'NONE',  ( -0.5364919789714478471, 0.6444004775717705469, -0.5449076811759709926 ) ) ;
#23014 = ORIENTED_EDGE ( 'NONE', *, *, #55147, .T. ) ;
#23015 = ORIENTED_EDGE ( 'NONE', *, *, #31360, .T. ) ;
#23016 = EDGE_CURVE ( 'NONE', #5857, #44275, #30534, .T. ) ;
#23017 = VERTEX_POINT ( 'NONE', #12903 ) ;
#23018 = ADVANCED_FACE ( 'NONE', ( #30233 ), #47548, .F. ) ;
#23019 = CARTESIAN_POINT ( 'NONE',  ( -27.06552663992790997, 0.000000000000000000, 7.195101427592543786 ) ) ;
#23020 = VECTOR ( 'NONE', #43745, 1000.000000000000000 ) ;
#23021 = DIRECTION ( 'NONE',  ( 0.000000000000000000, -1.000000000000000000, 0.000000000000000000 ) ) ;
#23022 = DIRECTION ( 'NONE',  ( 0.9999697198139515519, 0.000000000000000000, 0.007781995580013368816 ) ) ;
#23023 = ADVANCED_FACE ( 'NONE', ( #24526 ), #14911, .F. ) ;
#23024 = ADVANCED_FACE ( 'NONE', ( #23441 ), #45026, .F. ) ;
#23025 = EDGE_CURVE ( 'NONE', #3658, #7825, #14624, .T. ) ;
#23026 = AXIS2_PLACEMENT_3D ( 'NONE', #52248, #4810, #44287 ) ;
#23027 = PLANE ( 'NONE',  #275 ) ;
#23028 = ORIENTED_EDGE ( 'NONE', *, *, #39942, .T. ) ;
#23029 = EDGE_LOOP ( 'NONE', ( #55988, #47345, #55720, #49162, #51692 ) ) ;
#23030 = AXIS2_PLACEMENT_3D ( 'NONE', #12751, #12186, #21571 ) ;
#23031 = AXIS2_PLACEMENT_3D ( 'NONE', #45536, #23686, #10912 ) ;
#23032 = FACE_OUTER_BOUND ( 'NONE', #45236, .T. ) ;
#23033 = VERTEX_POINT ( 'NONE', #45289 ) ;
#23034 = CARTESIAN_POINT ( 'NONE',  ( -3.487307141772567842, 4.852350322572148933, -1.863785052350299232 ) ) ;
#23035 = ORIENTED_EDGE ( 'NONE', *, *, #37999, .T. ) ;
#23036 = DIRECTION ( 'NONE',  ( 0.005002170337468016433, -0.7660444431189770143, -0.6427681459581293666 ) ) ;
#23037 = CARTESIAN_POINT ( 'NONE',  ( -11.67244013076689946, 0.000000000000000000, 11.50401908778467863 ) ) ;
#23038 = VERTEX_POINT ( 'NONE', #15205 ) ;
#23039 = CARTESIAN_POINT ( 'NONE',  ( -17.74560456716937296, 0.000000000000000000, 3.774316574337878372 ) ) ;
#23040 = EDGE_CURVE ( 'NONE', #43429, #3658, #34524, .T. ) ;
#23041 = ORIENTED_EDGE ( 'NONE', *, *, #18197, .T. ) ;
#23042 = ADVANCED_FACE ( 'NONE', ( #32520 ), #23692, .F. ) ;
#23043 = CARTESIAN_POINT ( 'NONE',  ( -9.442067484779661513, -0.1191753592594197858, 10.59804618892231254 ) ) ;
#23044 = AXIS2_PLACEMENT_3D ( 'NONE', #43819, #14315, #5485 ) ;
#23045 = ORIENTED_EDGE ( 'NONE', *, *, #51653, .F. ) ;
#23046 = CARTESIAN_POINT ( 'NONE',  ( -13.94003342103131082, 0.000000000000000000, 4.342590492342347730 ) ) ;
#23047 = DIRECTION ( 'NONE',  ( -0.5364919789714478471, 0.6444004775717705469, -0.5449076811759709926 ) ) ;
#23048 = ADVANCED_FACE ( 'NONE', ( #33065 ), #40758, .F. ) ;
#23049 = CARTESIAN_POINT ( 'NONE',  ( -25.20200914511100265, -0.1191753592594197858, 6.570942640130446932 ) ) ;
#23050 = ORIENTED_EDGE ( 'NONE', *, *, #52503, .T. ) ;
#23051 = AXIS2_PLACEMENT_3D ( 'NONE', #1244, #26827, #13749 ) ;
#23052 = EDGE_CURVE ( 'NONE', #40111, #39737, #46119, .T. ) ;
#23053 = CARTESIAN_POINT ( 'NONE',  ( -10.74029228357944987, 0.000000000000000000, 11.14194120806293320 ) ) ;
#23054 = CARTESIAN_POINT ( 'NONE',  ( -23.33693525117809386, 0.000000000000000000, 5.746789908705562944 ) ) ;
#23055 = AXIS2_PLACEMENT_3D ( 'NONE', #1606, #39932, #18931 ) ;
#23056 = CYLINDRICAL_SURFACE ( 'NONE', #20496, 0.5000000000000004441 ) ;
#23057 = CARTESIAN_POINT ( 'NONE',  ( -12.80458192191714595, 0.000000000000000000, 11.86454056839041726 ) ) ;
#23058 = CARTESIAN_POINT ( 'NONE',  ( -14.05150990151598656, -1.813211359398158029, 2.281553818646722132 ) ) ;
#23059 = CARTESIAN_POINT ( 'NONE',  ( -67.99914138734528990, -9.626105528482602480, -5.294842188089768698 ) ) ;
#23060 = ORIENTED_EDGE ( 'NONE', *, *, #55863, .T. ) ;
#23061 = DIRECTION ( 'NONE',  ( -0.5449076811759708816, 0.6444004775717707689, 0.5364919789714475140 ) ) ;
#23062 = DIRECTION ( 'NONE',  ( 0.5449076811759707706, 0.6444004775717708799, -0.5364919789714476250 ) ) ;
#23063 = CARTESIAN_POINT ( 'NONE',  ( -67.02267797893095747, -0.6010035547808885159, -0.3415480826665019953 ) ) ;
#23064 = ORIENTED_EDGE ( 'NONE', *, *, #48838, .T. ) ;
#23065 = VECTOR ( 'NONE', #24606, 1000.000000000000227 ) ;
#23066 = DIRECTION ( 'NONE',  ( -0.5364919789714478471, 0.6444004775717705469, -0.5449076811759709926 ) ) ;
#23067 = DIRECTION ( 'NONE',  ( 0.9999697198139515519, 0.000000000000000000, 0.007781995580013368816 ) ) ;
#23068 = EDGE_LOOP ( 'NONE', ( #26599, #44208, #17271, #45243 ) ) ;
#23069 = AXIS2_PLACEMENT_3D ( 'NONE', #4606, #47491, #34432 ) ;
#23070 = DIRECTION ( 'NONE',  ( -0.5364919789714478471, 0.6444004775717705469, -0.5449076811759709926 ) ) ;
#23071 = CARTESIAN_POINT ( 'NONE',  ( -15.40103151951671734, 0.000000000000000000, 12.95233060667165681 ) ) ;
#23072 = FACE_OUTER_BOUND ( 'NONE', #17002, .T. ) ;
#23073 = ORIENTED_EDGE ( 'NONE', *, *, #45403, .F. ) ;
#23074 = VECTOR ( 'NONE', #50985, 999.9999999999998863 ) ;
#23075 = VECTOR ( 'NONE', #2696, 999.9999999999998863 ) ;
#23076 = ORIENTED_EDGE ( 'NONE', *, *, #44348, .F. ) ;
#23077 = DIRECTION ( 'NONE',  ( -1.000000000000000000, -0.000000000000000000, -0.000000000000000000 ) ) ;
#23078 = CARTESIAN_POINT ( 'NONE',  ( -66.07241458602462103, 2.000000000000034195, -4.498572511313228439 ) ) ;
#23079 = DIRECTION ( 'NONE',  ( 0.007781995580012662783, 0.000000000000000000, -0.9999697198139514409 ) ) ;
#23080 = LINE ( 'NONE', #919, #11046 ) ;
#23081 = EDGE_LOOP ( 'NONE', ( #12557, #33987, #3265, #43231, #46934, #39808, #38089, #7445 ) ) ;
#23082 = DIRECTION ( 'NONE',  ( -0.6427681459581293666, -0.7660444431189770143, -0.005002170337467561935 ) ) ;
#23083 = ORIENTED_EDGE ( 'NONE', *, *, #41030, .T. ) ;
#23084 = CARTESIAN_POINT ( 'NONE',  ( -25.20278734466900517, 0.000000000000000000, 6.670939612111840944 ) ) ;
#23085 = VECTOR ( 'NONE', #5032, 1000.000000000000227 ) ;
#23086 = CARTESIAN_POINT ( 'NONE',  ( -61.70068505767310540, 8.059153983834628221, 5.000000000000000000 ) ) ;
#23087 = ORIENTED_EDGE ( 'NONE', *, *, #11682, .T. ) ;
#23088 = AXIS2_PLACEMENT_3D ( 'NONE', #34684, #52007, #13120 ) ;
#23089 = CARTESIAN_POINT ( 'NONE',  ( -17.86861875374391317, 0.000000000000000000, 5.789345612113324435 ) ) ;
#23090 = DIRECTION ( 'NONE',  ( 0.5449076811759707706, 0.6444004775717708799, -0.5364919789714476250 ) ) ;
#23091 = VECTOR ( 'NONE', #27297, 1000.000000000000000 ) ;
#23092 = DIRECTION ( 'NONE',  ( 0.007781995580012663651, 0.000000000000000000, -0.9999697198139515519 ) ) ;
#23093 = EDGE_CURVE ( 'NONE', #28121, #20361, #45546, .T. ) ;
#23094 = ADVANCED_FACE ( 'NONE', ( #50083 ), #49565, .F. ) ;
#23095 = VERTEX_POINT ( 'NONE', #24273 ) ;
#23096 = DIRECTION ( 'NONE',  ( -0.6427681459581293666, -0.7660444431189770143, -0.005002170337467561935 ) ) ;
#23097 = VERTEX_POINT ( 'NONE', #10675 ) ;
#23098 = ADVANCED_FACE ( 'NONE', ( #19150 ), #36478, .F. ) ;
#23099 = ORIENTED_EDGE ( 'NONE', *, *, #12370, .T. ) ;
#23100 = EDGE_LOOP ( 'NONE', ( #19030, #4840, #37123, #48237 ) ) ;
#23101 = CARTESIAN_POINT ( 'NONE',  ( -25.20200914511100265, -0.1191753592594197858, 6.570942640130446932 ) ) ;
#23102 = VECTOR ( 'NONE', #53563, 1000.000000000000227 ) ;
#23103 = ORIENTED_EDGE ( 'NONE', *, *, #17610, .F. ) ;
#23104 = VECTOR ( 'NONE', #5308, 999.9999999999998863 ) ;
#23105 = LINE ( 'NONE', #27937, #42034 ) ;
#23106 = ORIENTED_EDGE ( 'NONE', *, *, #35208, .T. ) ;
#23107 = DIRECTION ( 'NONE',  ( 0.000000000000000000, -1.000000000000000000, 0.000000000000000000 ) ) ;
#23108 = DIRECTION ( 'NONE',  ( -0.005002170337468016433, -0.7660444431189770143, 0.6427681459581293666 ) ) ;
#23109 = VECTOR ( 'NONE', #35288, 1000.000000000000227 ) ;
#23110 = ORIENTED_EDGE ( 'NONE', *, *, #50301, .T. ) ;
#23111 = DIRECTION ( 'NONE',  ( 0.7660212471507180654, -0.6427876096865404731, 0.005961354470445141482 ) ) ;
#23112 = ORIENTED_EDGE ( 'NONE', *, *, #28594, .F. ) ;
#23113 = ADVANCED_FACE ( 'NONE', ( #41015 ), #28818, .F. ) ;
#23114 = VECTOR ( 'NONE', #34207, 1000.000000000000227 ) ;
#23115 = DIRECTION ( 'NONE',  ( 0.005961354470445682716, -0.6427876096865404731, -0.7660212471507180654 ) ) ;
#23116 = VECTOR ( 'NONE', #43574, 1000.000000000000227 ) ;
#23117 = FACE_OUTER_BOUND ( 'NONE', #6914, .T. ) ;
#23118 = DIRECTION ( 'NONE',  ( -0.7660212471507179544, -0.6427876096865405842, -0.005961354470445141482 ) ) ;
#23119 = DIRECTION ( 'NONE',  ( 0.000000000000000000, -1.000000000000000000, 0.000000000000000000 ) ) ;
#23120 = EDGE_CURVE ( 'NONE', #28250, #9132, #54618, .T. ) ;
#23121 = CARTESIAN_POINT ( 'NONE',  ( -14.98157860027400723, -0.1191753592594192307, 5.911816254260776837 ) ) ;
#23122 = CARTESIAN_POINT ( 'NONE',  ( 2.072287782118878319, 0.000000000000000000, -2.950529333540147015 ) ) ;
#23123 = PLANE ( 'NONE',  #24681 ) ;
#23124 = EDGE_LOOP ( 'NONE', ( #14644, #36496, #1974 ) ) ;
#23126 = ORIENTED_EDGE ( 'NONE', *, *, #5169, .F. ) ;
#23125 = ADVANCED_FACE ( 'NONE', ( #28518 ), #53521, .F. ) ;
#23127 = CARTESIAN_POINT ( 'NONE',  ( -13.19350925028023092, 0.000000000000000000, 2.132407697215775499 ) ) ;
#23128 = DIRECTION ( 'NONE',  ( -0.005002170337468016433, -0.7660444431189770143, 0.6427681459581293666 ) ) ;
#23129 = EDGE_CURVE ( 'NONE', #39009, #21187, #42687, .T. ) ;
#23130 = LINE ( 'NONE', #8959, #21538 ) ;
#23131 = AXIS2_PLACEMENT_3D ( 'NONE', #32378, #36914, #1688 ) ;
#23132 = FACE_OUTER_BOUND ( 'NONE', #53242, .T. ) ;
#23133 = VERTEX_POINT ( 'NONE', #29675 ) ;
#23134 = AXIS2_PLACEMENT_3D ( 'NONE', #11221, #33093, #49590 ) ;
#23135 = DIRECTION ( 'NONE',  ( 0.007781995580012663651, -3.146120232559066537E-19, -0.9999697198139514409 ) ) ;
#23136 = LINE ( 'NONE', #52943, #25041 ) ;
#23137 = ORIENTED_EDGE ( 'NONE', *, *, #31764, .F. ) ;
#23138 = LINE ( 'NONE', #44418, #27516 ) ;
#23139 = CARTESIAN_POINT ( 'NONE',  ( -16.02950353879027645, 2.229229656569005957, 6.766270303596409796 ) ) ;
#23140 = VECTOR ( 'NONE', #31923, 1000.000000000000227 ) ;
#23141 = EDGE_LOOP ( 'NONE', ( #12014, #49487, #41779, #12869 ) ) ;
#23142 = CARTESIAN_POINT ( 'NONE',  ( -68.33899556999409697, -8.925864846846893741, -6.396357082918144421 ) ) ;
#23143 = CARTESIAN_POINT ( 'NONE',  ( -30.79489622823572859, -0.1191753592594197858, 8.743409918460921304 ) ) ;
#23144 = VECTOR ( 'NONE', #35836, 999.9999999999998863 ) ;
#23145 = DIRECTION ( 'NONE',  ( 0.5449076811759707706, 0.6444004775717708799, -0.5364919789714476250 ) ) ;
#23146 = DIRECTION ( 'NONE',  ( 0.7660212471507180654, -0.6427876096865404731, 0.005961354470445141482 ) ) ;
#23147 = DIRECTION ( 'NONE',  ( -0.9999697198139514409, -0.000000000000000000, -0.007781995580013368816 ) ) ;
#23148 = ORIENTED_EDGE ( 'NONE', *, *, #20410, .T. ) ;
#23149 = VECTOR ( 'NONE', #5784, 1000.000000000000227 ) ;
#23150 = AXIS2_PLACEMENT_3D ( 'NONE', #16009, #8308, #42409 ) ;
#23151 = VERTEX_POINT ( 'NONE', #50920 ) ;
#23152 = VECTOR ( 'NONE', #21983, 999.9999999999998863 ) ;
#23153 = PLANE ( 'NONE',  #15756 ) ;
#23154 = PLANE ( 'NONE',  #51251 ) ;
#23155 = DIRECTION ( 'NONE',  ( -0.005961354470445682716, -0.6427876096865404731, 0.7660212471507180654 ) ) ;
#23156 = AXIS2_PLACEMENT_3D ( 'NONE', #35424, #39958, #52727 ) ;
#23157 = DIRECTION ( 'NONE',  ( 0.005002170337468016433, -0.7660444431189770143, -0.6427681459581293666 ) ) ;
#23158 = CARTESIAN_POINT ( 'NONE',  ( -23.33849165029409889, 0.000000000000000000, 5.946783852668351855 ) ) ;
#23159 = ORIENTED_EDGE ( 'NONE', *, *, #36568, .T. ) ;
#23160 = CARTESIAN_POINT ( 'NONE',  ( -16.20482545075801895, 23.30241550971489772, -3.967651922502964723 ) ) ;
#23161 = PLANE ( 'NONE',  #6646 ) ;
#23162 = VECTOR ( 'NONE', #19597, 1000.000000000000000 ) ;
#23163 = DIRECTION ( 'NONE',  ( 0.005002170337468016433, -0.7660444431189770143, -0.6427681459581293666 ) ) ;
#23164 = VECTOR ( 'NONE', #23062, 1000.000000000000114 ) ;
#23165 = CARTESIAN_POINT ( 'NONE',  ( -20.57714959317112147, 20.77805298910839582, -4.325263209797152619 ) ) ;
#23166 = ORIENTED_EDGE ( 'NONE', *, *, #12536, .T. ) ;
#23167 = PLANE ( 'NONE',  #19286 ) ;
#23168 = ORIENTED_EDGE ( 'NONE', *, *, #37301, .F. ) ;
#23169 = DIRECTION ( 'NONE',  ( 0.005002170337468016433, -0.7660444431189770143, -0.6427681459581293666 ) ) ;
#23170 = DIRECTION ( 'NONE',  ( -0.5364919789714478471, 0.6444004775717705469, -0.5449076811759709926 ) ) ;
#23171 = EDGE_CURVE ( 'NONE', #8281, #29778, #29362, .T. ) ;
#23172 = ORIENTED_EDGE ( 'NONE', *, *, #45436, .T. ) ;
#23173 = DIRECTION ( 'NONE',  ( -0.7660212471507179544, -0.6427876096865405842, -0.005961354470445141482 ) ) ;
#23174 = EDGE_LOOP ( 'NONE', ( #13112, #26238, #13640, #45610 ) ) ;
#23175 = ADVANCED_FACE ( 'NONE', ( #56059 ), #16878, .F. ) ;
#23176 = EDGE_CURVE ( 'NONE', #50963, #51710, #37896, .T. ) ;
#23177 = AXIS2_PLACEMENT_3D ( 'NONE', #12088, #2715, #50719 ) ;
#23178 = ORIENTED_EDGE ( 'NONE', *, *, #24800, .F. ) ;
#23179 = ORIENTED_EDGE ( 'NONE', *, *, #45591, .F. ) ;
#23180 = LINE ( 'NONE', #657, #23908 ) ;
#23181 = ORIENTED_EDGE ( 'NONE', *, *, #12478, .T. ) ;
#23182 = VECTOR ( 'NONE', #17430, 1000.000000000000227 ) ;
#23183 = ORIENTED_EDGE ( 'NONE', *, *, #30669, .T. ) ;
#23184 = CARTESIAN_POINT ( 'NONE',  ( -24.27063949748155380, 0.000000000000000000, 6.308861732390097288 ) ) ;
#23185 = LINE ( 'NONE', #31969, #14071 ) ;
#23186 = VECTOR ( 'NONE', #29652, 999.9999999999998863 ) ;
#23187 = EDGE_LOOP ( 'NONE', ( #42940, #33766, #15368, #49971 ) ) ;
#23188 = ORIENTED_EDGE ( 'NONE', *, *, #7532, .T. ) ;
#23189 = CARTESIAN_POINT ( 'NONE',  ( -27.06708303904391144, 0.000000000000000000, 7.395095371555332697 ) ) ;
#23190 = ORIENTED_EDGE ( 'NONE', *, *, #42118, .T. ) ;
#23191 = VECTOR ( 'NONE', #7065, 999.9999999999998863 ) ;
#23192 = ORIENTED_EDGE ( 'NONE', *, *, #6086, .F. ) ;
#23193 = VECTOR ( 'NONE', #5502, 999.9999999999998863 ) ;
#23194 = AXIS2_PLACEMENT_3D ( 'NONE', #8531, #47140, #30402 ) ;
#23195 = CARTESIAN_POINT ( 'NONE',  ( -16.81619947299561701, 3.200641362704010007, 3.111797470672864829 ) ) ;
#23196 = DIRECTION ( 'NONE',  ( 0.000000000000000000, 1.000000000000000000, 0.000000000000000000 ) ) ;
#23197 = PLANE ( 'NONE',  #26001 ) ;
#23198 = FACE_OUTER_BOUND ( 'NONE', #49941, .T. ) ;
#23199 = ORIENTED_EDGE ( 'NONE', *, *, #54367, .T. ) ;
#23200 = CARTESIAN_POINT ( 'NONE',  ( -14.20280369269832832, 0.000000000000000000, 12.40765738797303719 ) ) ;
#23201 = ORIENTED_EDGE ( 'NONE', *, *, #3131, .F. ) ;
#23202 = VECTOR ( 'NONE', #41437, 999.9999999999998863 ) ;
#23203 = AXIS2_PLACEMENT_3D ( 'NONE', #16240, #11964, #25066 ) ;
#23204 = VECTOR ( 'NONE', #9305, 999.9999999999998863 ) ;
#23205 = DIRECTION ( 'NONE',  ( 0.005961354470445682716, -0.6427876096865404731, -0.7660212471507180654 ) ) ;
#23206 = EDGE_CURVE ( 'NONE', #34036, #26165, #3787, .T. ) ;
#23207 = DIRECTION ( 'NONE',  ( 0.007781995580012662783, 0.000000000000000000, -0.9999697198139514409 ) ) ;
#23208 = VECTOR ( 'NONE', #39416, 999.9999999999998863 ) ;
#23209 = CARTESIAN_POINT ( 'NONE',  ( -69.02562660986798448, 0.1329415388989311775, 6.116987600435763284 ) ) ;
#23210 = CARTESIAN_POINT ( 'NONE',  ( -10.87894692659065221, 0.000000000000000000, 3.258416365829116312 ) ) ;
#23211 = ADVANCED_FACE ( 'NONE', ( #16036 ), #51222, .F. ) ;
#23212 = CARTESIAN_POINT ( 'NONE',  ( -14.94838282604900748, -0.1191753592594197858, 2.588085963191248506 ) ) ;
#23213 = LINE ( 'NONE', #31993, #40402 ) ;
#23214 = ORIENTED_EDGE ( 'NONE', *, *, #12341, .F. ) ;
#23215 = FACE_OUTER_BOUND ( 'NONE', #12393, .T. ) ;
#23216 = EDGE_CURVE ( 'NONE', #35486, #26049, #38436, .T. ) ;
#23217 = ORIENTED_EDGE ( 'NONE', *, *, #33534, .F. ) ;
#23218 = DIRECTION ( 'NONE',  ( 0.000000000000000000, 0.000000000000000000, -1.000000000000000000 ) ) ;
#23219 = CARTESIAN_POINT ( 'NONE',  ( 0.3240706152708105470, -3.670543518250628079, -2.125000000000001332 ) ) ;
#23220 = DIRECTION ( 'NONE',  ( 0.5364919789714477361, 0.6444004775717706579, 0.5449076811759711036 ) ) ;
#23221 = EDGE_CURVE ( 'NONE', #27104, #22456, #39248, .T. ) ;
#23222 = CARTESIAN_POINT ( 'NONE',  ( -16.28621033327900136, 0.000000000000000000, 7.278988559564416150 ) ) ;
#23223 = FACE_OUTER_BOUND ( 'NONE', #37184, .T. ) ;
#23224 = AXIS2_PLACEMENT_3D ( 'NONE', #11687, #3157, #46048 ) ;
#23225 = CARTESIAN_POINT ( 'NONE',  ( -66.79270813916639327, 2.820013818116702216E-15, -3.456045872278595610 ) ) ;
#23226 = ORIENTED_EDGE ( 'NONE', *, *, #54015, .F. ) ;
#23227 = CARTESIAN_POINT ( 'NONE',  ( -39.55045063245202641, 8.091761719094847649, 5.000000000000000000 ) ) ;
#23228 = FACE_OUTER_BOUND ( 'NONE', #21639, .T. ) ;
#23229 = CARTESIAN_POINT ( 'NONE',  ( -16.43317633868556626, -0.1191753592594197858, 13.31363028683540151 ) ) ;
#23230 = VECTOR ( 'NONE', #36752, 999.9999999999998863 ) ;
#23231 = CARTESIAN_POINT ( 'NONE',  ( -67.79210531775262893, 2.000000000000010214, -7.454399636913916716 ) ) ;
#23232 = VECTOR ( 'NONE', #35479, 1000.000000000000114 ) ;
#23233 = LINE ( 'NONE', #4770, #6735 ) ;
#23234 = LINE ( 'NONE', #36856, #31983 ) ;
#23235 = VECTOR ( 'NONE', #18154, 999.9999999999998863 ) ;
#23236 = VECTOR ( 'NONE', #26519, 999.9999999999998863 ) ;
#23237 = LINE ( 'NONE', #32319, #5153 ) ;
#23238 = LINE ( 'NONE', #28305, #222 ) ;
#23239 = ADVANCED_FACE ( 'NONE', ( #51770 ), #42981, .F. ) ;
#23240 = VECTOR ( 'NONE', #43867, 999.9999999999998863 ) ;
#23241 = ORIENTED_EDGE ( 'NONE', *, *, #5581, .T. ) ;
#23242 = AXIS2_PLACEMENT_3D ( 'NONE', #482, #22366, #5875 ) ;
#23243 = EDGE_CURVE ( 'NONE', #15067, #34449, #51518, .T. ) ;
#23244 = AXIS2_PLACEMENT_3D ( 'NONE', #42066, #20505, #13648 ) ;
#23245 = ORIENTED_EDGE ( 'NONE', *, *, #30261, .F. ) ;
#23246 = VECTOR ( 'NONE', #13567, 999.9999999999998863 ) ;
#23247 = ORIENTED_EDGE ( 'NONE', *, *, #2956, .T. ) ;
#23248 = VERTEX_POINT ( 'NONE', #37603 ) ;
#23249 = VERTEX_POINT ( 'NONE', #3524 ) ;
#23250 = DIRECTION ( 'NONE',  ( -1.000000000000000000, 0.000000000000000000, 0.000000000000000000 ) ) ;
#23251 = PLANE ( 'NONE',  #54782 ) ;
#23252 = ORIENTED_EDGE ( 'NONE', *, *, #21624, .T. ) ;
#23253 = ORIENTED_EDGE ( 'NONE', *, *, #54210, .F. ) ;
#23254 = EDGE_LOOP ( 'NONE', ( #21207, #48528, #50401, #11364 ) ) ;
#23255 = AXIS2_PLACEMENT_3D ( 'NONE', #52423, #52675, #48728 ) ;
#23256 = EDGE_CURVE ( 'NONE', #12044, #38354, #42432, .T. ) ;
#23257 = LINE ( 'NONE', #23784, #5696 ) ;
#23258 = DIRECTION ( 'NONE',  ( 0.6427681459581294776, -0.7660444431189769032, 0.005002170337467562802 ) ) ;
#23259 = CARTESIAN_POINT ( 'NONE',  ( -13.69485363937393529, -2.460819163488158878, 6.040101447381037936 ) ) ;
#23260 = ORIENTED_EDGE ( 'NONE', *, *, #4619, .T. ) ;
#23261 = VECTOR ( 'NONE', #44357, 1000.000000000000000 ) ;
#23262 = LINE ( 'NONE', #53612, #15595 ) ;
#23263 = VERTEX_POINT ( 'NONE', #47522 ) ;
#23264 = DIRECTION ( 'NONE',  ( 0.007781995580012662783, 0.000000000000000000, -0.9999697198139514409 ) ) ;
#23265 = VECTOR ( 'NONE', #2788, 1000.000000000000114 ) ;
#23266 = CARTESIAN_POINT ( 'NONE',  ( -50.02554558092695913, 3.776013638374817294, 5.000000000000000000 ) ) ;
#23267 = DIRECTION ( 'NONE',  ( 0.9999697198139515519, 0.000000000000000000, 0.007781995580013368816 ) ) ;
#23268 = PLANE ( 'NONE',  #52342 ) ;
#23269 = VECTOR ( 'NONE', #778, 1000.000000000000227 ) ;
#23270 = CARTESIAN_POINT ( 'NONE',  ( -46.00906441860568918, 4.911362066797304138, 5.000000000000000000 ) ) ;
#23271 = LINE ( 'NONE', #36062, #34749 ) ;
#23272 = FACE_OUTER_BOUND ( 'NONE', #40767, .T. ) ;
#23273 = ORIENTED_EDGE ( 'NONE', *, *, #32280, .T. ) ;
#23274 = LINE ( 'NONE', #827, #51869 ) ;
#23275 = ORIENTED_EDGE ( 'NONE', *, *, #37958, .F. ) ;
#23276 = VECTOR ( 'NONE', #24300, 999.9999999999998863 ) ;
#23277 = LINE ( 'NONE', #31784, #8352 ) ;
#23278 = CARTESIAN_POINT ( 'NONE',  ( -16.05622515956926577, 1.743523803501507485, 2.863087317488263395 ) ) ;
#23279 = DIRECTION ( 'NONE',  ( 0.000000000000000000, -0.000000000000000000, -1.000000000000000000 ) ) ;
#23280 = DIRECTION ( 'NONE',  ( -0.7660212471507179544, -0.6427876096865405842, -0.005961354470445141482 ) ) ;
#23281 = EDGE_CURVE ( 'NONE', #17923, #904, #25965, .T. ) ;
#23282 = DIRECTION ( 'NONE',  ( -0.5364919789714478471, 0.6444004775717705469, -0.5449076811759709926 ) ) ;
#23283 = CARTESIAN_POINT ( 'NONE',  ( -10.70194541067012395, 0.000000000000000000, 6.214450391007236618 ) ) ;
#23284 = PLANE ( 'NONE',  #8028 ) ;
#23285 = VECTOR ( 'NONE', #45632, 1000.000000000000227 ) ;
#23286 = AXIS2_PLACEMENT_3D ( 'NONE', #50066, #37293, #15713 ) ;
#23287 = CARTESIAN_POINT ( 'NONE',  ( -17.10315536259745528, 0.7721120973665037690, 3.300743681568104826 ) ) ;
#23288 = CARTESIAN_POINT ( 'NONE',  ( -11.63054826722768453, 25.36602540378449433, 3.000000000000000000 ) ) ;
#23289 = VERTEX_POINT ( 'NONE', #29928 ) ;
#23290 = DIRECTION ( 'NONE',  ( -0.005002170337468016433, -0.7660444431189770143, 0.6427681459581293666 ) ) ;
#23291 = PLANE ( 'NONE',  #43065 ) ;
#23292 = DIRECTION ( 'NONE',  ( -0.005002170337468016433, -0.7660444431189770143, 0.6427681459581293666 ) ) ;
#23293 = CARTESIAN_POINT ( 'NONE',  ( -16.98837300675671713, 1.743523803501507485, 3.225165197210008383 ) ) ;
#23294 = EDGE_CURVE ( 'NONE', #9654, #9899, #8335, .T. ) ;
#23295 = DIRECTION ( 'NONE',  ( 0.007781995580012663651, 0.000000000000000000, -0.9999697198139515519 ) ) ;
#23296 = EDGE_CURVE ( 'NONE', #43832, #36287, #3245, .T. ) ;
#23297 = CARTESIAN_POINT ( 'NONE',  ( -62.23823698199103660, 6.658783344088824663, 5.000000000000000000 ) ) ;
#23298 = EDGE_CURVE ( 'NONE', #14383, #37255, #21420, .T. ) ;
#23299 = DIRECTION ( 'NONE',  ( -0.5364919789714478471, 0.6444004775717705469, -0.5449076811759709926 ) ) ;
#23300 = VECTOR ( 'NONE', #50922, 1000.000000000000000 ) ;
#23301 = VERTEX_POINT ( 'NONE', #46379 ) ;
#23302 = EDGE_LOOP ( 'NONE', ( #3864, #9274, #33500, #18553 ) ) ;
#23303 = CARTESIAN_POINT ( 'NONE',  ( -15.35981059310210739, 0.000000000000000000, 7.655530086358199426 ) ) ;
#23304 = PLANE ( 'NONE',  #3215 ) ;
#23305 = ADVANCED_FACE ( 'NONE', ( #20574 ), #33610, .F. ) ;
#23306 = ORIENTED_EDGE ( 'NONE', *, *, #30891, .F. ) ;
#23307 = ADVANCED_FACE ( 'NONE', ( #46973 ), #8075, .F. ) ;
#23308 = FACE_OUTER_BOUND ( 'NONE', #20604, .T. ) ;
#23309 = VECTOR ( 'NONE', #14696, 1000.000000000000000 ) ;
#23310 = ORIENTED_EDGE ( 'NONE', *, *, #8915, .T. ) ;
#23311 = DIRECTION ( 'NONE',  ( 0.6427681459581294776, -0.7660444431189769032, 0.005002170337467562802 ) ) ;
#23312 = EDGE_CURVE ( 'NONE', #37777, #8995, #35312, .T. ) ;
#23313 = VECTOR ( 'NONE', #5402, 999.9999999999998863 ) ;
#23314 = ORIENTED_EDGE ( 'NONE', *, *, #47082, .F. ) ;
#23315 = ORIENTED_EDGE ( 'NONE', *, *, #13963, .T. ) ;
#23316 = ORIENTED_EDGE ( 'NONE', *, *, #25966, .T. ) ;
#23317 = CARTESIAN_POINT ( 'NONE',  ( -19.60990026154428278, 0.000000000000000000, 4.498472333781370125 ) ) ;
#23318 = DIRECTION ( 'NONE',  ( 0.6427681459581294776, -0.7660444431189769032, 0.005002170337467562802 ) ) ;
#23319 = LINE ( 'NONE', #32403, #51183 ) ;
#23320 = EDGE_CURVE ( 'NONE', #37770, #36287, #13710, .T. ) ;
#23321 = AXIS2_PLACEMENT_3D ( 'NONE', #35760, #22971, #44830 ) ;
#23322 = DIRECTION ( 'NONE',  ( 0.005961354470445682716, -0.6427876096865404731, -0.7660212471507180654 ) ) ;
#23323 = ORIENTED_EDGE ( 'NONE', *, *, #25143, .T. ) ;
#23324 = ORIENTED_EDGE ( 'NONE', *, *, #52960, .F. ) ;
#23325 = EDGE_CURVE ( 'NONE', #48176, #20000, #44377, .T. ) ;
#23326 = VECTOR ( 'NONE', #14546, 999.9999999999998863 ) ;
#23327 = CARTESIAN_POINT ( 'NONE',  ( -23.33849165029409889, 0.000000000000000000, 5.946783852668351855 ) ) ;
#23328 = VERTEX_POINT ( 'NONE', #40112 ) ;
#23329 = DIRECTION ( 'NONE',  ( 0.7660212471507180654, -0.6427876096865404731, 0.005961354470445141482 ) ) ;
#23330 = ORIENTED_EDGE ( 'NONE', *, *, #20483, .T. ) ;
#23331 = CARTESIAN_POINT ( 'NONE',  ( -13.57042358871905385, -0.1191753592594186895, 3.706805770018217316 ) ) ;
#23332 = CARTESIAN_POINT ( 'NONE',  ( -67.50702643244157741, 2.000000000000000000, -7.448289400635801805 ) ) ;
#23333 = ORIENTED_EDGE ( 'NONE', *, *, #5881, .T. ) ;
#23334 = LINE ( 'NONE', #40649, #31332 ) ;
#23335 = EDGE_LOOP ( 'NONE', ( #38543, #27205, #23188, #47106 ) ) ;
#23336 = FACE_OUTER_BOUND ( 'NONE', #39547, .T. ) ;
#23337 = ORIENTED_EDGE ( 'NONE', *, *, #51364, .T. ) ;
#23338 = LINE ( 'NONE', #36959, #43958 ) ;
#23339 = DIRECTION ( 'NONE',  ( 0.5449076811759707706, 0.6444004775717708799, -0.5364919789714476250 ) ) ;
#23340 = DIRECTION ( 'NONE',  ( -0.5364919789714478471, 0.6444004775717705469, -0.5449076811759709926 ) ) ;
#23341 = ORIENTED_EDGE ( 'NONE', *, *, #32491, .F. ) ;
#23342 = CARTESIAN_POINT ( 'NONE',  ( -1.753914626039396296, 5.922546351860411562, 3.899653579608918896 ) ) ;
#23343 = DIRECTION ( 'NONE',  ( -0.005002170337468016433, -0.7660444431189770143, 0.6427681459581293666 ) ) ;
#23344 = CARTESIAN_POINT ( 'NONE',  ( -69.22403449346161608, 1.440755222218420117, 7.485090880804399660 ) ) ;
#23345 = ADVANCED_FACE ( 'NONE', ( #48072 ), #53204, .F. ) ;
#23346 = DIRECTION ( 'NONE',  ( 0.000000000000000000, -0.000000000000000000, -1.000000000000000000 ) ) ;
#23347 = DIRECTION ( 'NONE',  ( -0.6427681459581293666, -0.7660444431189770143, -0.005002170337467561935 ) ) ;
#23348 = PLANE ( 'NONE',  #38803 ) ;
#23349 = VECTOR ( 'NONE', #16284, 1000.000000000000227 ) ;
#23350 = CARTESIAN_POINT ( 'NONE',  ( -67.25378808574402001, -11.41998066427858483, 8.237893588737414063 ) ) ;
#23351 = ORIENTED_EDGE ( 'NONE', *, *, #20555, .T. ) ;
#23352 = CARTESIAN_POINT ( 'NONE',  ( -14.46888367232926420, 0.000000000000000000, 12.59025272694991315 ) ) ;
#23353 = CARTESIAN_POINT ( 'NONE',  ( -16.01737567250614092, 0.000000000000000000, 6.742422609663679900 ) ) ;
#23354 = CARTESIAN_POINT ( 'NONE',  ( -66.10469148387817029, 7.155734338404329264E-14, -3.769581895381322934 ) ) ;
#23355 = ORIENTED_EDGE ( 'NONE', *, *, #29506, .F. ) ;
#23356 = PLANE ( 'NONE',  #51064 ) ;
#23357 = DIRECTION ( 'NONE',  ( -0.005002170337468016433, -0.7660444431189770143, 0.6427681459581293666 ) ) ;
#23358 = ORIENTED_EDGE ( 'NONE', *, *, #55538, .F. ) ;
#23359 = EDGE_CURVE ( 'NONE', #31029, #41467, #31329, .T. ) ;
#23360 = EDGE_CURVE ( 'NONE', #4025, #4723, #26784, .T. ) ;
#23361 = VECTOR ( 'NONE', #14044, 999.9999999999998863 ) ;
#23362 = DIRECTION ( 'NONE',  ( 0.5364919789714477361, 0.6444004775717706579, 0.5449076811759711036 ) ) ;
#23363 = LINE ( 'NONE', #44364, #23326 ) ;
#23364 = ADVANCED_FACE ( 'NONE', ( #14000 ), #39006, .F. ) ;
#23365 = DIRECTION ( 'NONE',  ( 0.000000000000000000, -0.000000000000000000, -1.000000000000000000 ) ) ;
#23366 = ORIENTED_EDGE ( 'NONE', *, *, #28922, .T. ) ;
#23367 = EDGE_LOOP ( 'NONE', ( #32715, #37060, #40810, #37978 ) ) ;
#23368 = DIRECTION ( 'NONE',  ( 0.000000000000000000, 0.000000000000000000, 1.000000000000000000 ) ) ;
#23369 = CARTESIAN_POINT ( 'NONE',  ( -23.44702061269273230, 18.93456859731804087, -4.495868787147773382 ) ) ;
#23370 = FACE_OUTER_BOUND ( 'NONE', #28672, .T. ) ;
#23371 = DIRECTION ( 'NONE',  ( 0.005961354470445682716, -0.6427876096865404731, -0.7660212471507180654 ) ) ;
#23372 = EDGE_LOOP ( 'NONE', ( #13529, #15583, #2481, #39863 ) ) ;
#23373 = ADVANCED_FACE ( 'NONE', ( #27069 ), #18538, .F. ) ;
#23374 = CARTESIAN_POINT ( 'NONE',  ( -6.110905869600904872, 1.712176620043476140E-14, -3.600000000000000089 ) ) ;
#23375 = EDGE_LOOP ( 'NONE', ( #231, #23921, #49353, #14323 ) ) ;
#23376 = DIRECTION ( 'NONE',  ( 0.005002170337468016433, -0.7660444431189770143, -0.6427681459581293666 ) ) ;
#23377 = ADVANCED_FACE ( 'NONE', ( #52358 ), #22535, .F. ) ;
#23378 = DIRECTION ( 'NONE',  ( 0.9999697198139515519, 0.000000000000000000, 0.007781995580013368816 ) ) ;
#23379 = EDGE_LOOP ( 'NONE', ( #43851, #48598, #55779, #10610 ) ) ;
#23380 = CARTESIAN_POINT ( 'NONE',  ( -18.12751359961164965, 0.000000000000000000, 5.048666692945789514 ) ) ;
#23381 = CARTESIAN_POINT ( 'NONE',  ( -18.32331583567987110, 0.000000000000000000, 4.508484831277049132 ) ) ;
#23382 = DIRECTION ( 'NONE',  ( -0.5449076811759708816, 0.6444004775717707689, 0.5364919789714475140 ) ) ;
#23383 = ORIENTED_EDGE ( 'NONE', *, *, #8942, .F. ) ;
#23384 = ADVANCED_FACE ( 'NONE', ( #47820 ), #43291, .F. ) ;
#23385 = FACE_OUTER_BOUND ( 'NONE', #17761, .T. ) ;
#23386 = ORIENTED_EDGE ( 'NONE', *, *, #28219, .F. ) ;
#23387 = ORIENTED_EDGE ( 'NONE', *, *, #38026, .T. ) ;
#23388 = ORIENTED_EDGE ( 'NONE', *, *, #48035, .T. ) ;
#23389 = DIRECTION ( 'NONE',  ( -0.000000000000000000, -0.000000000000000000, -1.000000000000000000 ) ) ;
#23390 = VERTEX_POINT ( 'NONE', #14308 ) ;
#23391 = CARTESIAN_POINT ( 'NONE',  ( -69.40103061304014886, -8.646553156806547236, -7.175319846998990947 ) ) ;
#23392 = ORIENTED_EDGE ( 'NONE', *, *, #1647, .F. ) ;
#23393 = DIRECTION ( 'NONE',  ( 0.5449076811759707706, 0.6444004775717708799, -0.5364919789714476250 ) ) ;
#23394 = DIRECTION ( 'NONE',  ( 0.5449076811759707706, 0.6444004775717708799, -0.5364919789714476250 ) ) ;
#23395 = VECTOR ( 'NONE', #4896, 999.9999999999998863 ) ;
#23396 = EDGE_LOOP ( 'NONE', ( #35326, #3421, #55200, #14375 ) ) ;
#23397 = LINE ( 'NONE', #45244, #16768 ) ;
#23398 = ORIENTED_EDGE ( 'NONE', *, *, #36259, .F. ) ;
#23399 = DIRECTION ( 'NONE',  ( 0.9999697198139515519, 0.000000000000000000, 0.007781995580013368816 ) ) ;
#23400 = CARTESIAN_POINT ( 'NONE',  ( -16.93098182883635161, 2.229229656569007734, 3.187375955030960384 ) ) ;
#23401 = CARTESIAN_POINT ( 'NONE',  ( -23.33693525117809386, 0.000000000000000000, 5.746789908705562944 ) ) ;
#23402 = CARTESIAN_POINT ( 'NONE',  ( -17.22853674009830982, 0.000000000000000000, 8.948989493022244446 ) ) ;
#23403 = FACE_OUTER_BOUND ( 'NONE', #13181, .T. ) ;
#23404 = LINE ( 'NONE', #10337, #49117 ) ;
#23405 = CARTESIAN_POINT ( 'NONE',  ( -18.29747203306047609, -0.1191753592594177458, 14.03778604627889059 ) ) ;
#23406 = ORIENTED_EDGE ( 'NONE', *, *, #26105, .T. ) ;
#23407 = EDGE_CURVE ( 'NONE', #49493, #13272, #13456, .T. ) ;
#23408 = ORIENTED_EDGE ( 'NONE', *, *, #44682, .F. ) ;
#23409 = FACE_OUTER_BOUND ( 'NONE', #45644, .T. ) ;
#23410 = DIRECTION ( 'NONE',  ( -0.005002170337468016433, -0.7660444431189770143, 0.6427681459581293666 ) ) ;
#23411 = EDGE_CURVE ( 'NONE', #2305, #20314, #43537, .T. ) ;
#23412 = CARTESIAN_POINT ( 'NONE',  ( -14.66887761629205222, 0.000000000000000000, 12.58869632783390990 ) ) ;
#23413 = PLANE ( 'NONE',  #41252 ) ;
#23414 = ORIENTED_EDGE ( 'NONE', *, *, #48616, .T. ) ;
#23415 = ADVANCED_FACE ( 'NONE', ( #43809 ), #34738, .T. ) ;
#23416 = FACE_OUTER_BOUND ( 'NONE', #11312, .T. ) ;
#23417 = CARTESIAN_POINT ( 'NONE',  ( -14.94760462649100496, 0.000000000000000000, 2.488088991209854051 ) ) ;
#23418 = EDGE_LOOP ( 'NONE', ( #8903, #54271, #35801, #17234, #38761 ) ) ;
#23419 = CARTESIAN_POINT ( 'NONE',  ( -20.50190040964466220, 0.9340140483890051470, 4.615766159821488301 ) ) ;
#23420 = LINE ( 'NONE', #44165, #45769 ) ;
#23421 = EDGE_LOOP ( 'NONE', ( #20786, #48034, #21503, #35670 ) ) ;
#23422 = EDGE_CURVE ( 'NONE', #24462, #1004, #21950, .T. ) ;
#23423 = EDGE_CURVE ( 'NONE', #36489, #2552, #367, .T. ) ;
#23424 = EDGE_CURVE ( 'NONE', #722, #23833, #671, .T. ) ;
#23425 = CARTESIAN_POINT ( 'NONE',  ( -67.70181732770106464, -8.853663008591706074, -5.215119943113103673 ) ) ;
#23426 = FACE_OUTER_BOUND ( 'NONE', #9256, .T. ) ;
#23427 = PLANE ( 'NONE',  #54968 ) ;
#23428 = ADVANCED_FACE ( 'NONE', ( #10302 ), #11118, .F. ) ;
#23429 = LINE ( 'NONE', #45531, #40523 ) ;
#23430 = CARTESIAN_POINT ( 'NONE',  ( -16.69028063513684401, -0.5179957512181557755, 3.347866143715504172 ) ) ;
#23431 = ORIENTED_EDGE ( 'NONE', *, *, #13845, .F. ) ;
#23432 = ORIENTED_EDGE ( 'NONE', *, *, #11744, .F. ) ;
#23433 = CARTESIAN_POINT ( 'NONE',  ( -21.24361069134453928, 2.876837460659007473, 9.854441329274578720 ) ) ;
#23434 = CARTESIAN_POINT ( 'NONE',  ( 5.273499422741863008, -1.089864486915345099, -2.388555951666875288 ) ) ;
#23435 = CARTESIAN_POINT ( 'NONE',  ( -17.73140113748535285, 0.000000000000000000, 13.85752530597602039 ) ) ;
#23436 = AXIS2_PLACEMENT_3D ( 'NONE', #22705, #53098, #14216 ) ;
#23437 = CARTESIAN_POINT ( 'NONE',  ( -19.67003419247834373, 2.714935509636508204, 4.235820352017147350 ) ) ;
#23438 = EDGE_CURVE ( 'NONE', #24207, #37392, #28165, .T. ) ;
#23439 = LINE ( 'NONE', #54616, #49416 ) ;
#23440 = ORIENTED_EDGE ( 'NONE', *, *, #51691, .T. ) ;
#23441 = FACE_OUTER_BOUND ( 'NONE', #3177, .T. ) ;
#23442 = LINE ( 'NONE', #10377, #7527 ) ;
#23443 = EDGE_CURVE ( 'NONE', #21504, #41243, #13517, .T. ) ;
#23444 = DIRECTION ( 'NONE',  ( -0.005002170337468016433, -0.7660444431189770143, 0.6427681459581293666 ) ) ;
#23445 = CARTESIAN_POINT ( 'NONE',  ( -20.33106256009199697, 20.92013140390070802, -4.309024953547888614 ) ) ;
#23446 = ORIENTED_EDGE ( 'NONE', *, *, #28948, .F. ) ;
#23447 = EDGE_CURVE ( 'NONE', #40865, #15160, #41232, .T. ) ;
#23448 = DIRECTION ( 'NONE',  ( -0.9999697198139514409, -0.000000000000000000, -0.007781995580013368816 ) ) ;
#23449 = EDGE_LOOP ( 'NONE', ( #22429, #22347, #39522, #48747 ) ) ;
#23450 = CARTESIAN_POINT ( 'NONE',  ( 2.072287782118878319, 0.000000000000000000, -2.950529333540147015 ) ) ;
#23451 = FACE_OUTER_BOUND ( 'NONE', #15466, .T. ) ;
#23452 = ORIENTED_EDGE ( 'NONE', *, *, #50337, .T. ) ;
#23453 = ADVANCED_FACE ( 'NONE', ( #28442 ), #45760, .F. ) ;
#23454 = FACE_OUTER_BOUND ( 'NONE', #54984, .T. ) ;
#23455 = ORIENTED_EDGE ( 'NONE', *, *, #37989, .T. ) ;
#23456 = EDGE_CURVE ( 'NONE', #10838, #25675, #32456, .T. ) ;
#23457 = VERTEX_POINT ( 'NONE', #19922 ) ;
#23458 = ORIENTED_EDGE ( 'NONE', *, *, #6732, .T. ) ;
#23459 = CARTESIAN_POINT ( 'NONE',  ( -46.52156441860518754, 5.799038105676674881, 5.000000000000000000 ) ) ;
#23460 = ORIENTED_EDGE ( 'NONE', *, *, #47830, .T. ) ;
#23461 = ORIENTED_EDGE ( 'NONE', *, *, #406, .T. ) ;
#23462 = CARTESIAN_POINT ( 'NONE',  ( -19.42910703681909368, 21.15220053346460816, -4.657437592157546824 ) ) ;
#23463 = DIRECTION ( 'NONE',  ( 0.7660212471507180654, -0.6427876096865404731, 0.005961354470445141482 ) ) ;
#23464 = ORIENTED_EDGE ( 'NONE', *, *, #39015, .T. ) ;
#23465 = ORIENTED_EDGE ( 'NONE', *, *, #41662, .T. ) ;
#23466 = DIRECTION ( 'NONE',  ( 0.9999697198139515519, 0.000000000000000000, 0.007781995580013368816 ) ) ;
#23467 = ORIENTED_EDGE ( 'NONE', *, *, #54619, .F. ) ;
#23468 = VERTEX_POINT ( 'NONE', #1764 ) ;
#23469 = DIRECTION ( 'NONE',  ( -0.6427681459581293666, -0.7660444431189770143, -0.005002170337467561935 ) ) ;
#23470 = PLANE ( 'NONE',  #14899 ) ;
#23471 = CARTESIAN_POINT ( 'NONE',  ( -23.44702061269273230, 18.93456859731804087, -4.495868787147773382 ) ) ;
#23472 = DIRECTION ( 'NONE',  ( -0.005002170337468016433, -0.7660444431189770143, 0.6427681459581293666 ) ) ;
#23473 = ORIENTED_EDGE ( 'NONE', *, *, #51142, .F. ) ;
#23474 = DIRECTION ( 'NONE',  ( -0.6427681459581293666, -0.7660444431189770143, -0.005002170337467561935 ) ) ;
#23475 = ORIENTED_EDGE ( 'NONE', *, *, #48325, .F. ) ;
#23476 = VECTOR ( 'NONE', #21677, 999.9999999999998863 ) ;
#23477 = PLANE ( 'NONE',  #55624 ) ;
#23478 = CARTESIAN_POINT ( 'NONE',  ( -12.33850799832341849, 0.000000000000000000, 11.68350162852954632 ) ) ;
#23479 = DIRECTION ( 'NONE',  ( 0.5449076811759707706, 0.6444004775717708799, -0.5364919789714476250 ) ) ;
#23480 = FACE_OUTER_BOUND ( 'NONE', #26580, .T. ) ;
#23481 = CARTESIAN_POINT ( 'NONE',  ( -34.64355613791357769, -1.000000000000000000, 10.23836012842048326 ) ) ;
#23482 = CARTESIAN_POINT ( 'NONE',  ( -5.572931691540063071, -7.450474849124534948, 5.383089502214839506 ) ) ;
#23483 = EDGE_LOOP ( 'NONE', ( #42357, #56020, #52629, #41101 ) ) ;
#23484 = LINE ( 'NONE', #48177, #2933 ) ;
#23485 = EDGE_LOOP ( 'NONE', ( #53345, #40684, #31436, #17511 ) ) ;
#23486 = ADVANCED_FACE ( 'NONE', ( #19665 ), #31874, .F. ) ;
#23487 = ADVANCED_FACE ( 'NONE', ( #32167 ), #24205, .F. ) ;
#23488 = DIRECTION ( 'NONE',  ( 0.5364919789714477361, 0.6444004775717706579, 0.5449076811759711036 ) ) ;
#23489 = CARTESIAN_POINT ( 'NONE',  ( -21.47263955680318404, 0.000000000000000000, 5.022634149262071190 ) ) ;
#23490 = LINE ( 'NONE', #19202, #39908 ) ;
#23491 = DIRECTION ( 'NONE',  ( -0.7660212471507179544, -0.6427876096865405842, -0.005961354470445141482 ) ) ;
#23492 = ADVANCED_FACE ( 'NONE', ( #14841 ), #53721, .T. ) ;
#23493 = CARTESIAN_POINT ( 'NONE',  ( -16.06709938707323460, 0.000000000000000000, 13.13181314741652628 ) ) ;
#23494 = DIRECTION ( 'NONE',  ( 0.6427681459581294776, -0.7660444431189769032, 0.005002170337467562802 ) ) ;
#23495 = ORIENTED_EDGE ( 'NONE', *, *, #18738, .T. ) ;
#23496 = CARTESIAN_POINT ( 'NONE',  ( -13.07066190154808361, 0.000000000000000000, 12.04713590736729678 ) ) ;
#23497 = CARTESIAN_POINT ( 'NONE',  ( -18.86354292863559579, 0.000000000000000000, 14.21804678658176080 ) ) ;
#23498 = CARTESIAN_POINT ( 'NONE',  ( -10.39993976222315020, 0.000000000000000000, 1.415483761308304889 ) ) ;
#23499 = CARTESIAN_POINT ( 'NONE',  ( -18.29402319138922905, 4.333955019861509328, 11.10009953143296890 ) ) ;
#23500 = DIRECTION ( 'NONE',  ( 0.007781995580012663651, 0.000000000000000000, -0.9999697198139515519 ) ) ;
#23501 = LINE ( 'NONE', #49631, #33628 ) ;
#23502 = DIRECTION ( 'NONE',  ( -0.7660212471507179544, -0.6427876096865405842, -0.005961354470445141482 ) ) ;
#23503 = PLANE ( 'NONE',  #24190 ) ;
#23504 = CARTESIAN_POINT ( 'NONE',  ( -9.648497380287073710, 7.293932373027242733, 0.5294304711899612270 ) ) ;
#23505 = VERTEX_POINT ( 'NONE', #27626 ) ;
#23506 = VECTOR ( 'NONE', #28146, 1000.000000000000227 ) ;
#23507 = ORIENTED_EDGE ( 'NONE', *, *, #10719, .T. ) ;
#23508 = ADVANCED_FACE ( 'NONE', ( #54020 ), #36409, .F. ) ;
#23509 = ORIENTED_EDGE ( 'NONE', *, *, #51446, .T. ) ;
#23510 = ORIENTED_EDGE ( 'NONE', *, *, #44063, .F. ) ;
#23511 = ORIENTED_EDGE ( 'NONE', *, *, #33013, .T. ) ;
#23512 = EDGE_CURVE ( 'NONE', #54767, #3728, #15387, .T. ) ;
#23513 = ORIENTED_EDGE ( 'NONE', *, *, #51883, .T. ) ;
#23514 = DIRECTION ( 'NONE',  ( -0.005002170337468016433, -0.7660444431189770143, 0.6427681459581293666 ) ) ;
#23515 = EDGE_CURVE ( 'NONE', #27231, #18068, #2031, .T. ) ;
#23516 = CARTESIAN_POINT ( 'NONE',  ( -19.98373089971760663, 3.038739411681507185, 9.630769916459319901 ) ) ;
#23517 = ORIENTED_EDGE ( 'NONE', *, *, #14251, .F. ) ;
#23518 = EDGE_LOOP ( 'NONE', ( #17088, #9229, #11640, #18149 ) ) ;
#23519 = EDGE_CURVE ( 'NONE', #55275, #28007, #15138, .T. ) ;
#23520 = ORIENTED_EDGE ( 'NONE', *, *, #19957, .T. ) ;
#23521 = LINE ( 'NONE', #9912, #32136 ) ;
#23522 = DIRECTION ( 'NONE',  ( 0.007781995580012663651, -3.146120232559066537E-19, -0.9999697198139514409 ) ) ;
#23523 = FACE_OUTER_BOUND ( 'NONE', #15404, .T. ) ;
#23524 = ORIENTED_EDGE ( 'NONE', *, *, #38476, .F. ) ;
#23525 = FACE_OUTER_BOUND ( 'NONE', #1130, .T. ) ;
#23526 = ORIENTED_EDGE ( 'NONE', *, *, #4685, .F. ) ;
#23527 = DIRECTION ( 'NONE',  ( 0.5449076811759707706, 0.6444004775717708799, -0.5364919789714476250 ) ) ;
#23528 = FACE_OUTER_BOUND ( 'NONE', #15821, .T. ) ;
#23529 = DIRECTION ( 'NONE',  ( -0.5364919789714478471, 0.6444004775717705469, -0.5449076811759709926 ) ) ;
#23530 = FACE_OUTER_BOUND ( 'NONE', #47062, .T. ) ;
#23531 = CARTESIAN_POINT ( 'NONE',  ( -11.87243407472968926, 0.000000000000000000, 11.50246268866867361 ) ) ;
#23532 = DIRECTION ( 'NONE',  ( 0.005002170337468016433, -0.7660444431189770143, -0.6427681459581293666 ) ) ;
#23533 = CARTESIAN_POINT ( 'NONE',  ( -14.58191950326086506, -5.213152330870665097, 2.379107003115130681 ) ) ;
#23534 = CARTESIAN_POINT ( 'NONE',  ( -20.12057211929586842, -0.08555834696032495190, 5.843614541628033621 ) ) ;
#23535 = ORIENTED_EDGE ( 'NONE', *, *, #24442, .T. ) ;
#23536 = CARTESIAN_POINT ( 'NONE',  ( -22.50936818614147583, 4.981562823951513508, 5.266396820920741462 ) ) ;
#23537 = ORIENTED_EDGE ( 'NONE', *, *, #26528, .F. ) ;
#23538 = AXIS2_PLACEMENT_3D ( 'NONE', #8534, #19842, #37161 ) ;
#23539 = ADVANCED_FACE ( 'NONE', ( #36159 ), #15651, .T. ) ;
#23540 = DIRECTION ( 'NONE',  ( -0.9999697198139514409, -0.000000000000000000, -0.007781995580013368816 ) ) ;
#23541 = DIRECTION ( 'NONE',  ( 0.5449076811759707706, 0.6444004775717708799, -0.5364919789714476250 ) ) ;
#23542 = CARTESIAN_POINT ( 'NONE',  ( -13.27065584551087163, 0.000000000000000000, 12.04557950825129176 ) ) ;
#23543 = DIRECTION ( 'NONE',  ( -0.5449076811759708816, 0.6444004775717707689, 0.5364919789714475140 ) ) ;
#23544 = LINE ( 'NONE', #28346, #17798 ) ;
#23545 = FACE_OUTER_BOUND ( 'NONE', #9102, .T. ) ;
#23546 = EDGE_CURVE ( 'NONE', #28121, #2600, #18839, .T. ) ;
#23547 = EDGE_CURVE ( 'NONE', #16295, #37024, #12254, .T. ) ;
#23548 = PLANE ( 'NONE',  #51528 ) ;
#23549 = FACE_OUTER_BOUND ( 'NONE', #32884, .T. ) ;
#23550 = SURFACE_STYLE_USAGE ( .BOTH. , #14220 ) ;
#23551 = DIRECTION ( 'NONE',  ( 0.5449076811759707706, 0.6444004775717708799, -0.5364919789714476250 ) ) ;
#23552 = ORIENTED_EDGE ( 'NONE', *, *, #17800, .F. ) ;
#23553 = FACE_OUTER_BOUND ( 'NONE', #14496, .T. ) ;
#23554 = CARTESIAN_POINT ( 'NONE',  ( -14.09271583063079980, -0.03739765774599798642, 2.294034608853361856 ) ) ;
#23555 = DIRECTION ( 'NONE',  ( 0.007781995580012663651, 0.000000000000000000, -0.9999697198139515519 ) ) ;
#23556 = CARTESIAN_POINT ( 'NONE',  ( -16.03749404704311843, 0.000000000000000000, 9.327590532468031270 ) ) ;
#23557 = LINE ( 'NONE', #53388, #35458 ) ;
#23558 = LINE ( 'NONE', #54218, #34829 ) ;
#23559 = CARTESIAN_POINT ( 'NONE',  ( 5.284044854955649129, -1.088655197871726710, 2.393421119419573806 ) ) ;
#23560 = FACE_OUTER_BOUND ( 'NONE', #16835, .T. ) ;
#23561 = EDGE_CURVE ( 'NONE', #15806, #23767, #51449, .T. ) ;
#23562 = EDGE_LOOP ( 'NONE', ( #39316, #52229, #40183, #51652 ) ) ;
#23563 = ORIENTED_EDGE ( 'NONE', *, *, #5913, .F. ) ;
#23564 = CARTESIAN_POINT ( 'NONE',  ( -19.45503627000849889, 0.000000000000000000, 7.556996783084074742 ) ) ;
#23565 = PLANE ( 'NONE',  #51212 ) ;
#23566 = ORIENTED_EDGE ( 'NONE', *, *, #19082, .F. ) ;
#23567 = CARTESIAN_POINT ( 'NONE',  ( -25.20278734466900517, 0.000000000000000000, 6.670939612111840944 ) ) ;
#23568 = ORIENTED_EDGE ( 'NONE', *, *, #18864, .T. ) ;
#23569 = DIRECTION ( 'NONE',  ( 0.5449076811759707706, 0.6444004775717708799, -0.5364919789714476250 ) ) ;
#23570 = ORIENTED_EDGE ( 'NONE', *, *, #16603, .F. ) ;
#23571 = ORIENTED_EDGE ( 'NONE', *, *, #31453, .T. ) ;
#23572 = VERTEX_POINT ( 'NONE', #29863 ) ;
#23573 = LINE ( 'NONE', #19867, #3931 ) ;
#23574 = DIRECTION ( 'NONE',  ( -0.7660212471507179544, -0.6427876096865405842, -0.005961354470445141482 ) ) ;
#23575 = PLANE ( 'NONE',  #12187 ) ;
#23576 = ORIENTED_EDGE ( 'NONE', *, *, #11071, .T. ) ;
#23577 = EDGE_CURVE ( 'NONE', #31801, #18836, #3717, .T. ) ;
#23578 = EDGE_LOOP ( 'NONE', ( #4203, #17160, #43671, #40622 ) ) ;
#23579 = DIRECTION ( 'NONE',  ( -0.2426528472758541499, 0.7422098413412800966, -0.6246952433987894571 ) ) ;
#23580 = EDGE_LOOP ( 'NONE', ( #38559, #21962, #34764, #25643 ) ) ;
#23581 = PLANE ( 'NONE',  #29143 ) ;
#23582 = VERTEX_POINT ( 'NONE', #47160 ) ;
#23583 = CARTESIAN_POINT ( 'NONE',  ( 2.072287782118878319, 0.000000000000000000, -2.950529333540147015 ) ) ;
#23584 = PLANE ( 'NONE',  #14048 ) ;
#23585 = ADVANCED_FACE ( 'NONE', ( #21036 ), #41768, .F. ) ;
#23586 = VERTEX_POINT ( 'NONE', #42905 ) ;
#23587 = CARTESIAN_POINT ( 'NONE',  ( -14.14577547200466690, 0.000000000000000000, 5.079653499741873190 ) ) ;
#23588 = EDGE_CURVE ( 'NONE', #34236, #17943, #33828, .T. ) ;
#23589 = EDGE_CURVE ( 'NONE', #55206, #46078, #38366, .T. ) ;
#23590 = LINE ( 'NONE', #40908, #32709 ) ;
#23591 = ORIENTED_EDGE ( 'NONE', *, *, #24294, .F. ) ;
#23592 = CARTESIAN_POINT ( 'NONE',  ( 2.072287782118878319, 0.000000000000000000, -2.950529333540147015 ) ) ;
#23593 = CARTESIAN_POINT ( 'NONE',  ( -15.49757964982686786, 4.333955019861511104, 10.01386589226773616 ) ) ;
#23594 = PLANE ( 'NONE',  #54613 ) ;
#23595 = EDGE_CURVE ( 'NONE', #40095, #3791, #37829, .T. ) ;
#23596 = VERTEX_POINT ( 'NONE', #15956 ) ;
#23597 = ADVANCED_FACE ( 'NONE', ( #51144 ), #17084, .F. ) ;
#23598 = CARTESIAN_POINT ( 'NONE',  ( -19.45503627000849889, -1.000000000000000000, 7.556996783084074742 ) ) ;
#23599 = DIRECTION ( 'NONE',  ( 0.005002170337468016433, -0.7660444431189770143, -0.6427681459581293666 ) ) ;
#23600 = CARTESIAN_POINT ( 'NONE',  ( -3.033112459793370075, -5.745301166973593610, -2.040209691347345533 ) ) ;
#23601 = DIRECTION ( 'NONE',  ( 0.6246952433987894571, -0.7422098413412800966, -0.2426528472758541777 ) ) ;
#23602 = PLANE ( 'NONE',  #50332 ) ;
#23603 = EDGE_CURVE ( 'NONE', #1256, #22414, #4014, .T. ) ;
#23604 = LINE ( 'NONE', #18812, #55125 ) ;
#23605 = VECTOR ( 'NONE', #26614, 1000.000000000000114 ) ;
#23606 = CARTESIAN_POINT ( 'NONE',  ( -67.60174820569504561, -9.580611907208711031, 4.357869429825873553 ) ) ;
#23607 = ORIENTED_EDGE ( 'NONE', *, *, #35403, .T. ) ;
#23608 = DIRECTION ( 'NONE',  ( -0.6427681459581293666, -0.7660444431189770143, -0.005002170337467561935 ) ) ;
#23609 = CARTESIAN_POINT ( 'NONE',  ( -27.99923088623136636, 0.000000000000000000, 7.757173251277078130 ) ) ;
#23610 = CARTESIAN_POINT ( 'NONE',  ( -67.26227515700414017, 8.227372716571623961E-12, 4.538413701022403046 ) ) ;
#23611 = ORIENTED_EDGE ( 'NONE', *, *, #27529, .T. ) ;
#23612 = CARTESIAN_POINT ( 'NONE',  ( -30.79411802867772607, 0.000000000000000000, 8.643412946479525516 ) ) ;
#23613 = LINE ( 'NONE', #41506, #6434 ) ;
#23614 = EDGE_CURVE ( 'NONE', #27150, #44163, #7416, .T. ) ;
#23615 = FACE_OUTER_BOUND ( 'NONE', #9390, .T. ) ;
#23616 = CARTESIAN_POINT ( 'NONE',  ( -19.35787096931604268, 0.1245042932765045296, 4.604908354090325062 ) ) ;
#23617 = DIRECTION ( 'NONE',  ( 0.000000000000000000, -1.000000000000000000, 0.000000000000000000 ) ) ;
#23618 = EDGE_CURVE ( 'NONE', #36106, #28751, #24740, .T. ) ;
#23619 = EDGE_LOOP ( 'NONE', ( #20351, #2977, #40068, #46214 ) ) ;
#23620 = ORIENTED_EDGE ( 'NONE', *, *, #49754, .T. ) ;
#23621 = PLANE ( 'NONE',  #14145 ) ;
#23622 = DIRECTION ( 'NONE',  ( -0.9999697198139514409, -0.000000000000000000, -0.007781995580013368816 ) ) ;
#23623 = CARTESIAN_POINT ( 'NONE',  ( -24.56000265080053069, 18.39574225916684824, -4.548402510131950294 ) ) ;
#23624 = ORIENTED_EDGE ( 'NONE', *, *, #11511, .T. ) ;
#23625 = CARTESIAN_POINT ( 'NONE',  ( -16.33317936670417225, 0.000000000000000000, 13.31440848639340224 ) ) ;
#23626 = ORIENTED_EDGE ( 'NONE', *, *, #41772, .F. ) ;
#23627 = DIRECTION ( 'NONE',  ( 0.6427681459581294776, -0.7660444431189769032, 0.005002170337467562802 ) ) ;
#23628 = ORIENTED_EDGE ( 'NONE', *, *, #2163, .F. ) ;
#23629 = ORIENTED_EDGE ( 'NONE', *, *, #36781, .T. ) ;
#23630 = FACE_OUTER_BOUND ( 'NONE', #32544, .T. ) ;
#23631 = CARTESIAN_POINT ( 'NONE',  ( -11.34226616904245333, 0.000000000000000000, 3.085484694766132741 ) ) ;
#23632 = PLANE ( 'NONE',  #37519 ) ;
#23633 = ORIENTED_EDGE ( 'NONE', *, *, #2115, .T. ) ;
#23635 = CARTESIAN_POINT ( 'NONE',  ( -9.487910289572674571, 0.000000000000000000, 3.638573804390909938 ) ) ;
#23634 = VECTOR ( 'NONE', #8227, 1000.000000000000227 ) ;
#23636 = EDGE_CURVE ( 'NONE', #8596, #54373, #42622, .T. ) ;
#23637 = EDGE_LOOP ( 'NONE', ( #535, #45253, #35100, #55162 ) ) ;
#23638 = VECTOR ( 'NONE', #17973, 999.9999999999998863 ) ;
#23639 = ORIENTED_EDGE ( 'NONE', *, *, #48684, .F. ) ;
#23640 = ORIENTED_EDGE ( 'NONE', *, *, #20832, .T. ) ;
#23641 = DIRECTION ( 'NONE',  ( -0.005961354470445682716, -0.6427876096865404731, 0.7660212471507180654 ) ) ;
#23642 = ORIENTED_EDGE ( 'NONE', *, *, #19119, .T. ) ;
#23643 = CARTESIAN_POINT ( 'NONE',  ( -18.86354292863559579, 0.000000000000000000, 14.21804678658176080 ) ) ;
#23644 = VERTEX_POINT ( 'NONE', #38669 ) ;
#23645 = DIRECTION ( 'NONE',  ( -0.6427681459581293666, -0.7660444431189770143, -0.005002170337467561935 ) ) ;
#23646 = DIRECTION ( 'NONE',  ( 0.005002170337468016433, -0.7660444431189770143, -0.6427681459581293666 ) ) ;
#23647 = ORIENTED_EDGE ( 'NONE', *, *, #49992, .F. ) ;
#23648 = DIRECTION ( 'NONE',  ( 0.9999697198139515519, 0.000000000000000000, 0.007781995580013368816 ) ) ;
#23649 = EDGE_LOOP ( 'NONE', ( #34072, #54560, #55036, #30815 ) ) ;
#23650 = ADVANCED_FACE ( 'NONE', ( #3163 ), #11952, .F. ) ;
#23651 = LINE ( 'NONE', #31645, #40987 ) ;
#23652 = CARTESIAN_POINT ( 'NONE',  ( -18.16643269429632568, 0.000000000000000000, 10.04968677925951681 ) ) ;
#23653 = PLANE ( 'NONE',  #46813 ) ;
#23654 = DIRECTION ( 'NONE',  ( 0.5449076811759707706, 0.6444004775717708799, -0.5364919789714476250 ) ) ;
#23655 = DIRECTION ( 'NONE',  ( 0.7660212471507180654, -0.6427876096865404731, 0.005961354470445141482 ) ) ;
#23656 = CARTESIAN_POINT ( 'NONE',  ( 2.072287782118878319, 0.000000000000000000, -2.950529333540147015 ) ) ;
#23657 = DIRECTION ( 'NONE',  ( 0.007781995580012663651, -3.146120232559066537E-19, -0.9999697198139514409 ) ) ;
#23658 = EDGE_LOOP ( 'NONE', ( #37259, #22578, #41392, #36498 ) ) ;
#23659 = ORIENTED_EDGE ( 'NONE', *, *, #41777, .F. ) ;
#23660 = VECTOR ( 'NONE', #54690, 999.9999999999998863 ) ;
#23661 = EDGE_CURVE ( 'NONE', #36484, #1451, #33546, .T. ) ;
#23662 = CARTESIAN_POINT ( 'NONE',  ( -24.96676581047183063, 18.24370688441070953, -4.565775476651154463 ) ) ;
#23663 = CARTESIAN_POINT ( 'NONE',  ( -68.98024086217516526, -9.100687180210641714, 7.490399608206207205 ) ) ;
#23664 = CARTESIAN_POINT ( 'NONE',  ( -13.87933636775488289, -3.270328918600661883, 2.168186092109577690 ) ) ;
#23665 = EDGE_CURVE ( 'NONE', #7585, #25732, #16226, .T. ) ;
#23666 = CARTESIAN_POINT ( 'NONE',  ( -15.33550051067056685, 0.000000000000000000, 4.531736701001109147 ) ) ;
#23667 = CARTESIAN_POINT ( 'NONE',  ( -9.110551994824897193, -1.000000000000000000, 3.538847790438064411 ) ) ;
#23668 = VERTEX_POINT ( 'NONE', #55398 ) ;
#23669 = DIRECTION ( 'NONE',  ( 0.000000000000000000, -1.000000000000000000, 0.000000000000000000 ) ) ;
#23670 = DIRECTION ( 'NONE',  ( 0.000000000000000000, -0.000000000000000000, -1.000000000000000000 ) ) ;
#23671 = ORIENTED_EDGE ( 'NONE', *, *, #2270, .T. ) ;
#23672 = LINE ( 'NONE', #54593, #51992 ) ;
#23673 = CARTESIAN_POINT ( 'NONE',  ( 2.072287782118878319, 0.000000000000000000, -2.950529333540147015 ) ) ;
#23674 = ORIENTED_EDGE ( 'NONE', *, *, #46449, .T. ) ;
#23675 = ADVANCED_FACE ( 'NONE', ( #25317 ), #20190, .F. ) ;
#23676 = FACE_OUTER_BOUND ( 'NONE', #28051, .T. ) ;
#23677 = CARTESIAN_POINT ( 'NONE',  ( 2.072287782118878319, 0.000000000000000000, -2.950529333540147015 ) ) ;
#23678 = VECTOR ( 'NONE', #22970, 1000.000000000000000 ) ;
#23679 = CARTESIAN_POINT ( 'NONE',  ( -16.16125387310899697, 0.000000000000000000, 9.495953418471051677 ) ) ;
#23680 = DIRECTION ( 'NONE',  ( 0.005961354470445682716, -0.6427876096865404731, -0.7660212471507180654 ) ) ;
#23681 = AXIS2_PLACEMENT_3D ( 'NONE', #13313, #9036, #34324 ) ;
#23682 = DIRECTION ( 'NONE',  ( -0.6427681459581293666, -0.7660444431189770143, -0.005002170337467561935 ) ) ;
#23683 = EDGE_CURVE ( 'NONE', #23836, #6448, #50597, .T. ) ;
#23684 = ORIENTED_EDGE ( 'NONE', *, *, #48616, .F. ) ;
#23685 = ORIENTED_EDGE ( 'NONE', *, *, #54325, .T. ) ;
#23686 = DIRECTION ( 'NONE',  ( -0.7660212471507179544, -0.6427876096865405842, -0.005961354470445141482 ) ) ;
#23687 = FACE_OUTER_BOUND ( 'NONE', #55654, .T. ) ;
#23688 = DIRECTION ( 'NONE',  ( 0.5364919789714477361, 0.6444004775717706579, 0.5449076811759711036 ) ) ;
#23689 = LINE ( 'NONE', #19433, #47287 ) ;
#23690 = DIRECTION ( 'NONE',  ( 0.000000000000000000, 1.000000000000000000, 0.000000000000000000 ) ) ;
#23691 = ORIENTED_EDGE ( 'NONE', *, *, #23216, .T. ) ;
#23692 = PLANE ( 'NONE',  #6593 ) ;
#23693 = DIRECTION ( 'NONE',  ( 0.6427681459581294776, -0.7660444431189769032, 0.005002170337467562802 ) ) ;
#23694 = CARTESIAN_POINT ( 'NONE',  ( -23.33693525117809386, 0.000000000000000000, 5.746789908705562944 ) ) ;
#23695 = ORIENTED_EDGE ( 'NONE', *, *, #5917, .T. ) ;
#23696 = LINE ( 'NONE', #19444, #22013 ) ;
#23697 = EDGE_LOOP ( 'NONE', ( #35520, #35566, #44804, #865 ) ) ;
#23698 = CARTESIAN_POINT ( 'NONE',  ( -8.842080168916501393, 0.000000000000000000, 6.059598278784299019 ) ) ;
#23699 = ADVANCED_FACE ( 'NONE', ( #34972 ), #26420, .F. ) ;
#23700 = DIRECTION ( 'NONE',  ( -0.6427681459581293666, -0.7660444431189770143, -0.005002170337467561935 ) ) ;
#23701 = ORIENTED_EDGE ( 'NONE', *, *, #48437, .F. ) ;
#23702 = VECTOR ( 'NONE', #24956, 1000.000000000000227 ) ;
#23703 = AXIS2_PLACEMENT_3D ( 'NONE', #21589, #39458, #21290 ) ;
#23704 = LINE ( 'NONE', #41027, #46768 ) ;
#23705 = EDGE_CURVE ( 'NONE', #43196, #32551, #51982, .T. ) ;
#23706 = ORIENTED_EDGE ( 'NONE', *, *, #24347, .T. ) ;
#23707 = ORIENTED_EDGE ( 'NONE', *, *, #26172, .F. ) ;
#23708 = ORIENTED_EDGE ( 'NONE', *, *, #41395, .F. ) ;
#23709 = LINE ( 'NONE', #1293, #26633 ) ;
#23710 = EDGE_CURVE ( 'NONE', #52765, #11344, #17931, .T. ) ;
#23711 = ORIENTED_EDGE ( 'NONE', *, *, #33533, .F. ) ;
#23712 = ADVANCED_FACE ( 'NONE', ( #22474 ), #52287, .F. ) ;
#23713 = ORIENTED_EDGE ( 'NONE', *, *, #7322, .T. ) ;
#23714 = CARTESIAN_POINT ( 'NONE',  ( -18.39746900504187010, 0.000000000000000000, 14.03700784672088808 ) ) ;
#23716 = EDGE_CURVE ( 'NONE', #40359, #47613, #48273, .T. ) ;
#23715 = EDGE_LOOP ( 'NONE', ( #26720, #52220, #21046, #18859, #34690 ) ) ;
#23717 = EDGE_CURVE ( 'NONE', #43426, #36296, #39783, .T. ) ;
#23718 = EDGE_CURVE ( 'NONE', #8121, #16962, #1129, .T. ) ;
#23719 = EDGE_LOOP ( 'NONE', ( #10234, #20428, #38243, #49578 ) ) ;
#23720 = DIRECTION ( 'NONE',  ( -0.005002170337468016433, -0.7660444431189770143, 0.6427681459581293666 ) ) ;
#23721 = ORIENTED_EDGE ( 'NONE', *, *, #2032, .T. ) ;
#23722 = ORIENTED_EDGE ( 'NONE', *, *, #32393, .F. ) ;
#23723 = AXIS2_PLACEMENT_3D ( 'NONE', #19040, #10247, #31825 ) ;
#23724 = ORIENTED_EDGE ( 'NONE', *, *, #49818, .T. ) ;
#23725 = LINE ( 'NONE', #19469, #32010 ) ;
#23726 = FACE_OUTER_BOUND ( 'NONE', #1899, .T. ) ;
#23727 = PLANE ( 'NONE',  #19619 ) ;
#23728 = PLANE ( 'NONE',  #6064 ) ;
#23729 = VERTEX_POINT ( 'NONE', #863 ) ;
#23730 = LINE ( 'NONE', #40789, #7461 ) ;
#23731 = ORIENTED_EDGE ( 'NONE', *, *, #44612, .F. ) ;
#23732 = ORIENTED_EDGE ( 'NONE', *, *, #26471, .T. ) ;
#23733 = EDGE_CURVE ( 'NONE', #37328, #17921, #52547, .T. ) ;
#23734 = CARTESIAN_POINT ( 'NONE',  ( -14.20918270945749029, -3.108426967578162170, 2.301475132743175056 ) ) ;
#23735 = EDGE_CURVE ( 'NONE', #42842, #19450, #52816, .T. ) ;
#23736 = LINE ( 'NONE', #36521, #11559 ) ;
#23737 = DIRECTION ( 'NONE',  ( 0.5449076811759707706, 0.6444004775717708799, -0.5364919789714476250 ) ) ;
#23738 = EDGE_CURVE ( 'NONE', #48144, #24901, #43738, .T. ) ;
#23739 = DIRECTION ( 'NONE',  ( 0.7660212471507180654, -0.6427876096865404731, 0.005961354470445141482 ) ) ;
#23740 = CARTESIAN_POINT ( 'NONE',  ( -9.759857748577539738, 0.000000000000000000, 4.575127642217221791 ) ) ;
#23741 = ORIENTED_EDGE ( 'NONE', *, *, #13053, .F. ) ;
#23742 = FACE_OUTER_BOUND ( 'NONE', #34767, .T. ) ;
#23743 = EDGE_LOOP ( 'NONE', ( #7818, #9342, #49760, #31344 ) ) ;
#23744 = VECTOR ( 'NONE', #4993, 1000.000000000000114 ) ;
#23745 = EDGE_CURVE ( 'NONE', #13391, #51597, #30711, .T. ) ;
#23746 = AXIS2_PLACEMENT_3D ( 'NONE', #50630, #54886, #25084 ) ;
#23747 = DIRECTION ( 'NONE',  ( 0.9999697198139515519, 0.000000000000000000, 0.007781995580013368816 ) ) ;
#23748 = LINE ( 'NONE', #27453, #27816 ) ;
#23749 = CARTESIAN_POINT ( 'NONE',  ( -13.08330893211609869, 0.000000000000000000, 1.763933231766363630 ) ) ;
#23750 = LINE ( 'NONE', #36842, #45834 ) ;
#23751 = DIRECTION ( 'NONE',  ( -0.3620778797217457101, 0.000000000000000000, -0.9321478471874540261 ) ) ;
#23752 = AXIS2_PLACEMENT_3D ( 'NONE', #32206, #40729, #48696 ) ;
#23753 = ORIENTED_EDGE ( 'NONE', *, *, #21870, .T. ) ;
#23754 = DIRECTION ( 'NONE',  ( 0.000000000000000000, -1.000000000000000000, 0.000000000000000000 ) ) ;
#23755 = PLANE ( 'NONE',  #9506 ) ;
#23756 = FACE_OUTER_BOUND ( 'NONE', #50365, .T. ) ;
#23757 = PLANE ( 'NONE',  #27348 ) ;
#23758 = VECTOR ( 'NONE', #53308, 1000.000000000000227 ) ;
#23759 = CARTESIAN_POINT ( 'NONE',  ( -27.99767448711536133, 0.000000000000000000, 7.557179307314289218 ) ) ;
#23760 = DIRECTION ( 'NONE',  ( 0.9999697198139515519, 0.000000000000000000, 0.007781995580013368816 ) ) ;
#23761 = DIRECTION ( 'NONE',  ( 0.5449076811759707706, 0.6444004775717708799, -0.5364919789714476250 ) ) ;
#23762 = AXIS2_PLACEMENT_3D ( 'NONE', #14031, #5504, #19111 ) ;
#23763 = CARTESIAN_POINT ( 'NONE',  ( -17.65712859575999616, 0.000000000000000000, 4.313663198198272930 ) ) ;
#23764 = DIRECTION ( 'NONE',  ( 0.007781995580012662783, 0.000000000000000000, -0.9999697198139514409 ) ) ;
#23765 = VERTEX_POINT ( 'NONE', #22174 ) ;
#23766 = EDGE_LOOP ( 'NONE', ( #13103, #50911, #38798, #14427 ) ) ;
#23767 = VERTEX_POINT ( 'NONE', #13924 ) ;
#23768 = ORIENTED_EDGE ( 'NONE', *, *, #1798, .T. ) ;
#23769 = VERTEX_POINT ( 'NONE', #21629 ) ;
#23770 = VECTOR ( 'NONE', #23812, 1000.000000000000227 ) ;
#23771 = PLANE ( 'NONE',  #39627 ) ;
#23772 = CARTESIAN_POINT ( 'NONE',  ( -23.33849165029409889, 0.000000000000000000, 5.946783852668351855 ) ) ;
#23773 = EDGE_CURVE ( 'NONE', #8547, #49068, #9695, .T. ) ;
#23774 = EDGE_CURVE ( 'NONE', #25905, #11704, #27008, .T. ) ;
#23775 = VECTOR ( 'NONE', #42429, 999.9999999999998863 ) ;
#23776 = VECTOR ( 'NONE', #18430, 999.9999999999998863 ) ;
#23777 = ORIENTED_EDGE ( 'NONE', *, *, #42269, .F. ) ;
#23778 = LINE ( 'NONE', #28318, #8624 ) ;
#23779 = ORIENTED_EDGE ( 'NONE', *, *, #24663, .T. ) ;
#23780 = EDGE_CURVE ( 'NONE', #2943, #43670, #22729, .T. ) ;
#23781 = ORIENTED_EDGE ( 'NONE', *, *, #4468, .F. ) ;
#23782 = VECTOR ( 'NONE', #39431, 1000.000000000000227 ) ;
#23783 = VECTOR ( 'NONE', #15357, 1000.000000000000227 ) ;
#23784 = CARTESIAN_POINT ( 'NONE',  ( -24.53375310857961367, 18.49370688441070953, -4.657437592157546824 ) ) ;
#23785 = DIRECTION ( 'NONE',  ( 0.007781995580012663651, -3.146120232559066537E-19, -0.9999697198139514409 ) ) ;
#23786 = LINE ( 'NONE', #6477, #6018 ) ;
#23787 = ORIENTED_EDGE ( 'NONE', *, *, #46101, .T. ) ;
#23788 = CARTESIAN_POINT ( 'NONE',  ( -10.93224078895172013, 8.537444759202470479, 1.028080007224975168 ) ) ;
#23789 = LINE ( 'NONE', #36886, #40039 ) ;
#23790 = VECTOR ( 'NONE', #37086, 1000.000000000000227 ) ;
#23791 = PLANE ( 'NONE',  #41161 ) ;
#23792 = EDGE_CURVE ( 'NONE', #38808, #10480, #40043, .T. ) ;
#23793 = FACE_OUTER_BOUND ( 'NONE', #5953, .T. ) ;
#23794 = LINE ( 'NONE', #50498, #42361 ) ;
#23795 = DIRECTION ( 'NONE',  ( 0.000000000000000000, 0.000000000000000000, 1.000000000000000000 ) ) ;
#23796 = PLANE ( 'NONE',  #51025 ) ;
#23797 = LINE ( 'NONE', #41128, #20334 ) ;
#23798 = EDGE_CURVE ( 'NONE', #23836, #45704, #8558, .T. ) ;
#23799 = DIRECTION ( 'NONE',  ( 0.7660212471507180654, -0.6427876096865404731, 0.005961354470445141482 ) ) ;
#23800 = ORIENTED_EDGE ( 'NONE', *, *, #38891, .T. ) ;
#23801 = DIRECTION ( 'NONE',  ( 0.007781995580012662783, 0.000000000000000000, -0.9999697198139514409 ) ) ;
#23802 = ORIENTED_EDGE ( 'NONE', *, *, #46147, .F. ) ;
#23803 = EDGE_CURVE ( 'NONE', #25259, #56036, #34662, .T. ) ;
#23804 = DIRECTION ( 'NONE',  ( 0.5449076811759707706, 0.6444004775717708799, -0.5364919789714476250 ) ) ;
#23805 = DIRECTION ( 'NONE',  ( 0.007781995580012663651, -3.146120232559066537E-19, -0.9999697198139514409 ) ) ;
#23806 = DIRECTION ( 'NONE',  ( 0.007781995580012663651, -3.146120232559066537E-19, -0.9999697198139514409 ) ) ;
#23807 = LINE ( 'NONE', #36322, #14159 ) ;
#23808 = AXIS2_PLACEMENT_3D ( 'NONE', #34797, #38011, #4693 ) ;
#23809 = DIRECTION ( 'NONE',  ( 0.6427681459581294776, -0.7660444431189769032, 0.005002170337467562802 ) ) ;
#23810 = FACE_OUTER_BOUND ( 'NONE', #34081, .T. ) ;
#23811 = ADVANCED_FACE ( 'NONE', ( #8861 ), #26164, .F. ) ;
#23812 = DIRECTION ( 'NONE',  ( 0.007781995580012662783, 0.000000000000000000, -0.9999697198139514409 ) ) ;
#23813 =( NAMED_UNIT ( * ) PLANE_ANGLE_UNIT ( ) SI_UNIT ( $, .RADIAN. ) );
#23814 = LINE ( 'NONE', #53922, #3824 ) ;
#23815 = VECTOR ( 'NONE', #20833, 1000.000000000000114 ) ;
#23816 = LINE ( 'NONE', #45394, #38427 ) ;
#23817 = CARTESIAN_POINT ( 'NONE',  ( -15.06510945078170494, 0.000000000000000000, 3.795176807137583985 ) ) ;
#23818 = CARTESIAN_POINT ( 'NONE',  ( -19.06253550030438504, 0.000000000000000000, 5.780054275925301077 ) ) ;
#23819 = LINE ( 'NONE', #54758, #9661 ) ;
#23820 = VECTOR ( 'NONE', #6258, 999.9999999999998863 ) ;
#23821 = AXIS2_PLACEMENT_3D ( 'NONE', #45896, #2153, #54147 ) ;
#23822 = DIRECTION ( 'NONE',  ( 0.7660212471507180654, -0.6427876096865404731, 0.005961354470445141482 ) ) ;
#23823 = CARTESIAN_POINT ( 'NONE',  ( -10.27421835998572064, 0.000000000000000000, 10.96090226820206048 ) ) ;
#23824 = DIRECTION ( 'NONE',  ( -0.9999697198139514409, -0.000000000000000000, -0.007781995580013368816 ) ) ;
#23825 = FACE_OUTER_BOUND ( 'NONE', #33790, .T. ) ;
#23826 = ORIENTED_EDGE ( 'NONE', *, *, #10829, .T. ) ;
#23827 = VECTOR ( 'NONE', #23448, 1000.000000000000227 ) ;
#23828 = LINE ( 'NONE', #11336, #31256 ) ;
#23829 = VECTOR ( 'NONE', #12462, 1000.000000000000114 ) ;
#23830 = ORIENTED_EDGE ( 'NONE', *, *, #18037, .T. ) ;
#23831 = DIRECTION ( 'NONE',  ( 0.000000000000000000, -0.000000000000000000, -1.000000000000000000 ) ) ;
#23832 = DIRECTION ( 'NONE',  ( 0.007781995580012663651, -3.146120232559066537E-19, -0.9999697198139514409 ) ) ;
#23833 = VERTEX_POINT ( 'NONE', #2542 ) ;
#23834 = DIRECTION ( 'NONE',  ( 0.005002170337468016433, -0.7660444431189770143, -0.6427681459581293666 ) ) ;
#23835 = AXIS2_PLACEMENT_3D ( 'NONE', #4213, #16389, #8445 ) ;
#23836 = VERTEX_POINT ( 'NONE', #10799 ) ;
#23837 = FACE_OUTER_BOUND ( 'NONE', #51240, .T. ) ;
#23838 = VECTOR ( 'NONE', #43365, 1000.000000000000227 ) ;
#23839 = ORIENTED_EDGE ( 'NONE', *, *, #52906, .F. ) ;
#23840 = VERTEX_POINT ( 'NONE', #44871 ) ;
#23841 = EDGE_LOOP ( 'NONE', ( #20441, #53445, #53613, #20502 ) ) ;
#23842 = CARTESIAN_POINT ( 'NONE',  ( -9.512459116730939357, 0.000000000000000000, 6.793045374415813242 ) ) ;
#23843 = CARTESIAN_POINT ( 'NONE',  ( -16.35395655750867405, -0.1191753592594181482, 3.134058533975019323 ) ) ;
#23844 = PLANE ( 'NONE',  #23985 ) ;
#23845 = VECTOR ( 'NONE', #12373, 999.9999999999998863 ) ;
#23846 = EDGE_CURVE ( 'NONE', #24756, #28463, #5688, .T. ) ;
#23847 = VERTEX_POINT ( 'NONE', #6527 ) ;
#23848 = ORIENTED_EDGE ( 'NONE', *, *, #40505, .T. ) ;
#23849 = VECTOR ( 'NONE', #50291, 999.9999999999998863 ) ;
#23850 = EDGE_CURVE ( 'NONE', #45468, #17431, #40886, .T. ) ;
#23851 = EDGE_CURVE ( 'NONE', #30589, #26710, #45167, .T. ) ;
#23852 = DIRECTION ( 'NONE',  ( 0.9999697198139515519, 0.000000000000000000, 0.007781995580013368816 ) ) ;
#23853 = ORIENTED_EDGE ( 'NONE', *, *, #15567, .T. ) ;
#23854 = VECTOR ( 'NONE', #36348, 1000.000000000000227 ) ;
#23855 = CARTESIAN_POINT ( 'NONE',  ( -16.53317331066696383, 0.000000000000000000, 13.31285208727739899 ) ) ;
#23856 = EDGE_LOOP ( 'NONE', ( #15761, #47595, #2609, #5628 ) ) ;
#23857 = CARTESIAN_POINT ( 'NONE',  ( -22.40478740399063895, 0.000000000000000000, 5.384712028983816623 ) ) ;
#23858 = CARTESIAN_POINT ( 'NONE',  ( -15.88130887279446490, 0.000000000000000000, 3.050160814894388839 ) ) ;
#23859 = VECTOR ( 'NONE', #16946, 999.9999999999998863 ) ;
#23860 = AXIS2_PLACEMENT_3D ( 'NONE', #54074, #40737, #19712 ) ;
#23861 = ORIENTED_EDGE ( 'NONE', *, *, #37641, .T. ) ;
#23862 = CARTESIAN_POINT ( 'NONE',  ( -21.69488263569956743, 4.495856970884009485, 12.68681751722644080 ) ) ;
#23863 = VECTOR ( 'NONE', #35812, 1000.000000000000227 ) ;
#23864 = DIRECTION ( 'NONE',  ( 0.7660212471507180654, -0.6427876096865404731, 0.005961354470445141482 ) ) ;
#23865 = VECTOR ( 'NONE', #44929, 999.9999999999998863 ) ;
#23866 = ORIENTED_EDGE ( 'NONE', *, *, #26643, .T. ) ;
#23867 = DIRECTION ( 'NONE',  ( 0.9999697198139515519, 0.000000000000000000, 0.007781995580013368816 ) ) ;
#23868 = DIRECTION ( 'NONE',  ( 0.5449076811759707706, 0.6444004775717708799, -0.5364919789714476250 ) ) ;
#23869 = FACE_OUTER_BOUND ( 'NONE', #38655, .T. ) ;
#23870 = ORIENTED_EDGE ( 'NONE', *, *, #47402, .F. ) ;
#23871 = DIRECTION ( 'NONE',  ( 1.000000000000000000, -3.469446951953611033E-15, 0.000000000000000000 ) ) ;
#23872 = LINE ( 'NONE', #2574, #28724 ) ;
#23873 = DIRECTION ( 'NONE',  ( 0.7660212471507180654, -0.6427876096865404731, 0.005961354470445141482 ) ) ;
#23874 = LINE ( 'NONE', #32962, #34986 ) ;
#23875 = AXIS2_PLACEMENT_3D ( 'NONE', #46396, #7821, #33625 ) ;
#23876 = ADVANCED_FACE ( 'NONE', ( #27550, #23837 ), #49947, .F. ) ;
#23877 = PLANE ( 'NONE',  #24036 ) ;
#23878 = DIRECTION ( 'NONE',  ( 0.005002170337468016433, -0.7660444431189770143, -0.6427681459581293666 ) ) ;
#23879 = CARTESIAN_POINT ( 'NONE',  ( -65.13378959736581919, -11.17687152541042295, -3.942473205280556670 ) ) ;
#23880 = ORIENTED_EDGE ( 'NONE', *, *, #13184, .F. ) ;
#23882 = EDGE_CURVE ( 'NONE', #48860, #44057, #35805, .T. ) ;
#23881 = DIRECTION ( 'NONE',  ( 0.005002170337468016433, -0.7660444431189770143, -0.6427681459581293666 ) ) ;
#23883 =( BOUNDED_CURVE ( )  B_SPLINE_CURVE ( 3, ( #30298, #13269, #8422, #17809 ),
 .UNSPECIFIED., .F., .F. ) 
 B_SPLINE_CURVE_WITH_KNOTS ( ( 4, 4 ),
 ( 5.142782291042174769, 6.283185307179586232 ),
 .UNSPECIFIED. ) 
 CURVE ( )  GEOMETRIC_REPRESENTATION_ITEM ( )  RATIONAL_B_SPLINE_CURVE ( ( 1.000000000000000000, 0.8945281452387645604, 0.8945281452387645604, 1.000000000000000000 ) ) 
 REPRESENTATION_ITEM ( '' )  );
#23884 = FACE_OUTER_BOUND ( 'NONE', #46196, .T. ) ;
#23885 = CARTESIAN_POINT ( 'NONE',  ( -68.21604434836798703, -0.6011028652887574486, 5.268187007956926848 ) ) ;
#23886 = EDGE_LOOP ( 'NONE', ( #32472, #23848, #4473, #8486 ) ) ;
#23887 = DIRECTION ( 'NONE',  ( 0.005002170337468016433, -0.7660444431189770143, -0.6427681459581293666 ) ) ;
#23889 = ADVANCED_FACE ( 'NONE', ( #31811 ), #40631, .F. ) ;
#23888 = LINE ( 'NONE', #15119, #46283 ) ;
#23890 = VECTOR ( 'NONE', #16132, 1000.000000000000000 ) ;
#23891 = EDGE_CURVE ( 'NONE', #21762, #39023, #40333, .T. ) ;
#23892 = DIRECTION ( 'NONE',  ( -0.9999697198139514409, -0.000000000000000000, -0.007781995580013368816 ) ) ;
#23893 = VECTOR ( 'NONE', #1759, 1000.000000000000227 ) ;
#23894 = DIRECTION ( 'NONE',  ( 0.005002170337468016433, -0.7660444431189770143, -0.6427681459581293666 ) ) ;
#23895 = LINE ( 'NONE', #41756, #40152 ) ;
#23896 = ORIENTED_EDGE ( 'NONE', *, *, #36940, .T. ) ;
#23897 = ORIENTED_EDGE ( 'NONE', *, *, #10886, .F. ) ;
#23898 = LINE ( 'NONE', #5755, #43154 ) ;
#23899 = VECTOR ( 'NONE', #42989, 999.9999999999998863 ) ;
#23900 = VECTOR ( 'NONE', #48689, 1000.000000000000227 ) ;
#23901 = CARTESIAN_POINT ( 'NONE',  ( -10.27421835998572064, 0.000000000000000000, 10.96090226820206048 ) ) ;
#23902 = VECTOR ( 'NONE', #45973, 999.9999999999998863 ) ;
#23903 = ORIENTED_EDGE ( 'NONE', *, *, #48168, .T. ) ;
#23904 = CARTESIAN_POINT ( 'NONE',  ( -14.83119343108531751, -0.5179957512181563306, 3.292990205337949394 ) ) ;
#23905 = EDGE_LOOP ( 'NONE', ( #54543, #24876, #31433, #5480 ) ) ;
#23906 = CARTESIAN_POINT ( 'NONE',  ( -14.56888064431065821, -0.1191753592594197858, 12.58947452739191064 ) ) ;
#23907 = ADVANCED_FACE ( 'NONE', ( #45413 ), #5991, .F. ) ;
#23908 = VECTOR ( 'NONE', #48910, 999.9999999999998863 ) ;
#23909 = ORIENTED_EDGE ( 'NONE', *, *, #8971, .F. ) ;
#23910 = VECTOR ( 'NONE', #24380, 1000.000000000000000 ) ;
#23911 = VERTEX_POINT ( 'NONE', #41463 ) ;
#23912 = DIRECTION ( 'NONE',  ( 0.007781995580012663651, -3.146120232559066537E-19, -0.9999697198139514409 ) ) ;
#23913 = EDGE_CURVE ( 'NONE', #33489, #56039, #53659, .T. ) ;
#23914 = CARTESIAN_POINT ( 'NONE',  ( -10.78835031468310746, -0.1191753592594185784, 4.467120647141804568 ) ) ;
#23915 = CARTESIAN_POINT ( 'NONE',  ( -15.82025578204862981, 0.000000000000000000, 7.113288712037448391 ) ) ;
#23916 = VERTEX_POINT ( 'NONE', #48863 ) ;
#23917 = CARTESIAN_POINT ( 'NONE',  ( -18.82375902897363318, 0.000000000000000000, 9.105901117897188257 ) ) ;
#23918 = EDGE_CURVE ( 'NONE', #40865, #7098, #53128, .T. ) ;
#23919 = ORIENTED_EDGE ( 'NONE', *, *, #38058, .F. ) ;
#23920 = EDGE_CURVE ( 'NONE', #15287, #40042, #1963, .T. ) ;
#23921 = ORIENTED_EDGE ( 'NONE', *, *, #33730, .F. ) ;
#23922 = ORIENTED_EDGE ( 'NONE', *, *, #26951, .T. ) ;
#23923 = CARTESIAN_POINT ( 'NONE',  ( -12.26038586170047040, -1.327505506330656893, 3.622944660148642360 ) ) ;
#23924 = AXIS2_PLACEMENT_3D ( 'NONE', #33008, #52004, #48027 ) ;
#23925 = ORIENTED_EDGE ( 'NONE', *, *, #55601, .F. ) ;
#23926 = CARTESIAN_POINT ( 'NONE',  ( -18.86354292863559579, 0.000000000000000000, 14.21804678658176080 ) ) ;
#23927 = VERTEX_POINT ( 'NONE', #32101 ) ;
#23928 = AXIS2_PLACEMENT_3D ( 'NONE', #28787, #54581, #46346 ) ;
#23929 = CARTESIAN_POINT ( 'NONE',  ( -8.609916609573598834, 0.000000000000000000, 10.23519010964256637 ) ) ;
#23930 = CARTESIAN_POINT ( 'NONE',  ( -20.54204810873173415, 0.000000000000000000, 4.860550213503115558 ) ) ;
#23931 = ORIENTED_EDGE ( 'NONE', *, *, #53591, .T. ) ;
#23932 = LINE ( 'NONE', #19108, #55766 ) ;
#23933 = VECTOR ( 'NONE', #15244, 999.9999999999998863 ) ;
#23934 = EDGE_LOOP ( 'NONE', ( #55241, #10617, #3545, #50239 ) ) ;
#23935 = EDGE_CURVE ( 'NONE', #33308, #3658, #22265, .T. ) ;
#23936 = DIRECTION ( 'NONE',  ( 0.007781995580012663651, -3.146120232559066537E-19, -0.9999697198139514409 ) ) ;
#23937 = CARTESIAN_POINT ( 'NONE',  ( -11.87243407472968926, 0.000000000000000000, 11.50246268866867361 ) ) ;
#23938 = PLANE ( 'NONE',  #30497 ) ;
#23939 = CARTESIAN_POINT ( 'NONE',  ( -14.63496119600401357, 0.000000000000000000, 8.230509157998767478 ) ) ;
#23940 = DIRECTION ( 'NONE',  ( 0.2426528472758542054, 0.7422098413412800966, 0.6246952433987894571 ) ) ;
#23941 = VECTOR ( 'NONE', #8867, 999.9999999999998863 ) ;
#23942 = DIRECTION ( 'NONE',  ( 0.007781995580012662783, 0.000000000000000000, -0.9999697198139514409 ) ) ;
#23943 = ORIENTED_EDGE ( 'NONE', *, *, #548, .T. ) ;
#23944 = VECTOR ( 'NONE', #31520, 1000.000000000000227 ) ;
#23945 = EDGE_LOOP ( 'NONE', ( #31952, #20193, #52375, #41026 ) ) ;
#23946 = CARTESIAN_POINT ( 'NONE',  ( -56.07727432805427981, 3.800000000000001155, 1.969340487120371019 ) ) ;
#23947 = PLANE ( 'NONE',  #21214 ) ;
#23948 = DIRECTION ( 'NONE',  ( 0.007781995580012663651, -3.146120232559066537E-19, -0.9999697198139514409 ) ) ;
#23949 = LINE ( 'NONE', #15697, #51444 ) ;
#23950 = AXIS2_PLACEMENT_3D ( 'NONE', #8710, #26032, #35369 ) ;
#23951 = AXIS2_PLACEMENT_3D ( 'NONE', #55253, #21480, #30267 ) ;
#23952 = LINE ( 'NONE', #37029, #42182 ) ;
#23953 = EDGE_LOOP ( 'NONE', ( #27996, #41051, #40055, #13725, #11295, #21261 ) ) ;
#23954 = LINE ( 'NONE', #2377, #13187 ) ;
#23955 = CARTESIAN_POINT ( 'NONE',  ( -17.63356496434233378, 4.172053068839010059, 3.398296866036514263 ) ) ;
#23956 = VERTEX_POINT ( 'NONE', #15064 ) ;
#23957 = CARTESIAN_POINT ( 'NONE',  ( -13.07066190154808361, 0.000000000000000000, 12.04713590736729678 ) ) ;
#23958 = DIRECTION ( 'NONE',  ( -0.5449076811759708816, 0.6444004775717707689, 0.5364919789714475140 ) ) ;
#23959 = ORIENTED_EDGE ( 'NONE', *, *, #50814, .F. ) ;
#23960 = CARTESIAN_POINT ( 'NONE',  ( -68.18492111507299569, 1.999999999999999556, 4.989023737097912914 ) ) ;
#23961 = CARTESIAN_POINT ( 'NONE',  ( -11.84011462117533320, 0.6102101463440047224, 1.261565443871230263 ) ) ;
#23962 = ADVANCED_FACE ( 'NONE', ( #19599 ), #45693, .F. ) ;
#23963 = DIRECTION ( 'NONE',  ( -0.7660212471507179544, -0.6427876096865405842, -0.005961354470445141482 ) ) ;
#23964 = FACE_OUTER_BOUND ( 'NONE', #36807, .T. ) ;
#23965 = CARTESIAN_POINT ( 'NONE',  ( -9.908141408373387193, -0.1191753592594197858, 10.77908512878318703 ) ) ;
#23966 = VECTOR ( 'NONE', #54249, 999.9999999999998863 ) ;
#23967 = EDGE_LOOP ( 'NONE', ( #41789, #24411, #46678, #14948 ) ) ;
#23968 = ORIENTED_EDGE ( 'NONE', *, *, #22579, .F. ) ;
#23969 = CARTESIAN_POINT ( 'NONE',  ( -19.60834386242827776, 0.000000000000000000, 4.298478389818581213 ) ) ;
#23970 = FACE_OUTER_BOUND ( 'NONE', #18626, .T. ) ;
#23971 = CARTESIAN_POINT ( 'NONE',  ( -11.89750579909570227, 0.1245042932765041271, 1.299354686050277818 ) ) ;
#23972 = VECTOR ( 'NONE', #38475, 999.9999999999998863 ) ;
#23973 = EDGE_CURVE ( 'NONE', #29009, #42993, #31555, .T. ) ;
#23974 = CARTESIAN_POINT ( 'NONE',  ( -22.24825055231656634, 5.143464774974011888, 13.96459914429588167 ) ) ;
#23975 = CARTESIAN_POINT ( 'NONE',  ( -17.50764612648356433, -1.489407457353158160, 3.634365539079154050 ) ) ;
#23976 = CARTESIAN_POINT ( 'NONE',  ( -20.54049170961573267, 0.000000000000000000, 4.660556269540326646 ) ) ;
#23978 = ADVANCED_FACE ( 'NONE', ( #6815 ), #20714, .F. ) ;
#23977 = ORIENTED_EDGE ( 'NONE', *, *, #21018, .F. ) ;
#23979 = DIRECTION ( 'NONE',  ( 0.6427681459581294776, -0.7660444431189769032, 0.005002170337467562802 ) ) ;
#23980 = EDGE_CURVE ( 'NONE', #32939, #18253, #46838, .T. ) ;
#23981 = PLANE ( 'NONE',  #3305 ) ;
#23982 = DIRECTION ( 'NONE',  ( -0.005002170337468016433, -0.7660444431189770143, 0.6427681459581293666 ) ) ;
#23984 = EDGE_LOOP ( 'NONE', ( #24579, #44284, #55122, #30087 ) ) ;
#23983 = VECTOR ( 'NONE', #18027, 999.9999999999998863 ) ;
#23985 = AXIS2_PLACEMENT_3D ( 'NONE', #28115, #6000, #24148 ) ;
#23986 = CARTESIAN_POINT ( 'NONE',  ( -45.73406441860519323, 4.435048094716153244, -5.000000000000000000 ) ) ;
#23987 = EDGE_CURVE ( 'NONE', #1435, #33297, #11636, .T. ) ;
#23988 = CARTESIAN_POINT ( 'NONE',  ( -24.27063949748155380, 0.000000000000000000, 6.308861732390097288 ) ) ;
#23989 = FACE_OUTER_BOUND ( 'NONE', #30281, .T. ) ;
#23990 = VECTOR ( 'NONE', #50197, 1000.000000000000114 ) ;
#23991 = ORIENTED_EDGE ( 'NONE', *, *, #31040, .T. ) ;
#23992 = CARTESIAN_POINT ( 'NONE',  ( -14.00280974873554030, 0.000000000000000000, 12.40921378708904044 ) ) ;
#23993 = EDGE_CURVE ( 'NONE', #6150, #52665, #46245, .T. ) ;
#23994 = ORIENTED_EDGE ( 'NONE', *, *, #6360, .T. ) ;
#23995 = EDGE_CURVE ( 'NONE', #54772, #9210, #42564, .T. ) ;
#23996 = VECTOR ( 'NONE', #32453, 1000.000000000000227 ) ;
#23997 = ORIENTED_EDGE ( 'NONE', *, *, #25858, .F. ) ;
#23998 = VERTEX_POINT ( 'NONE', #7946 ) ;
#23999 = VECTOR ( 'NONE', #11880, 1000.000000000000114 ) ;
#24000 = ORIENTED_EDGE ( 'NONE', *, *, #51959, .F. ) ;
#24001 = ORIENTED_EDGE ( 'NONE', *, *, #40054, .F. ) ;
#24002 = DIRECTION ( 'NONE',  ( -0.005002170337468016433, -0.7660444431189770143, 0.6427681459581293666 ) ) ;
#24003 = EDGE_LOOP ( 'NONE', ( #44897, #52313, #30479, #40771 ) ) ;
#24004 = ADVANCED_FACE ( 'NONE', ( #3655 ), #28679, .F. ) ;
#24005 = ORIENTED_EDGE ( 'NONE', *, *, #46510, .F. ) ;
#24006 = LINE ( 'NONE', #14935, #32214 ) ;
#24007 = ORIENTED_EDGE ( 'NONE', *, *, #1870, .F. ) ;
#24008 = EDGE_LOOP ( 'NONE', ( #50670, #12642, #29378, #17390 ) ) ;
#24009 = ORIENTED_EDGE ( 'NONE', *, *, #24577, .F. ) ;
#24010 = VECTOR ( 'NONE', #2234, 1000.000000000000227 ) ;
#24011 = ADVANCED_FACE ( 'NONE', ( #12180 ), #29213, .F. ) ;
#24012 = CARTESIAN_POINT ( 'NONE',  ( -23.33693525117809386, 0.000000000000000000, 5.746789908705562944 ) ) ;
#24013 = VECTOR ( 'NONE', #41187, 1000.000000000000227 ) ;
#24014 = CARTESIAN_POINT ( 'NONE',  ( -15.88053067323646417, -0.1191753592594197858, 2.950163842912994383 ) ) ;
#24015 = DIRECTION ( 'NONE',  ( 0.6427681459581294776, -0.7660444431189769032, 0.005002170337467562802 ) ) ;
#24016 = LINE ( 'NONE', #10705, #8737 ) ;
#24017 = EDGE_LOOP ( 'NONE', ( #2134, #22807, #47002, #11646 ) ) ;
#24018 = CARTESIAN_POINT ( 'NONE',  ( -14.93495759592298988, 0.000000000000000000, 12.77129166681078409 ) ) ;
#24019 = AXIS2_PLACEMENT_3D ( 'NONE', #20158, #45448, #46278 ) ;
#24020 = EDGE_LOOP ( 'NONE', ( #3334, #15396, #30969, #4681, #27166 ) ) ;
#24021 = ORIENTED_EDGE ( 'NONE', *, *, #28542, .F. ) ;
#24022 = CARTESIAN_POINT ( 'NONE',  ( -1.086233639165236964, 0.000000000000000000, -2.796443541562362078 ) ) ;
#24023 = DIRECTION ( 'NONE',  ( -0.5364919789714478471, 0.6444004775717705469, -0.5449076811759709926 ) ) ;
#24024 = AXIS2_PLACEMENT_3D ( 'NONE', #45189, #11377, #40655 ) ;
#24025 = DIRECTION ( 'NONE',  ( 0.000000000000000000, -1.000000000000000000, 0.000000000000000000 ) ) ;
#24026 = VECTOR ( 'NONE', #6096, 999.9999999999998863 ) ;
#24027 = AXIS2_PLACEMENT_3D ( 'NONE', #13969, #35290, #47493 ) ;
#24028 = LINE ( 'NONE', #36525, #35936 ) ;
#24029 = VECTOR ( 'NONE', #53386, 1000.000000000000227 ) ;
#24030 = CARTESIAN_POINT ( 'NONE',  ( -30.79567442779373110, 0.000000000000000000, 8.843406890442315316 ) ) ;
#24031 = AXIS2_PLACEMENT_3D ( 'NONE', #41788, #33310, #50613 ) ;
#24032 = FACE_OUTER_BOUND ( 'NONE', #29042, .T. ) ;
#24033 = VERTEX_POINT ( 'NONE', #42296 ) ;
#24034 = CARTESIAN_POINT ( 'NONE',  ( -13.53673582514181106, 0.000000000000000000, 12.22817484722816772 ) ) ;
#24035 = VERTEX_POINT ( 'NONE', #41991 ) ;
#24036 = AXIS2_PLACEMENT_3D ( 'NONE', #50830, #19338, #33266 ) ;
#24037 = CARTESIAN_POINT ( 'NONE',  ( -24.27063949748155380, 0.000000000000000000, 6.308861732390097288 ) ) ;
#24038 = DIRECTION ( 'NONE',  ( 0.007781995580012663651, 0.000000000000000000, -0.9999697198139515519 ) ) ;
#24039 = DIRECTION ( 'NONE',  ( -0.7660212471507179544, -0.6427876096865405842, -0.005961354470445141482 ) ) ;
#24040 = EDGE_CURVE ( 'NONE', #37024, #13654, #32919, .T. ) ;
#24041 = CARTESIAN_POINT ( 'NONE',  ( -9.482162182562110075, 0.000000000000000000, 2.899954397875381673 ) ) ;
#24042 = LINE ( 'NONE', #5600, #40479 ) ;
#24043 = VECTOR ( 'NONE', #149, 999.9999999999998863 ) ;
#24044 = VECTOR ( 'NONE', #21991, 999.9999999999998863 ) ;
#24045 = ORIENTED_EDGE ( 'NONE', *, *, #49822, .T. ) ;
#24046 = CARTESIAN_POINT ( 'NONE',  ( -28.93060053386082231, -0.1191753592594197858, 8.019254159017428663 ) ) ;
#24047 = CARTESIAN_POINT ( 'NONE',  ( -16.37867951088334451, 4.819660872929009798, 11.15324105243068686 ) ) ;
#24048 = CARTESIAN_POINT ( 'NONE',  ( -20.26041485802610609, 3.362543313726507499, 10.26966072999404034 ) ) ;
#24049 = EDGE_CURVE ( 'NONE', #1446, #9065, #46526, .T. ) ;
#24050 = EDGE_CURVE ( 'NONE', #17921, #35066, #20969, .T. ) ;
#24051 = EDGE_CURVE ( 'NONE', #7585, #48014, #7647, .T. ) ;
#24052 = CARTESIAN_POINT ( 'NONE',  ( -9.908141408373387193, -0.1191753592594197858, 10.77908512878318703 ) ) ;
#24053 = DIRECTION ( 'NONE',  ( 0.000000000000000000, -0.000000000000000000, -1.000000000000000000 ) ) ;
#24054 = CARTESIAN_POINT ( 'NONE',  ( -14.46888367232926420, 0.000000000000000000, 12.59025272694991315 ) ) ;
#24055 = DIRECTION ( 'NONE',  ( 0.007781995580012663651, -3.146120232559066537E-19, -0.9999697198139514409 ) ) ;
#24056 = EDGE_CURVE ( 'NONE', #52707, #33003, #43605, .T. ) ;
#24057 = AXIS2_PLACEMENT_3D ( 'NONE', #39647, #26280, #56112 ) ;
#24058 = PLANE ( 'NONE',  #46848 ) ;
#24059 = CARTESIAN_POINT ( 'NONE',  ( -19.60834386242827776, 0.000000000000000000, 4.298478389818581213 ) ) ;
#24060 = VECTOR ( 'NONE', #26980, 1000.000000000000227 ) ;
#24061 = ORIENTED_EDGE ( 'NONE', *, *, #34840, .T. ) ;
#24062 = EDGE_CURVE ( 'NONE', #35444, #34483, #55335, .T. ) ;
#24063 = VECTOR ( 'NONE', #18666, 1000.000000000000114 ) ;
#24064 = ADVANCED_FACE ( 'NONE', ( #52137 ), #16431, .F. ) ;
#24065 = ORIENTED_EDGE ( 'NONE', *, *, #32752, .F. ) ;
#24066 = ORIENTED_EDGE ( 'NONE', *, *, #24563, .F. ) ;
#24067 = AXIS2_PLACEMENT_3D ( 'NONE', #18797, #14797, #53155 ) ;
#24068 = VECTOR ( 'NONE', #42878, 999.9999999999998863 ) ;
#24069 = EDGE_LOOP ( 'NONE', ( #50735, #41886, #54804, #25765 ) ) ;
#24070 = EDGE_CURVE ( 'NONE', #23847, #33893, #29522, .T. ) ;
#24071 = VERTEX_POINT ( 'NONE', #25261 ) ;
#24072 = DIRECTION ( 'NONE',  ( -0.005002170337468016433, -0.7660444431189770143, 0.6427681459581293666 ) ) ;
#24073 = CARTESIAN_POINT ( 'NONE',  ( -18.67697421479882181, -0.1191753592594197858, 4.036397482078229793 ) ) ;
#24074 = VECTOR ( 'NONE', #32001, 999.9999999999998863 ) ;
#24075 = ADVANCED_FACE ( 'NONE', ( #38295 ), #37181, .F. ) ;
#24076 = VECTOR ( 'NONE', #45119, 999.9999999999998863 ) ;
#24077 = ORIENTED_EDGE ( 'NONE', *, *, #15911, .T. ) ;
#24078 = DIRECTION ( 'NONE',  ( -0.005002170337468016433, -0.7660444431189770143, 0.6427681459581293666 ) ) ;
#24079 = ORIENTED_EDGE ( 'NONE', *, *, #3224, .T. ) ;
#24080 = ORIENTED_EDGE ( 'NONE', *, *, #21623, .F. ) ;
#24081 = VECTOR ( 'NONE', #4645, 999.9999999999998863 ) ;
#24082 = AXIS2_PLACEMENT_3D ( 'NONE', #24441, #42037, #55120 ) ;
#24083 = CARTESIAN_POINT ( 'NONE',  ( -66.20463474764028433, -9.286562617286856280, -2.844731389947795286 ) ) ;
#24084 = CARTESIAN_POINT ( 'NONE',  ( -16.43317633868556626, -0.1191753592594197858, 13.31363028683540151 ) ) ;
#24085 = DIRECTION ( 'NONE',  ( 0.7660212471507180654, -0.6427876096865404731, 0.005961354470445141482 ) ) ;
#24086 = ORIENTED_EDGE ( 'NONE', *, *, #28948, .T. ) ;
#24087 = DIRECTION ( 'NONE',  ( -0.9983709377222390602, -0.05705673239519638146, 0.000000000000000000 ) ) ;
#24088 = LINE ( 'NONE', #41120, #92 ) ;
#24089 = LINE ( 'NONE', #38250, #27545 ) ;
#24090 = VECTOR ( 'NONE', #52542, 1000.000000000000114 ) ;
#24091 = DIRECTION ( 'NONE',  ( -0.005002170337468016433, -0.7660444431189770143, 0.6427681459581293666 ) ) ;
#24092 = PLANE ( 'NONE',  #5164 ) ;
#24093 = CARTESIAN_POINT ( 'NONE',  ( -19.60834386242827776, 0.000000000000000000, 4.298478389818581213 ) ) ;
#24094 = CARTESIAN_POINT ( 'NONE',  ( 2.072287782118878319, 0.000000000000000000, -2.950529333540147015 ) ) ;
#24096 = VECTOR ( 'NONE', #53227, 999.9999999999998863 ) ;
#24095 = LINE ( 'NONE', #2215, #17629 ) ;
#24097 = CARTESIAN_POINT ( 'NONE',  ( -14.39084381659288070, 3.038739411681508518, 7.458302638128849971 ) ) ;
#24098 = EDGE_LOOP ( 'NONE', ( #3501, #1659, #23909, #11602 ) ) ;
#24099 = PLANE ( 'NONE',  #51909 ) ;
#24100 = ORIENTED_EDGE ( 'NONE', *, *, #33107, .F. ) ;
#24101 = VECTOR ( 'NONE', #13825, 1000.000000000000114 ) ;
#24102 = EDGE_CURVE ( 'NONE', #17210, #17624, #15885, .T. ) ;
#24103 = LINE ( 'NONE', #6782, #34694 ) ;
#24104 = CARTESIAN_POINT ( 'NONE',  ( -13.38620395562085719, 0.7721120973665037690, 3.348144823107547463 ) ) ;
#24105 = DIRECTION ( 'NONE',  ( 0.007781995580012663651, 0.000000000000000000, -0.9999697198139515519 ) ) ;
#24106 = AXIS2_PLACEMENT_3D ( 'NONE', #22144, #31528, #52524 ) ;
#24107 = EDGE_CURVE ( 'NONE', #45238, #17332, #18625, .T. ) ;
#24108 = PLANE ( 'NONE',  #9647 ) ;
#24109 = LINE ( 'NONE', #15852, #23202 ) ;
#24110 = VECTOR ( 'NONE', #2224, 1000.000000000000227 ) ;
#24112 = AXIS2_PLACEMENT_3D ( 'NONE', #7753, #25081, #42395 ) ;
#24111 = DIRECTION ( 'NONE',  ( 0.000000000000000000, -1.000000000000000000, 0.000000000000000000 ) ) ;
#24113 = PLANE ( 'NONE',  #12010 ) ;
#24114 = CARTESIAN_POINT ( 'NONE',  ( 2.072287782118878319, 0.000000000000000000, -2.950529333540147015 ) ) ;
#24115 = FACE_OUTER_BOUND ( 'NONE', #18772, .T. ) ;
#24116 = VECTOR ( 'NONE', #17831, 1000.000000000000114 ) ;
#24117 = FACE_OUTER_BOUND ( 'NONE', #20010, .T. ) ;
#24118 = ADVANCED_FACE ( 'NONE', ( #9550 ), #10094, .F. ) ;
#24120 = VECTOR ( 'NONE', #50650, 1000.000000000000000 ) ;
#24119 = DIRECTION ( 'NONE',  ( 0.7660212471507180654, -0.6427876096865404731, 0.005961354470445141482 ) ) ;
#24121 = EDGE_CURVE ( 'NONE', #44182, #40596, #53286, .T. ) ;
#24122 = ADVANCED_FACE ( 'NONE', ( #1282 ), #44194, .F. ) ;
#24123 = VECTOR ( 'NONE', #1309, 1000.000000000000227 ) ;
#24124 = CARTESIAN_POINT ( 'NONE',  ( -31.72782227498118601, 0.000000000000000000, 9.205484770164058972 ) ) ;
#24125 = CARTESIAN_POINT ( 'NONE',  ( -20.42408051421004345, -0.5179957512181551094, 5.465457483668419769 ) ) ;
#24126 = ADVANCED_FACE ( 'NONE', ( #4715 ), #31956, .F. ) ;
#24127 = DIRECTION ( 'NONE',  ( -0.005002170337468016433, -0.7660444431189770143, 0.6427681459581293666 ) ) ;
#24128 = DIRECTION ( 'NONE',  ( -0.5364919789714478471, 0.6444004775717705469, -0.5449076811759709926 ) ) ;
#24129 = EDGE_LOOP ( 'NONE', ( #6692, #17244, #49031, #6531 ) ) ;
#24130 = VECTOR ( 'NONE', #41774, 1000.000000000000227 ) ;
#24132 = CARTESIAN_POINT ( 'NONE',  ( -13.73672976910459909, 0.000000000000000000, 12.22661844811216270 ) ) ;
#24131 = AXIS2_PLACEMENT_3D ( 'NONE', #13835, #196, #39705 ) ;
#24133 = EDGE_LOOP ( 'NONE', ( #34283, #39868, #40266, #8495 ) ) ;
#24134 = CARTESIAN_POINT ( 'NONE',  ( -24.27063949748155380, 0.000000000000000000, 6.308861732390097288 ) ) ;
#24135 = EDGE_LOOP ( 'NONE', ( #27217, #55434, #20065, #6588 ) ) ;
#24136 = ORIENTED_EDGE ( 'NONE', *, *, #37633, .T. ) ;
#24137 = CARTESIAN_POINT ( 'NONE',  ( -17.74404816805336793, 0.000000000000000000, 3.574322630375089460 ) ) ;
#24138 = EDGE_CURVE ( 'NONE', #37968, #50912, #1587, .T. ) ;
#24139 = VECTOR ( 'NONE', #24275, 1000.000000000000227 ) ;
#24140 = EDGE_CURVE ( 'NONE', #16305, #21974, #31111, .T. ) ;
#24141 = ORIENTED_EDGE ( 'NONE', *, *, #2184, .T. ) ;
#24142 = ORIENTED_EDGE ( 'NONE', *, *, #5168, .T. ) ;
#24143 = ORIENTED_EDGE ( 'NONE', *, *, #46873, .T. ) ;
#24144 = EDGE_CURVE ( 'NONE', #42632, #50731, #44730, .T. ) ;
#24145 = DIRECTION ( 'NONE',  ( -0.7660212471507179544, -0.6427876096865405842, -0.005961354470445141482 ) ) ;
#24146 = CARTESIAN_POINT ( 'NONE',  ( -15.60102546347950536, 0.000000000000000000, 12.95077420755565356 ) ) ;
#24147 = AXIS2_PLACEMENT_3D ( 'NONE', #33041, #36454, #24502 ) ;
#24148 = DIRECTION ( 'NONE',  ( -0.6427681459581293666, -0.7660444431189770143, -0.005002170337467561935 ) ) ;
#24149 = EDGE_CURVE ( 'NONE', #45990, #30666, #26870, .T. ) ;
#24150 = VECTOR ( 'NONE', #6737, 999.9999999999998863 ) ;
#24151 = ORIENTED_EDGE ( 'NONE', *, *, #48020, .T. ) ;
#24152 = EDGE_LOOP ( 'NONE', ( #7747, #7949, #39776, #41543 ) ) ;
#24153 = EDGE_CURVE ( 'NONE', #53959, #2345, #18322, .T. ) ;
#24154 = VECTOR ( 'NONE', #29782, 999.9999999999998863 ) ;
#24155 = CARTESIAN_POINT ( 'NONE',  ( -67.81626209598535127, 0.000000000000000000, 7.454917401049828918 ) ) ;
#24156 = DIRECTION ( 'NONE',  ( -0.5364919789714478471, 0.6444004775717705469, -0.5449076811759709926 ) ) ;
#24157 = ORIENTED_EDGE ( 'NONE', *, *, #20893, .T. ) ;
#24158 = DIRECTION ( 'NONE',  ( 0.007781995580012663651, -3.146120232559066537E-19, -0.9999697198139514409 ) ) ;
#24159 = VERTEX_POINT ( 'NONE', #48736 ) ;
#24160 = LINE ( 'NONE', #31827, #34844 ) ;
#24161 = DIRECTION ( 'NONE',  ( -0.9999697198139514409, -0.000000000000000000, -0.007781995580013368816 ) ) ;
#24162 = VECTOR ( 'NONE', #37434, 999.9999999999998863 ) ;
#24163 = EDGE_LOOP ( 'NONE', ( #42464, #18895, #44196, #38085 ) ) ;
#24164 = AXIS2_PLACEMENT_3D ( 'NONE', #45581, #11230, #28552 ) ;
#24165 = DIRECTION ( 'NONE',  ( 0.005961354470445682716, -0.6427876096865404731, -0.7660212471507180654 ) ) ;
#24166 = AXIS2_PLACEMENT_3D ( 'NONE', #53600, #1065, #23250 ) ;
#24167 = FACE_OUTER_BOUND ( 'NONE', #38096, .T. ) ;
#24168 = AXIS2_PLACEMENT_3D ( 'NONE', #48641, #53709, #35562 ) ;
#24169 = ORIENTED_EDGE ( 'NONE', *, *, #30548, .T. ) ;
#24170 = CARTESIAN_POINT ( 'NONE',  ( -14.02643832504429611, -0.1191753592594190225, 2.595260748476915236 ) ) ;
#24171 = CARTESIAN_POINT ( 'NONE',  ( -20.09634856977056927, -0.6798977022406551551, 5.603863950574907271 ) ) ;
#24172 = PLANE ( 'NONE',  #42831 ) ;
#24173 = ORIENTED_EDGE ( 'NONE', *, *, #50493, .F. ) ;
#24174 = CARTESIAN_POINT ( 'NONE',  ( -16.89925026227929195, -0.1191753592594197858, 13.49466922669627422 ) ) ;
#24175 = CARTESIAN_POINT ( 'NONE',  ( -10.00813838035478298, 0.000000000000000000, 10.77830692922518452 ) ) ;
#24176 = DIRECTION ( 'NONE',  ( -0.6427681459581293666, -0.7660444431189770143, -0.005002170337467561935 ) ) ;
#24177 = CARTESIAN_POINT ( 'NONE',  ( -13.27065584551087163, 0.000000000000000000, 12.04557950825129176 ) ) ;
#24178 = DIRECTION ( 'NONE',  ( -0.005961354470445682716, -0.6427876096865404731, 0.7660212471507180654 ) ) ;
#24179 = DIRECTION ( 'NONE',  ( 0.005002170337468016433, -0.7660444431189770143, -0.6427681459581293666 ) ) ;
#24180 = VECTOR ( 'NONE', #12027, 1000.000000000000227 ) ;
#24181 = DIRECTION ( 'NONE',  ( -0.6246952433987893460, -0.7422098413412802076, 0.2426528472758542054 ) ) ;
#24182 = ORIENTED_EDGE ( 'NONE', *, *, #45793, .F. ) ;
#24183 = FACE_OUTER_BOUND ( 'NONE', #30981, .T. ) ;
#24184 = CARTESIAN_POINT ( 'NONE',  ( -9.542064456761055524, 0.000000000000000000, 10.59726798936431180 ) ) ;
#24185 = CARTESIAN_POINT ( 'NONE',  ( -67.48059261034040901, -0.6012577534369748511, -3.373741216793211262 ) ) ;
#24186 = ORIENTED_EDGE ( 'NONE', *, *, #51522, .T. ) ;
#24187 = DIRECTION ( 'NONE',  ( -0.005002170337468016433, -0.7660444431189770143, 0.6427681459581293666 ) ) ;
#24188 = DIRECTION ( 'NONE',  ( 0.000000000000000000, -0.000000000000000000, -1.000000000000000000 ) ) ;
#24189 = ADVANCED_FACE ( 'NONE', ( #9838 ), #27141, .F. ) ;
#24190 = AXIS2_PLACEMENT_3D ( 'NONE', #19219, #1348, #49053 ) ;
#24191 = CARTESIAN_POINT ( 'NONE',  ( -3.033112459793370075, -5.745301166973593610, -2.040209691347345533 ) ) ;
#24192 = EDGE_CURVE ( 'NONE', #19093, #12718, #454, .T. ) ;
#24193 = ADVANCED_FACE ( 'NONE', ( #27408 ), #52429, .F. ) ;
#24194 = LINE ( 'NONE', #19909, #3331 ) ;
#24195 = CARTESIAN_POINT ( 'NONE',  ( -56.65661634607675978, 6.425189153618619642, 2.399912804366261643 ) ) ;
#24196 = ORIENTED_EDGE ( 'NONE', *, *, #12178, .T. ) ;
#24197 = VECTOR ( 'NONE', #54744, 1000.000000000000227 ) ;
#24198 = VERTEX_POINT ( 'NONE', #48140 ) ;
#24199 = DIRECTION ( 'NONE',  ( -0.7660212471507179544, -0.6427876096865405842, -0.005961354470445141482 ) ) ;
#24200 = DIRECTION ( 'NONE',  ( 0.9999697198139515519, 0.000000000000000000, 0.007781995580013368816 ) ) ;
#24201 = VECTOR ( 'NONE', #44767, 1000.000000000000114 ) ;
#24202 = ORIENTED_EDGE ( 'NONE', *, *, #42453, .F. ) ;
#24203 = LINE ( 'NONE', #2326, #23996 ) ;
#24204 = ORIENTED_EDGE ( 'NONE', *, *, #14393, .F. ) ;
#24205 = PLANE ( 'NONE',  #31979 ) ;
#24206 = AXIS2_PLACEMENT_3D ( 'NONE', #55385, #20176, #54531 ) ;
#24207 = VERTEX_POINT ( 'NONE', #35973 ) ;
#24208 = ORIENTED_EDGE ( 'NONE', *, *, #10082, .T. ) ;
#24209 = DIRECTION ( 'NONE',  ( 0.7660212471507180654, -0.6427876096865404731, 0.005961354470445141482 ) ) ;
#24210 = LINE ( 'NONE', #32172, #12384 ) ;
#24211 = DIRECTION ( 'NONE',  ( 0.9999697198139515519, 0.000000000000000000, 0.007781995580013368816 ) ) ;
#24212 = ORIENTED_EDGE ( 'NONE', *, *, #42402, .F. ) ;
#24213 = CARTESIAN_POINT ( 'NONE',  ( -22.69879496416571740, -4.889348428825663895, 5.542308122156290651 ) ) ;
#24214 = ORIENTED_EDGE ( 'NONE', *, *, #25153, .T. ) ;
#24215 = ADVANCED_FACE ( 'NONE', ( #5847 ), #9249, .F. ) ;
#24216 = VECTOR ( 'NONE', #22745, 1000.000000000000000 ) ;
#24217 = ORIENTED_EDGE ( 'NONE', *, *, #35450, .T. ) ;
#24218 = ORIENTED_EDGE ( 'NONE', *, *, #55919, .T. ) ;
#24219 = DIRECTION ( 'NONE',  ( 0.9999697198139515519, 0.000000000000000000, 0.007781995580013368816 ) ) ;
#24220 = EDGE_CURVE ( 'NONE', #29163, #21607, #31691, .T. ) ;
#24221 = ORIENTED_EDGE ( 'NONE', *, *, #1772, .T. ) ;
#24222 = PLANE ( 'NONE',  #6710 ) ;
#24223 = EDGE_CURVE ( 'NONE', #6114, #51035, #39662, .T. ) ;
#24224 = ORIENTED_EDGE ( 'NONE', *, *, #45554, .F. ) ;
#24225 = CARTESIAN_POINT ( 'NONE',  ( -12.45405610843340050, 0.7721120973665051013, 2.986066943385802475 ) ) ;
#24226 = DIRECTION ( 'NONE',  ( 0.007781995580012663651, 0.000000000000000000, -0.9999697198139515519 ) ) ;
#24227 = VERTEX_POINT ( 'NONE', #35380 ) ;
#24228 = VECTOR ( 'NONE', #43292, 1000.000000000000227 ) ;
#24229 = EDGE_CURVE ( 'NONE', #33221, #22744, #54629, .T. ) ;
#24230 = CARTESIAN_POINT ( 'NONE',  ( -56.70083583094844926, 4.876814673940706335, 2.999999999999993339 ) ) ;
#24231 = ORIENTED_EDGE ( 'NONE', *, *, #47402, .T. ) ;
#24232 = VECTOR ( 'NONE', #29658, 999.9999999999998863 ) ;
#24233 = DIRECTION ( 'NONE',  ( 0.000000000000000000, -1.000000000000000000, 0.000000000000000000 ) ) ;
#24234 = PLANE ( 'NONE',  #43828 ) ;
#24235 = CARTESIAN_POINT ( 'NONE',  ( -13.03530845450740117, 0.000000000000000000, 7.504293885903270400 ) ) ;
#24236 = DIRECTION ( 'NONE',  ( 0.6427681459581294776, -0.7660444431189769032, 0.005002170337467562802 ) ) ;
#24237 = FACE_OUTER_BOUND ( 'NONE', #54038, .T. ) ;
#24238 = DIRECTION ( 'NONE',  ( 0.005961354470445682716, -0.6427876096865404731, -0.7660212471507180654 ) ) ;
#24239 = APPLICATION_CONTEXT ( 'automotive_design' ) ;
#24240 = ORIENTED_EDGE ( 'NONE', *, *, #9361, .F. ) ;
#24241 = ORIENTED_EDGE ( 'NONE', *, *, #29640, .T. ) ;
#24242 = AXIS2_PLACEMENT_3D ( 'NONE', #34782, #13212, #21462 ) ;
#24243 = LINE ( 'NONE', #45804, #32790 ) ;
#24244 = LINE ( 'NONE', #42100, #16721 ) ;
#24245 = DIRECTION ( 'NONE',  ( 0.9999697198139515519, 0.000000000000000000, 0.007781995580013368816 ) ) ;
#24246 = LINE ( 'NONE', #32741, #22433 ) ;
#24247 = CARTESIAN_POINT ( 'NONE',  ( -17.39823374989226679, 0.000000000000000000, 5.054342117365806075 ) ) ;
#24248 = ORIENTED_EDGE ( 'NONE', *, *, #32043, .F. ) ;
#24249 = CARTESIAN_POINT ( 'NONE',  ( 2.072287782118878319, 0.000000000000000000, -2.950529333540147015 ) ) ;
#24250 = LINE ( 'NONE', #23955, #37729 ) ;
#24251 = ORIENTED_EDGE ( 'NONE', *, *, #18719, .F. ) ;
#24252 = DIRECTION ( 'NONE',  ( 0.5364919789714477361, 0.6444004775717706579, 0.5449076811759711036 ) ) ;
#24253 = EDGE_CURVE ( 'NONE', #10694, #31194, #32526, .T. ) ;
#24254 = LINE ( 'NONE', #24794, #3172 ) ;
#24255 = ORIENTED_EDGE ( 'NONE', *, *, #18563, .F. ) ;
#24256 = ADVANCED_FACE ( 'NONE', ( #45036 ), #28242, .F. ) ;
#24257 = DIRECTION ( 'NONE',  ( 0.7660212471507180654, -0.6427876096865404731, 0.005961354470445141482 ) ) ;
#24258 = CARTESIAN_POINT ( 'NONE',  ( -16.13159951105223655, 1.257817950434005461, 5.211675742713992143 ) ) ;
#24259 = PLANE ( 'NONE',  #12332 ) ;
#24260 = ADVANCED_FACE ( 'NONE', ( #11202 ), #28826, .F. ) ;
#24261 = EDGE_CURVE ( 'NONE', #16128, #49537, #50395, .T. ) ;
#24262 = PLANE ( 'NONE',  #31441 ) ;
#24263 = DIRECTION ( 'NONE',  ( 0.000000000000000000, -0.000000000000000000, -1.000000000000000000 ) ) ;
#24264 = ORIENTED_EDGE ( 'NONE', *, *, #25158, .T. ) ;
#24265 = ORIENTED_EDGE ( 'NONE', *, *, #12019, .F. ) ;
#24266 = DIRECTION ( 'NONE',  ( 0.007781995580012662783, 0.000000000000000000, -0.9999697198139514409 ) ) ;
#24267 = DIRECTION ( 'NONE',  ( 0.9999697198139515519, 0.000000000000000000, 0.007781995580013368816 ) ) ;
#24268 = PLANE ( 'NONE',  #43338 ) ;
#24269 = PLANE ( 'NONE',  #3374 ) ;
#24270 = DIRECTION ( 'NONE',  ( 0.9999697198139515519, 0.000000000000000000, 0.007781995580013368816 ) ) ;
#24271 = LINE ( 'NONE', #40487, #4997 ) ;
#24272 = EDGE_LOOP ( 'NONE', ( #41911, #21497, #51123, #46560 ) ) ;
#24273 = CARTESIAN_POINT ( 'NONE',  ( -11.26160937204003609, -0.1191753592594181482, 5.571433845147086394 ) ) ;
#24274 = ADVANCED_FACE ( 'NONE', ( #15212 ), #40766, .F. ) ;
#24276 = AXIS2_PLACEMENT_3D ( 'NONE', #28584, #45908, #7025 ) ;
#24275 = DIRECTION ( 'NONE',  ( -0.5449076811759708816, 0.6444004775717707689, 0.5364919789714475140 ) ) ;
#24277 = PLANE ( 'NONE',  #26031 ) ;
#24278 = EDGE_LOOP ( 'NONE', ( #19021, #18395, #15349, #39295 ) ) ;
#24279 = PLANE ( 'NONE',  #51014 ) ;
#24280 = CARTESIAN_POINT ( 'NONE',  ( -16.76996837579439870, 0.000000000000000000, 9.732398803345603255 ) ) ;
#24281 = DIRECTION ( 'NONE',  ( 0.7660212471507180654, -0.6427876096865404731, 0.005961354470445141482 ) ) ;
#24282 = ORIENTED_EDGE ( 'NONE', *, *, #54985, .F. ) ;
#24283 = VECTOR ( 'NONE', #48049, 1000.000000000000227 ) ;
#24284 = DIRECTION ( 'NONE',  ( -0.5449076811759708816, 0.6444004775717707689, 0.5364919789714475140 ) ) ;
#24285 = ORIENTED_EDGE ( 'NONE', *, *, #4133, .T. ) ;
#24286 = ORIENTED_EDGE ( 'NONE', *, *, #33568, .T. ) ;
#24287 = ORIENTED_EDGE ( 'NONE', *, *, #28489, .F. ) ;
#24288 = ORIENTED_EDGE ( 'NONE', *, *, #6842, .T. ) ;
#24289 = ORIENTED_EDGE ( 'NONE', *, *, #3977, .F. ) ;
#24290 = FACE_OUTER_BOUND ( 'NONE', #56120, .T. ) ;
#24291 = ORIENTED_EDGE ( 'NONE', *, *, #36014, .F. ) ;
#24292 = VERTEX_POINT ( 'NONE', #41324 ) ;
#24293 = DIRECTION ( 'NONE',  ( 0.5449076811759707706, 0.6444004775717708799, -0.5364919789714476250 ) ) ;
#24294 = EDGE_CURVE ( 'NONE', #6114, #2679, #36488, .T. ) ;
#24295 = ORIENTED_EDGE ( 'NONE', *, *, #31553, .T. ) ;
#24296 = ORIENTED_EDGE ( 'NONE', *, *, #52869, .T. ) ;
#24297 = LINE ( 'NONE', #28263, #33016 ) ;
#24298 = CARTESIAN_POINT ( 'NONE',  ( -15.27194367764935379, 3.524445264749008100, 8.597677798291803342 ) ) ;
#24299 = CARTESIAN_POINT ( 'NONE',  ( -15.99282684534787613, 0.000000000000000000, 3.587951039638777484 ) ) ;
#24300 = DIRECTION ( 'NONE',  ( 0.9999697198139515519, 0.000000000000000000, 0.007781995580013368816 ) ) ;
#24301 = ORIENTED_EDGE ( 'NONE', *, *, #27074, .T. ) ;
#24302 = ADVANCED_FACE ( 'NONE', ( #23989 ), #49574, .F. ) ;
#24303 = ORIENTED_EDGE ( 'NONE', *, *, #29190, .T. ) ;
#24304 = CARTESIAN_POINT ( 'NONE',  ( -11.72337221537584107, -0.1191753592594181482, 5.198508230121311691 ) ) ;
#24305 = DIRECTION ( 'NONE',  ( -0.005002170337468016433, -0.7660444431189770143, 0.6427681459581293666 ) ) ;
#24306 = EDGE_CURVE ( 'NONE', #33602, #52686, #6974, .T. ) ;
#24307 = EDGE_CURVE ( 'NONE', #31801, #14557, #10683, .T. ) ;
#24308 = CARTESIAN_POINT ( 'NONE',  ( -31.72626587586518099, 0.000000000000000000, 9.005490826201270949 ) ) ;
#24309 = LINE ( 'NONE', #10713, #23102 ) ;
#24310 = CARTESIAN_POINT ( 'NONE',  ( -14.13008755008897310, 0.000000000000000000, 3.063789224158076419 ) ) ;
#24311 = DIRECTION ( 'NONE',  ( -0.6246952433987894571, 0.7422098413412802076, 0.2426528472758539834 ) ) ;
#24312 = VERTEX_POINT ( 'NONE', #37315 ) ;
#24313 = PLANE ( 'NONE',  #52839 ) ;
#24314 = ADVANCED_FACE ( 'NONE', ( #2414 ), #49829, .F. ) ;
#24315 = ORIENTED_EDGE ( 'NONE', *, *, #35065, .F. ) ;
#24316 = VECTOR ( 'NONE', #43580, 999.9999999999998863 ) ;
#24317 = DIRECTION ( 'NONE',  ( -0.9999697198139514409, -0.000000000000000000, -0.007781995580013368816 ) ) ;
#24318 = PLANE ( 'NONE',  #46851 ) ;
#24319 = EDGE_CURVE ( 'NONE', #41524, #10050, #41590, .T. ) ;
#24320 = CARTESIAN_POINT ( 'NONE',  ( -13.94733792715787857, 0.000000000000000000, 5.281203842820665351 ) ) ;
#24321 = CARTESIAN_POINT ( 'NONE',  ( -19.60834386242827776, 0.000000000000000000, 4.298478389818581213 ) ) ;
#24322 = ADVANCED_FACE ( 'NONE', ( #23451 ), #19159, .F. ) ;
#24323 = LINE ( 'NONE', #41629, #22317 ) ;
#24324 = ORIENTED_EDGE ( 'NONE', *, *, #16183, .F. ) ;
#24325 = CARTESIAN_POINT ( 'NONE',  ( -18.58640238944216705, 0.000000000000000000, 4.306431374662254008 ) ) ;
#24326 = DIRECTION ( 'NONE',  ( 0.7660212471507180654, -0.6427876096865404731, 0.005961354470445141482 ) ) ;
#24327 = CARTESIAN_POINT ( 'NONE',  ( -19.42906346370737580, 0.000000000000000000, 7.623862219596294842 ) ) ;
#24328 = EDGE_CURVE ( 'NONE', #16476, #25539, #32779, .T. ) ;
#24329 = CARTESIAN_POINT ( 'NONE',  ( 2.072287782118878319, 0.000000000000000000, -2.950529333540147015 ) ) ;
#24330 = CARTESIAN_POINT ( 'NONE',  ( -1.086233639165236964, 0.000000000000000000, -2.796443541562362078 ) ) ;
#24331 = DIRECTION ( 'NONE',  ( 0.000000000000000000, -1.000000000000000000, 0.000000000000000000 ) ) ;
#24332 = DIRECTION ( 'NONE',  ( -0.7660212471507179544, -0.6427876096865405842, -0.005961354470445141482 ) ) ;
#24333 = ADVANCED_FACE ( 'NONE', ( #2672 ), #24533, .F. ) ;
#24334 = PLANE ( 'NONE',  #6978 ) ;
#24335 = DIRECTION ( 'NONE',  ( -0.5449076811759708816, 0.6444004775717707689, 0.5364919789714475140 ) ) ;
#24336 = ORIENTED_EDGE ( 'NONE', *, *, #29998, .T. ) ;
#24337 = ORIENTED_EDGE ( 'NONE', *, *, #7877, .T. ) ;
#24338 = VERTEX_POINT ( 'NONE', #32253 ) ;
#24339 = ORIENTED_EDGE ( 'NONE', *, *, #48909, .T. ) ;
#24340 = ORIENTED_EDGE ( 'NONE', *, *, #15378, .T. ) ;
#24341 = DIRECTION ( 'NONE',  ( 0.007781995580012663651, -3.146120232559066537E-19, -0.9999697198139514409 ) ) ;
#24342 = DIRECTION ( 'NONE',  ( -0.5364919789714478471, 0.6444004775717705469, -0.5449076811759709926 ) ) ;
#24343 = DIRECTION ( 'NONE',  ( 0.7660212471507180654, -0.6427876096865404731, 0.005961354470445141482 ) ) ;
#24344 = AXIS2_PLACEMENT_3D ( 'NONE', #25105, #33886, #42417 ) ;
#24345 = EDGE_LOOP ( 'NONE', ( #52439, #2256, #21978, #52688 ) ) ;
#24346 = CARTESIAN_POINT ( 'NONE',  ( -18.45093045568905410, 5.143464774974012776, 3.684796261400164141 ) ) ;
#24347 = EDGE_CURVE ( 'NONE', #41029, #48142, #45298, .T. ) ;
#24348 = ORIENTED_EDGE ( 'NONE', *, *, #15690, .T. ) ;
#24349 = CARTESIAN_POINT ( 'NONE',  ( -26.13493519185646008, 0.000000000000000000, 7.033017491833586377 ) ) ;
#24350 = VERTEX_POINT ( 'NONE', #12618 ) ;
#24351 = CARTESIAN_POINT ( 'NONE',  ( -65.98131617537119098, -9.260953737796825180, 1.428098984226591872 ) ) ;
#24352 = LINE ( 'NONE', #32342, #22835 ) ;
#24353 = LINE ( 'NONE', #19539, #11431 ) ;
#24354 = ORIENTED_EDGE ( 'NONE', *, *, #22062, .F. ) ;
#24355 = CARTESIAN_POINT ( 'NONE',  ( -69.66297551618575312, -8.676591480033549075, 7.503902134509970345 ) ) ;
#24356 = ORIENTED_EDGE ( 'NONE', *, *, #28065, .T. ) ;
#24357 = CARTESIAN_POINT ( 'NONE',  ( -10.89487359323307025, 0.000000000000000000, 5.304958826080728329 ) ) ;
#24358 = CARTESIAN_POINT ( 'NONE',  ( -16.01581927339013589, 0.000000000000000000, 6.542428665700890988 ) ) ;
#24359 = EDGE_CURVE ( 'NONE', #15067, #6267, #52065, .T. ) ;
#24360 = PLANE ( 'NONE',  #33571 ) ;
#24361 = CARTESIAN_POINT ( 'NONE',  ( -19.86075176232942496, 0.000000000000000000, 6.512506512018135574 ) ) ;
#24362 = CARTESIAN_POINT ( 'NONE',  ( -14.01545677930355183, 0.000000000000000000, 2.126011111488108174 ) ) ;
#24363 = CARTESIAN_POINT ( 'NONE',  ( -16.45933145549171428, 1.095915999411505082, 5.073269275807504641 ) ) ;
#24364 = CARTESIAN_POINT ( 'NONE',  ( -16.43317633868556626, -0.1191753592594197858, 13.31363028683540151 ) ) ;
#24365 = FACE_OUTER_BOUND ( 'NONE', #12716, .T. ) ;
#24366 = LINE ( 'NONE', #11852, #22047 ) ;
#24367 = ORIENTED_EDGE ( 'NONE', *, *, #26195, .F. ) ;
#24368 = DIRECTION ( 'NONE',  ( -0.6427681459581293666, -0.7660444431189770143, -0.005002170337467561935 ) ) ;
#24369 = ORIENTED_EDGE ( 'NONE', *, *, #31806, .F. ) ;
#24370 = CARTESIAN_POINT ( 'NONE',  ( -20.72814514249575168, 20.40220053346460460, 4.343046601168861542 ) ) ;
#24371 = LINE ( 'NONE', #50510, #54112 ) ;
#24372 = ADVANCED_FACE ( 'NONE', ( #25974 ), #37901, .F. ) ;
#24373 = CARTESIAN_POINT ( 'NONE',  ( -18.60031110817512356, 1.419719901456505395, 6.436315848785716831 ) ) ;
#24374 = DIRECTION ( 'NONE',  ( 0.005961354470445682716, -0.6427876096865404731, -0.7660212471507180654 ) ) ;
#24375 = LINE ( 'NONE', #32369, #28612 ) ;
#24376 = ADVANCED_FACE ( 'NONE', ( #29081 ), #7500, .F. ) ;
#24377 = CARTESIAN_POINT ( 'NONE',  ( -11.21979143729918960, -0.1191753592594197858, 1.139774444304266554 ) ) ;
#24378 = VERTEX_POINT ( 'NONE', #47530 ) ;
#24379 = DIRECTION ( 'NONE',  ( -0.6427681459581293666, -0.7660444431189770143, -0.005002170337467561935 ) ) ;
#24380 = DIRECTION ( 'NONE',  ( -0.5364919789714478471, 0.6444004775717705469, -0.5449076811759709926 ) ) ;
#24381 = CARTESIAN_POINT ( 'NONE',  ( -14.26863008609943329, 0.000000000000000000, 2.324046914494605875 ) ) ;
#24382 = DIRECTION ( 'NONE',  ( -0.5449076811759708816, 0.6444004775717707689, 0.5364919789714475140 ) ) ;
#24383 = CARTESIAN_POINT ( 'NONE',  ( -12.99351530631744289, 0.000000000000000000, 2.133964096331779636 ) ) ;
#24384 = EDGE_CURVE ( 'NONE', #15979, #48336, #33618, .T. ) ;
#24385 = COLOUR_RGB ( '', 0.31764706, 0.68627451, 0.89019608) ;
#24386 = DIRECTION ( 'NONE',  ( 0.000000000000000000, -0.000000000000000000, -1.000000000000000000 ) ) ;
#24387 = DIRECTION ( 'NONE',  ( -0.7660212471507179544, -0.6427876096865405842, -0.005961354470445141482 ) ) ;
#24388 = CARTESIAN_POINT ( 'NONE',  ( -23.33693525117809386, 0.000000000000000000, 5.746789908705562944 ) ) ;
#24389 = CARTESIAN_POINT ( 'NONE',  ( -9.856202467495650765, -0.1191753592594188005, 4.105042767420058247 ) ) ;
#24390 = EDGE_LOOP ( 'NONE', ( #8797, #54606, #18568, #30013, #30678, #33840 ) ) ;
#24391 = EDGE_CURVE ( 'NONE', #41524, #32862, #8643, .T. ) ;
#24392 = CARTESIAN_POINT ( 'NONE',  ( -16.79925329029790149, 0.000000000000000000, 13.49544742625427496 ) ) ;
#24393 = ORIENTED_EDGE ( 'NONE', *, *, #4263, .T. ) ;
#24394 = CARTESIAN_POINT ( 'NONE',  ( -32.65997012216863737, 0.000000000000000000, 9.567562649885804404 ) ) ;
#24395 = DIRECTION ( 'NONE',  ( 0.5449076811759707706, 0.6444004775717708799, -0.5364919789714476250 ) ) ;
#24396 = ORIENTED_EDGE ( 'NONE', *, *, #1288, .F. ) ;
#24397 = VERTEX_POINT ( 'NONE', #7812 ) ;
#24398 = DIRECTION ( 'NONE',  ( 0.007781995580012663651, -3.146120232559066537E-19, -0.9999697198139514409 ) ) ;
#24399 = ORIENTED_EDGE ( 'NONE', *, *, #18563, .T. ) ;
#24400 = ORIENTED_EDGE ( 'NONE', *, *, #2448, .T. ) ;
#24401 = ORIENTED_EDGE ( 'NONE', *, *, #33475, .T. ) ;
#24402 = DIRECTION ( 'NONE',  ( -0.5364919789714478471, 0.6444004775717705469, -0.5449076811759709926 ) ) ;
#24403 = CARTESIAN_POINT ( 'NONE',  ( -67.27731269685068582, -9.409571107119717226, -7.454891809856700746 ) ) ;
#24404 = CARTESIAN_POINT ( 'NONE',  ( -8.609916609573598834, 0.000000000000000000, 10.23519010964256637 ) ) ;
#24405 = EDGE_CURVE ( 'NONE', #45690, #46955, #34745, .T. ) ;
#24406 = ORIENTED_EDGE ( 'NONE', *, *, #48440, .T. ) ;
#24408 = ORIENTED_EDGE ( 'NONE', *, *, #7588, .T. ) ;
#24407 = ADVANCED_FACE ( 'NONE', ( #46979 ), #12034, .F. ) ;
#24409 = DIRECTION ( 'NONE',  ( 1.000000000000000000, 0.000000000000000000, -1.224646799147353207E-16 ) ) ;
#24410 = LINE ( 'NONE', #50251, #17291 ) ;
#24412 = EDGE_CURVE ( 'NONE', #45113, #36795, #37472, .T. ) ;
#24411 = ORIENTED_EDGE ( 'NONE', *, *, #47474, .F. ) ;
#24413 = FACE_OUTER_BOUND ( 'NONE', #38312, .T. ) ;
#24414 = ORIENTED_EDGE ( 'NONE', *, *, #39666, .T. ) ;
#24415 = FACE_OUTER_BOUND ( 'NONE', #54288, .T. ) ;
#24416 = CARTESIAN_POINT ( 'NONE',  ( -18.22254066414048168, -0.1191753592594167466, 4.409266058853649639 ) ) ;
#24417 = EDGE_CURVE ( 'NONE', #3505, #6678, #25132, .T. ) ;
#24418 = EDGE_CURVE ( 'NONE', #32474, #17347, #29370, .T. ) ;
#24419 = EDGE_CURVE ( 'NONE', #20494, #39433, #42009, .T. ) ;
#24420 = B_SPLINE_CURVE_WITH_KNOTS ( 'NONE', 3,
 ( #1943, #23288, #6505, #32621 ),
 .UNSPECIFIED., .F., .F.,
 ( 4, 4 ),
 ( 0.000000000000000000, 1.000000000000000000 ),
 .UNSPECIFIED. ) ;
#24421 = ORIENTED_EDGE ( 'NONE', *, *, #43307, .F. ) ;
#24422 = CARTESIAN_POINT ( 'NONE',  ( -9.878549426739102302, -0.06895642802817161798, 1.561684332249249296 ) ) ;
#24423 = DIRECTION ( 'NONE',  ( 0.000000000000000000, -0.000000000000000000, -1.000000000000000000 ) ) ;
#24424 = VERTEX_POINT ( 'NONE', #16885 ) ;
#24425 = PLANE ( 'NONE',  #7686 ) ;
#24426 = DIRECTION ( 'NONE',  ( -0.9999697198139514409, -0.000000000000000000, -0.007781995580013368816 ) ) ;
#24427 = CARTESIAN_POINT ( 'NONE',  ( -10.76535788664084592, -0.1191753592594202438, 1.512643021079689953 ) ) ;
#24428 = EDGE_LOOP ( 'NONE', ( #29302, #55049, #34261, #28506 ) ) ;
#24429 = LINE ( 'NONE', #41739, #19243 ) ;
#24430 = LINE ( 'NONE', #2297, #38701 ) ;
#24431 = CARTESIAN_POINT ( 'NONE',  ( -20.54049170961573267, 0.000000000000000000, 4.660556269540326646 ) ) ;
#24432 = ADVANCED_FACE ( 'NONE', ( #8081 ), #38750, .F. ) ;
#24433 = FACE_OUTER_BOUND ( 'NONE', #26286, .T. ) ;
#24434 = CARTESIAN_POINT ( 'NONE',  ( -20.54204810873173415, 0.000000000000000000, 4.860550213503115558 ) ) ;
#24436 = EDGE_CURVE ( 'NONE', #30300, #43916, #33912, .T. ) ;
#24435 = PLANE ( 'NONE',  #32477 ) ;
#24437 = ADVANCED_FACE ( 'NONE', ( #46687 ), #42696, .F. ) ;
#24438 = CARTESIAN_POINT ( 'NONE',  ( -68.96873366698683583, -11.61664068348967938, -7.382776467525443920 ) ) ;
#24439 = ORIENTED_EDGE ( 'NONE', *, *, #13362, .T. ) ;
#24440 = CARTESIAN_POINT ( 'NONE',  ( -15.23141738930936739, -2.622721114510659035, 6.902663673731017191 ) ) ;
#24441 = CARTESIAN_POINT ( 'NONE',  ( 2.072287782118878319, 0.000000000000000000, -2.950529333540147015 ) ) ;
#24442 = EDGE_CURVE ( 'NONE', #46093, #2126, #38446, .T. ) ;
#24443 = LINE ( 'NONE', #50581, #42305 ) ;
#24444 = ORIENTED_EDGE ( 'NONE', *, *, #29156, .F. ) ;
#24445 = DIRECTION ( 'NONE',  ( 0.9999697198139515519, 0.000000000000000000, 0.007781995580013368816 ) ) ;
#24446 = DIRECTION ( 'NONE',  ( -0.005002170337468016433, -0.7660444431189770143, 0.6427681459581293666 ) ) ;
#24447 = EDGE_CURVE ( 'NONE', #12870, #43988, #55474, .T. ) ;
#24448 = PLANE ( 'NONE',  #51270 ) ;
#24449 = LINE ( 'NONE', #41509, #28750 ) ;
#24450 = EDGE_CURVE ( 'NONE', #6826, #40411, #34216, .T. ) ;
#24451 = DIRECTION ( 'NONE',  ( 0.000000000000000000, 1.000000000000000000, 0.000000000000000000 ) ) ;
#24452 = ORIENTED_EDGE ( 'NONE', *, *, #36270, .T. ) ;
#24453 = ORIENTED_EDGE ( 'NONE', *, *, #6811, .F. ) ;
#24454 = DIRECTION ( 'NONE',  ( 0.005961354470445682716, -0.6427876096865404731, -0.7660212471507180654 ) ) ;
#24455 = DIRECTION ( 'NONE',  ( 0.005961354470445682716, -0.6427876096865404731, -0.7660212471507180654 ) ) ;
#24456 = LINE ( 'NONE', #9829, #32020 ) ;
#24457 = ORIENTED_EDGE ( 'NONE', *, *, #28909, .F. ) ;
#24458 = CARTESIAN_POINT ( 'NONE',  ( -15.50102849149811135, -0.1191753592594197858, 12.95155240711365430 ) ) ;
#24459 = ORIENTED_EDGE ( 'NONE', *, *, #5529, .F. ) ;
#24460 = CARTESIAN_POINT ( 'NONE',  ( -16.70641145532281868, 4.657758921906509642, 11.01483458552420025 ) ) ;
#24461 = EDGE_LOOP ( 'NONE', ( #305, #17327, #14491, #28269 ) ) ;
#24462 = VERTEX_POINT ( 'NONE', #35582 ) ;
#24463 = DIRECTION ( 'NONE',  ( -0.5364919789714478471, 0.6444004775717705469, -0.5449076811759709926 ) ) ;
#24464 = DIRECTION ( 'NONE',  ( 0.9999697198139515519, 0.000000000000000000, 0.007781995580013368816 ) ) ;
#24465 = DIRECTION ( 'NONE',  ( 0.5449076811759707706, 0.6444004775717708799, -0.5364919789714476250 ) ) ;
#24466 = VERTEX_POINT ( 'NONE', #35320 ) ;
#24467 = FACE_OUTER_BOUND ( 'NONE', #15431, .T. ) ;
#24468 = ORIENTED_EDGE ( 'NONE', *, *, #54193, .F. ) ;
#24469 = VERTEX_POINT ( 'NONE', #18252 ) ;
#24470 = EDGE_LOOP ( 'NONE', ( #12424, #43871, #13727, #50423 ) ) ;
#24471 = LINE ( 'NONE', #15152, #52215 ) ;
#24472 = DIRECTION ( 'NONE',  ( -0.6427681459581293666, -0.7660444431189770143, -0.005002170337467561935 ) ) ;
#24473 = EDGE_LOOP ( 'NONE', ( #6981, #22039, #34532, #52532 ) ) ;
#24474 = LINE ( 'NONE', #11443, #16671 ) ;
#24475 = VERTEX_POINT ( 'NONE', #14010 ) ;
#24476 = DIRECTION ( 'NONE',  ( -0.7660212471507179544, -0.6427876096865405842, -0.005961354470445141482 ) ) ;
#24477 = PLANE ( 'NONE',  #17757 ) ;
#24478 = EDGE_CURVE ( 'NONE', #38023, #5343, #52900, .T. ) ;
#24479 = EDGE_CURVE ( 'NONE', #8687, #15659, #22801, .T. ) ;
#24480 = ORIENTED_EDGE ( 'NONE', *, *, #27435, .F. ) ;
#24481 = LINE ( 'NONE', #11448, #40414 ) ;
#24482 = ORIENTED_EDGE ( 'NONE', *, *, #14264, .T. ) ;
#24483 = EDGE_CURVE ( 'NONE', #28250, #25448, #52617, .T. ) ;
#24484 = VECTOR ( 'NONE', #1921, 999.9999999999998863 ) ;
#24485 = CARTESIAN_POINT ( 'NONE',  ( -17.26532721389163072, 0.000000000000000000, 13.67648636611514590 ) ) ;
#24486 = DIRECTION ( 'NONE',  ( -0.9999697198139514409, -0.000000000000000000, -0.007781995580013368816 ) ) ;
#24487 = DIRECTION ( 'NONE',  ( -0.9999697198139514409, -0.000000000000000000, -0.007781995580013368816 ) ) ;
#24488 = CARTESIAN_POINT ( 'NONE',  ( -9.774228016103954531, 0.000000000000000000, 6.421676158506044452 ) ) ;
#24489 = LINE ( 'NONE', #12297, #14207 ) ;
#24490 = DIRECTION ( 'NONE',  ( 0.7660212471507180654, -0.6427876096865404731, 0.005961354470445141482 ) ) ;
#24491 = ORIENTED_EDGE ( 'NONE', *, *, #2873, .F. ) ;
#24492 = ORIENTED_EDGE ( 'NONE', *, *, #8095, .F. ) ;
#24493 = CARTESIAN_POINT ( 'NONE',  ( -18.51965916356675024, 5.143464774974010112, 12.51628762540889994 ) ) ;
#24494 = DIRECTION ( 'NONE',  ( -0.6246952433987893460, -0.7422098413412802076, 0.2426528472758542054 ) ) ;
#24495 = LINE ( 'NONE', #20543, #53972 ) ;
#24496 = DIRECTION ( 'NONE',  ( -0.5449076811759708816, 0.6444004775717707689, 0.5364919789714475140 ) ) ;
#24498 = EDGE_CURVE ( 'NONE', #23038, #22613, #39594, .T. ) ;
#24497 = LINE ( 'NONE', #6933, #690 ) ;
#24499 = CARTESIAN_POINT ( 'NONE',  ( -17.26532721389163072, 0.000000000000000000, 13.67648636611514590 ) ) ;
#24500 = ORIENTED_EDGE ( 'NONE', *, *, #15766, .T. ) ;
#24501 = LINE ( 'NONE', #55443, #53120 ) ;
#24502 = DIRECTION ( 'NONE',  ( 0.9335804264972044075, -0.3583679495452936070, 0.000000000000000000 ) ) ;
#24503 = ORIENTED_EDGE ( 'NONE', *, *, #53089, .F. ) ;
#24504 = CARTESIAN_POINT ( 'NONE',  ( -12.60008893460168622, 2.067327705546505801, 1.510275597055831698 ) ) ;
#24505 = DIRECTION ( 'NONE',  ( -0.005002170337468016433, -0.7660444431189770143, 0.6427681459581293666 ) ) ;
#24506 = VERTEX_POINT ( 'NONE', #53212 ) ;
#24507 = DIRECTION ( 'NONE',  ( 0.000000000000000000, -0.000000000000000000, -1.000000000000000000 ) ) ;
#24508 = LINE ( 'NONE', #41568, #21491 ) ;
#24509 = ADVANCED_FACE ( 'NONE', ( #48077 ), #43817, .F. ) ;
#24510 = CARTESIAN_POINT ( 'NONE',  ( -8.479536098004086142, -0.1191753592594181482, 6.331748722270672758 ) ) ;
#24511 = ADVANCED_FACE ( 'NONE', ( #14313 ), #26497, .F. ) ;
#24512 = LINE ( 'NONE', #8062, #33255 ) ;
#24513 = LINE ( 'NONE', #2920, #8374 ) ;
#24514 = VERTEX_POINT ( 'NONE', #48357 ) ;
#24515 = EDGE_CURVE ( 'NONE', #50834, #56081, #31033, .T. ) ;
#24516 = VERTEX_POINT ( 'NONE', #9183 ) ;
#24517 = PLANE ( 'NONE',  #23031 ) ;
#24518 = CARTESIAN_POINT ( 'NONE',  ( -9.542064456761055524, 0.000000000000000000, 10.59726798936431180 ) ) ;
#24519 = CARTESIAN_POINT ( 'NONE',  ( -10.77110599365141042, -0.1191753592594194527, 2.251262427595218885 ) ) ;
#24520 = EDGE_CURVE ( 'NONE', #44275, #53402, #5483, .T. ) ;
#24521 = CARTESIAN_POINT ( 'NONE',  ( -11.35220598394758262, 0.000000000000000000, 4.362729563834402136 ) ) ;
#24522 = DIRECTION ( 'NONE',  ( -0.9999697198139514409, -0.000000000000000000, -0.007781995580013368816 ) ) ;
#24523 = EDGE_CURVE ( 'NONE', #6407, #8862, #1515, .T. ) ;
#24524 = PLANE ( 'NONE',  #7705 ) ;
#24525 = ORIENTED_EDGE ( 'NONE', *, *, #13425, .T. ) ;
#24526 = FACE_OUTER_BOUND ( 'NONE', #50082, .T. ) ;
#24527 = VECTOR ( 'NONE', #18226, 1000.000000000000227 ) ;
#24528 = LINE ( 'NONE', #20272, #19600 ) ;
#24529 = CARTESIAN_POINT ( 'NONE',  ( -15.60102546347950536, 0.000000000000000000, 12.95077420755565356 ) ) ;
#24530 = ORIENTED_EDGE ( 'NONE', *, *, #34420, .T. ) ;
#24531 = FACE_OUTER_BOUND ( 'NONE', #45206, .T. ) ;
#24532 = DIRECTION ( 'NONE',  ( 0.005002170337468016433, -0.7660444431189770143, -0.6427681459581293666 ) ) ;
#24533 = PLANE ( 'NONE',  #55634 ) ;
#24534 = ORIENTED_EDGE ( 'NONE', *, *, #38328, .F. ) ;
#24535 = DIRECTION ( 'NONE',  ( 0.007781995580012662783, 0.000000000000000000, -0.9999697198139514409 ) ) ;
#24536 = ORIENTED_EDGE ( 'NONE', *, *, #11083, .F. ) ;
#24537 = ORIENTED_EDGE ( 'NONE', *, *, #12906, .T. ) ;
#24538 = ORIENTED_EDGE ( 'NONE', *, *, #4055, .F. ) ;
#24539 = ORIENTED_EDGE ( 'NONE', *, *, #49843, .F. ) ;
#24540 = SHAPE_REPRESENTATION ( 'Upper Lever Press Arm', ( #2610 ), #44334 ) ;
#24541 = VERTEX_POINT ( 'NONE', #48932 ) ;
#24542 = CARTESIAN_POINT ( 'NONE',  ( -10.79409842169367373, -0.1191753592594179401, 5.205740053657330613 ) ) ;
#24543 = ORIENTED_EDGE ( 'NONE', *, *, #22898, .F. ) ;
#24544 = EDGE_CURVE ( 'NONE', #33009, #24728, #13464, .T. ) ;
#24545 = VECTOR ( 'NONE', #50551, 999.9999999999998863 ) ;
#24546 = EDGE_LOOP ( 'NONE', ( #33842, #34085, #39319, #33770 ) ) ;
#24547 = CARTESIAN_POINT ( 'NONE',  ( -17.74404816805336793, 0.000000000000000000, 3.574322630375089460 ) ) ;
#24548 = ORIENTED_EDGE ( 'NONE', *, *, #47907, .T. ) ;
#24549 = VERTEX_POINT ( 'NONE', #18845 ) ;
#24550 = EDGE_CURVE ( 'NONE', #11444, #25938, #22541, .T. ) ;
#24551 = EDGE_CURVE ( 'NONE', #38228, #55983, #26791, .T. ) ;
#24552 = LINE ( 'NONE', #37336, #14909 ) ;
#24553 = DIRECTION ( 'NONE',  ( 0.5449076811759707706, 0.6444004775717708799, -0.5364919789714476250 ) ) ;
#24554 = CARTESIAN_POINT ( 'NONE',  ( -50.02554558092695913, 3.776013638374817294, 5.000000000000000000 ) ) ;
#24555 = CARTESIAN_POINT ( 'NONE',  ( -18.67697421479882181, -0.1191753592594197858, 4.036397482078229793 ) ) ;
#24556 = DIRECTION ( 'NONE',  ( 0.000000000000000000, -0.000000000000000000, -1.000000000000000000 ) ) ;
#24557 = ORIENTED_EDGE ( 'NONE', *, *, #46627, .T. ) ;
#24558 = VERTEX_POINT ( 'NONE', #30515 ) ;
#24559 = AXIS2_PLACEMENT_3D ( 'NONE', #20452, #23864, #41192 ) ;
#24560 = DIRECTION ( 'NONE',  ( -0.9321478471874540261, 0.000000000000000000, 0.3620778797217457656 ) ) ;
#24561 = CARTESIAN_POINT ( 'NONE',  ( 2.072287782118878319, 0.000000000000000000, -2.950529333540147015 ) ) ;
#24562 = UNCERTAINTY_MEASURE_WITH_UNIT (LENGTH_MEASURE( 1.000000000000000082E-05 ), #48842, 'distance_accuracy_value', 'NONE');
#24563 = EDGE_CURVE ( 'NONE', #31490, #54764, #47827, .T. ) ;
#24564 = VECTOR ( 'NONE', #31738, 1000.000000000000000 ) ;
#24565 = DIRECTION ( 'NONE',  ( 0.9999697198139515519, 0.000000000000000000, 0.007781995580013368816 ) ) ;
#24566 = CARTESIAN_POINT ( 'NONE',  ( -16.72210669506725722, 0.000000000000000000, 3.582275615218761367 ) ) ;
#24567 = CARTESIAN_POINT ( 'NONE',  ( -10.27421835998572064, 0.000000000000000000, 10.96090226820206048 ) ) ;
#24568 = LINE ( 'NONE', #54981, #52198 ) ;
#24569 = ORIENTED_EDGE ( 'NONE', *, *, #3652, .T. ) ;
#24570 = FACE_OUTER_BOUND ( 'NONE', #38743, .T. ) ;
#24571 = VERTEX_POINT ( 'NONE', #4646 ) ;
#24572 = DIRECTION ( 'NONE',  ( 0.5449076811759707706, 0.6444004775717708799, -0.5364919789714476250 ) ) ;
#24573 = DIRECTION ( 'NONE',  ( 0.000000000000000000, 0.000000000000000000, -1.000000000000000000 ) ) ;
#24574 = CARTESIAN_POINT ( 'NONE',  ( -15.13495153988577968, 0.000000000000000000, 12.76973526769478084 ) ) ;
#24575 = LINE ( 'NONE', #19782, #21786 ) ;
#24576 = FACE_OUTER_BOUND ( 'NONE', #36203, .T. ) ;
#24577 = EDGE_CURVE ( 'NONE', #7363, #1451, #21957, .T. ) ;
#24578 = CARTESIAN_POINT ( 'NONE',  ( -9.492340742193960068, 0.000000000000000000, 4.207877451611462760 ) ) ;
#24579 = ORIENTED_EDGE ( 'NONE', *, *, #38088, .F. ) ;
#24580 = EDGE_CURVE ( 'NONE', #20518, #51745, #375, .T. ) ;
#24581 = ORIENTED_EDGE ( 'NONE', *, *, #47901, .T. ) ;
#24582 = DIRECTION ( 'NONE',  ( -0.5364919789714478471, 0.6444004775717705469, -0.5449076811759709926 ) ) ;
#24583 = FACE_OUTER_BOUND ( 'NONE', #5440, .T. ) ;
#24584 = DIRECTION ( 'NONE',  ( 0.5449076811759707706, 0.6444004775717708799, -0.5364919789714476250 ) ) ;
#24585 = VECTOR ( 'NONE', #31170, 1000.000000000000000 ) ;
#24586 = AXIS2_PLACEMENT_3D ( 'NONE', #13599, #10179, #40588 ) ;
#24587 = DIRECTION ( 'NONE',  ( -0.9999697198139514409, -0.000000000000000000, -0.007781995580013368816 ) ) ;
#24588 = EDGE_CURVE ( 'NONE', #23847, #18842, #35059, .T. ) ;
#24589 = LINE ( 'NONE', #12943, #37572 ) ;
#24590 = CARTESIAN_POINT ( 'NONE',  ( -26.13337879274045505, 0.000000000000000000, 6.833023547870798353 ) ) ;
#24591 = FACE_OUTER_BOUND ( 'NONE', #6204, .T. ) ;
#24592 = CARTESIAN_POINT ( 'NONE',  ( -22.40478740399063895, 0.000000000000000000, 5.384712028983816623 ) ) ;
#24593 = PLANE ( 'NONE',  #53697 ) ;
#24594 = ADVANCED_FACE ( 'NONE', ( #32175 ), #27926, .F. ) ;
#24595 = ORIENTED_EDGE ( 'NONE', *, *, #53482, .T. ) ;
#24596 = EDGE_CURVE ( 'NONE', #32862, #33548, #11124, .T. ) ;
#24597 = EDGE_CURVE ( 'NONE', #14051, #11826, #19927, .T. ) ;
#24598 = VECTOR ( 'NONE', #49359, 999.9999999999998863 ) ;
#24599 = ORIENTED_EDGE ( 'NONE', *, *, #13460, .F. ) ;
#24600 = EDGE_LOOP ( 'NONE', ( #52115, #4111, #47967, #20274 ) ) ;
#24601 = VERTEX_POINT ( 'NONE', #49766 ) ;
#24602 = ORIENTED_EDGE ( 'NONE', *, *, #21695, .T. ) ;
#24603 = PLANE ( 'NONE',  #16023 ) ;
#24604 = CARTESIAN_POINT ( 'NONE',  ( -21.47419595591918906, 0.000000000000000000, 5.222628093224860102 ) ) ;
#24605 = ADVANCED_FACE ( 'NONE', ( #1769 ), #49193, .F. ) ;
#24606 = DIRECTION ( 'NONE',  ( -0.5449076811759708816, 0.6444004775717707689, 0.5364919789714475140 ) ) ;
#24608 = EDGE_CURVE ( 'NONE', #32882, #370, #36416, .T. ) ;
#24607 = ORIENTED_EDGE ( 'NONE', *, *, #16790, .T. ) ;
#24609 = EDGE_LOOP ( 'NONE', ( #19864, #11048, #24503, #7208 ) ) ;
#24610 = EDGE_LOOP ( 'NONE', ( #35663, #19877, #51547 ) ) ;
#24611 = DIRECTION ( 'NONE',  ( -0.2426528472758541499, 0.7422098413412800966, -0.6246952433987894571 ) ) ;
#24612 = ORIENTED_EDGE ( 'NONE', *, *, #50414, .T. ) ;
#24613 = ADVANCED_FACE ( 'NONE', ( #10613 ), #53728, .F. ) ;
#24614 = CARTESIAN_POINT ( 'NONE',  ( -67.99425556498525225, -9.491785959746023238, 8.455601507725486243 ) ) ;
#24615 = LINE ( 'NONE', #41114, #15561 ) ;
#24616 = CARTESIAN_POINT ( 'NONE',  ( -27.06552663992790997, 0.000000000000000000, 7.195101427592543786 ) ) ;
#24617 = VERTEX_POINT ( 'NONE', #27634 ) ;
#24618 = DIRECTION ( 'NONE',  ( 0.005961354470445682716, -0.6427876096865404731, -0.7660212471507180654 ) ) ;
#24619 = VERTEX_POINT ( 'NONE', #45482 ) ;
#24620 = ADVANCED_FACE ( 'NONE', ( #11428 ), #10312, .F. ) ;
#24621 = VECTOR ( 'NONE', #45912, 999.9999999999998863 ) ;
#24622 = VECTOR ( 'NONE', #23942, 1000.000000000000227 ) ;
#24623 = ADVANCED_FACE ( 'NONE', ( #2870 ), #23632, .F. ) ;
#24624 = CARTESIAN_POINT ( 'NONE',  ( -17.46532115785441519, 0.000000000000000000, 13.67492996699914265 ) ) ;
#24625 = DIRECTION ( 'NONE',  ( 0.007781995580012663651, -3.146120232559066537E-19, -0.9999697198139514409 ) ) ;
#24626 = EDGE_CURVE ( 'NONE', #24462, #9004, #6332, .T. ) ;
#24627 = CARTESIAN_POINT ( 'NONE',  ( -22.40478740399063895, 0.000000000000000000, 5.384712028983816623 ) ) ;
#24628 = VECTOR ( 'NONE', #8303, 1000.000000000000000 ) ;
#24629 = FACE_OUTER_BOUND ( 'NONE', #29525, .T. ) ;
#24630 = CARTESIAN_POINT ( 'NONE',  ( -13.17065887352947762, -0.1191753592594197858, 12.04635770780929427 ) ) ;
#24631 = DIRECTION ( 'NONE',  ( 0.007781995580012662783, 0.000000000000000000, -0.9999697198139514409 ) ) ;
#24632 = DIRECTION ( 'NONE',  ( 0.9999697198139515519, 0.000000000000000000, 0.007781995580013368816 ) ) ;
#24633 = LINE ( 'NONE', #32358, #51943 ) ;
#24634 = ORIENTED_EDGE ( 'NONE', *, *, #5590, .T. ) ;
#24635 = PLANE ( 'NONE',  #16565 ) ;
#24636 = VERTEX_POINT ( 'NONE', #23915 ) ;
#24637 = DIRECTION ( 'NONE',  ( -0.005002170337468016433, -0.7660444431189770143, 0.6427681459581293666 ) ) ;
#24638 = DIRECTION ( 'NONE',  ( -0.5449076811759708816, 0.6444004775717707689, 0.5364919789714475140 ) ) ;
#24639 = DIRECTION ( 'NONE',  ( 0.9999697198139515519, 0.000000000000000000, 0.007781995580013368816 ) ) ;
#24640 = VECTOR ( 'NONE', #14121, 1000.000000000000227 ) ;
#24641 = DIRECTION ( 'NONE',  ( 0.6427681459581294776, -0.7660444431189769032, 0.005002170337467562802 ) ) ;
#24642 = CARTESIAN_POINT ( 'NONE',  ( -20.54204810873173415, 0.000000000000000000, 4.860550213503115558 ) ) ;
#24643 = VECTOR ( 'NONE', #11718, 999.9999999999998863 ) ;
#24644 = CARTESIAN_POINT ( 'NONE',  ( -14.94760462649100496, 0.000000000000000000, 2.488088991209854051 ) ) ;
#24645 = CARTESIAN_POINT ( 'NONE',  ( -6.110905869601588769, 0.3662912372091372548, -5.334729614065428678E-16 ) ) ;
#24646 = ORIENTED_EDGE ( 'NONE', *, *, #55641, .F. ) ;
#24647 = DIRECTION ( 'NONE',  ( 0.007781995580012663651, -3.146120232559066537E-19, -0.9999697198139514409 ) ) ;
#24648 = LINE ( 'NONE', #50776, #42972 ) ;
#24649 = DIRECTION ( 'NONE',  ( -0.7660212471507179544, -0.6427876096865405842, -0.005961354470445141482 ) ) ;
#24650 = PLANE ( 'NONE',  #8242 ) ;
#24651 = CARTESIAN_POINT ( 'NONE',  ( -49.27554558092695913, 2.476975532698160620, 5.000000000000000000 ) ) ;
#24652 = DIRECTION ( 'NONE',  ( 0.007781995580012663651, -3.146120232559066537E-19, -0.9999697198139514409 ) ) ;
#24653 = EDGE_CURVE ( 'NONE', #14368, #41698, #36709, .T. ) ;
#24654 = CARTESIAN_POINT ( 'NONE',  ( -12.60458797795435615, 0.000000000000000000, 11.86609696750642229 ) ) ;
#24655 = PLANE ( 'NONE',  #15140 ) ;
#24656 = LINE ( 'NONE', #30057, #12020 ) ;
#24657 = ORIENTED_EDGE ( 'NONE', *, *, #26294, .F. ) ;
#24658 = DIRECTION ( 'NONE',  ( 0.007781995580012662783, 0.000000000000000000, -0.9999697198139514409 ) ) ;
#24659 = DIRECTION ( 'NONE',  ( -0.6427681459581293666, -0.7660444431189770143, -0.005002170337467561935 ) ) ;
#24660 = ORIENTED_EDGE ( 'NONE', *, *, #22339, .F. ) ;
#24661 = CARTESIAN_POINT ( 'NONE',  ( -20.54049170961573267, 0.000000000000000000, 4.660556269540326646 ) ) ;
#24662 = CARTESIAN_POINT ( 'NONE',  ( -16.81345671998191449, 0.000000000000000000, 3.412238694616132495 ) ) ;
#24663 = EDGE_CURVE ( 'NONE', #39497, #3767, #50311, .T. ) ;
#24664 = VECTOR ( 'NONE', #15201, 1000.000000000000114 ) ;
#24665 = VECTOR ( 'NONE', #45191, 999.9999999999998863 ) ;
#24666 = EDGE_LOOP ( 'NONE', ( #4713, #48756, #11956, #4574 ) ) ;
#24667 = ORIENTED_EDGE ( 'NONE', *, *, #33235, .T. ) ;
#24668 = DIRECTION ( 'NONE',  ( -0.5449076811759708816, 0.6444004775717707689, 0.5364919789714475140 ) ) ;
#24669 = EDGE_CURVE ( 'NONE', #23840, #8533, #54028, .T. ) ;
#24670 = EDGE_CURVE ( 'NONE', #33400, #7659, #45770, .T. ) ;
#24671 = VECTOR ( 'NONE', #23764, 1000.000000000000227 ) ;
#24672 = ORIENTED_EDGE ( 'NONE', *, *, #27842, .F. ) ;
#24673 = ORIENTED_EDGE ( 'NONE', *, *, #5023, .T. ) ;
#24674 = AXIS2_PLACEMENT_3D ( 'NONE', #23598, #44915, #10265 ) ;
#24675 = ORIENTED_EDGE ( 'NONE', *, *, #23987, .F. ) ;
#24676 = CARTESIAN_POINT ( 'NONE',  ( -15.60102546347950536, 0.000000000000000000, 12.95077420755565356 ) ) ;
#24677 = FACE_OUTER_BOUND ( 'NONE', #4650, .T. ) ;
#24678 = DIRECTION ( 'NONE',  ( 0.9999697198139515519, 0.000000000000000000, 0.007781995580013368816 ) ) ;
#24679 = ADVANCED_FACE ( 'NONE', ( #41775 ), #6897, .F. ) ;
#24680 = EDGE_LOOP ( 'NONE', ( #25550, #3943, #55828, #33444 ) ) ;
#24681 = AXIS2_PLACEMENT_3D ( 'NONE', #40452, #28195, #5801 ) ;
#24682 = ORIENTED_EDGE ( 'NONE', *, *, #19703, .F. ) ;
#24683 = EDGE_CURVE ( 'NONE', #18658, #43254, #31882, .T. ) ;
#24684 = CARTESIAN_POINT ( 'NONE',  ( -9.303843012252302813, 0.000000000000000000, 5.686672663758525204 ) ) ;
#24685 = DIRECTION ( 'NONE',  ( -0.5364919789714478471, 0.6444004775717705469, -0.5449076811759709926 ) ) ;
#24686 = EDGE_LOOP ( 'NONE', ( #39980, #48644, #11777, #45574 ) ) ;
#24687 = FACE_OUTER_BOUND ( 'NONE', #30141, .T. ) ;
#24688 = ORIENTED_EDGE ( 'NONE', *, *, #12515, .F. ) ;
#24689 = DIRECTION ( 'NONE',  ( -0.005961354470445682716, -0.6427876096865404731, 0.7660212471507180654 ) ) ;
#24690 = CARTESIAN_POINT ( 'NONE',  ( -19.79569077582305070, 0.000000000000000000, 14.58012466630350445 ) ) ;
#24691 = ADVANCED_FACE ( 'NONE', ( #14847 ), #40698, .F. ) ;
#24692 = ORIENTED_EDGE ( 'NONE', *, *, #40521, .F. ) ;
#24693 = FACE_OUTER_BOUND ( 'NONE', #45025, .T. ) ;
#24694 = AXIS2_PLACEMENT_3D ( 'NONE', #22315, #10362, #5823 ) ;
#24695 = EDGE_CURVE ( 'NONE', #23151, #52744, #12264, .T. ) ;
#24696 = DIRECTION ( 'NONE',  ( -0.005002170337468016433, -0.7660444431189770143, 0.6427681459581293666 ) ) ;
#24697 = ORIENTED_EDGE ( 'NONE', *, *, #22408, .T. ) ;
#24698 = FACE_OUTER_BOUND ( 'NONE', #27085, .T. ) ;
#24699 = VECTOR ( 'NONE', #7492, 1000.000000000000000 ) ;
#24700 = PLANE ( 'NONE',  #36473 ) ;
#24701 = EDGE_LOOP ( 'NONE', ( #4942, #52322, #38753, #56010 ) ) ;
#24702 = VECTOR ( 'NONE', #30348, 1000.000000000000114 ) ;
#24703 = VECTOR ( 'NONE', #48474, 1000.000000000000114 ) ;
#24704 = DIRECTION ( 'NONE',  ( 0.007781995580012663651, 0.000000000000000000, -0.9999697198139515519 ) ) ;
#24705 = CARTESIAN_POINT ( 'NONE',  ( -28.93137873341882127, 0.000000000000000000, 8.119251130998824451 ) ) ;
#24706 = DIRECTION ( 'NONE',  ( -0.6427681459581293666, -0.7660444431189770143, -0.005002170337467561935 ) ) ;
#24707 = PLANE ( 'NONE',  #32271 ) ;
#24708 = CARTESIAN_POINT ( 'NONE',  ( -28.93137873341882127, 0.000000000000000000, 8.119251130998824451 ) ) ;
#24709 = DIRECTION ( 'NONE',  ( 0.007781995580012663651, -3.146120232559066537E-19, -0.9999697198139514409 ) ) ;
#24710 = VECTOR ( 'NONE', #9045, 999.9999999999998863 ) ;
#24711 = DIRECTION ( 'NONE',  ( 0.9999697198139515519, 0.000000000000000000, 0.007781995580013368816 ) ) ;
#24712 = AXIS2_PLACEMENT_3D ( 'NONE', #25234, #3369, #21539 ) ;
#24713 = ORIENTED_EDGE ( 'NONE', *, *, #3961, .F. ) ;
#24714 = CARTESIAN_POINT ( 'NONE',  ( -21.47419595591918906, 0.000000000000000000, 5.222628093224860102 ) ) ;
#24715 = LINE ( 'NONE', #11396, #41319 ) ;
#24716 = CARTESIAN_POINT ( 'NONE',  ( -68.30214028159727491, 2.081668171172168513E-14, 8.159882300546032141 ) ) ;
#24717 = EDGE_LOOP ( 'NONE', ( #40903, #21965, #1960, #50790 ) ) ;
#24718 = CARTESIAN_POINT ( 'NONE',  ( -18.67619601524082285, 0.000000000000000000, 3.936400510096834893 ) ) ;
#24719 = CARTESIAN_POINT ( 'NONE',  ( -26.13337879274045505, 0.000000000000000000, 6.833023547870798353 ) ) ;
#24720 = CARTESIAN_POINT ( 'NONE',  ( -15.13495153988577968, 0.000000000000000000, 12.76973526769478084 ) ) ;
#24721 = VECTOR ( 'NONE', #32356, 1000.000000000000227 ) ;
#24722 = EDGE_CURVE ( 'NONE', #9919, #51258, #37534, .T. ) ;
#24723 = AXIS2_PLACEMENT_3D ( 'NONE', #48665, #10864, #54032 ) ;
#24724 = DIRECTION ( 'NONE',  ( -0.5449076811759708816, 0.6444004775717707689, 0.5364919789714475140 ) ) ;
#24725 = CARTESIAN_POINT ( 'NONE',  ( -6.110905869600904872, 1.712176620043476140E-14, 3.600000000000000089 ) ) ;
#24726 = ORIENTED_EDGE ( 'NONE', *, *, #4274, .T. ) ;
#24727 = EDGE_CURVE ( 'NONE', #23468, #18912, #4023, .T. ) ;
#24728 = VERTEX_POINT ( 'NONE', #21043 ) ;
#24729 = ADVANCED_FACE ( 'NONE', ( #34141 ), #29869, .F. ) ;
#24730 = DIRECTION ( 'NONE',  ( 0.9999697198139515519, 0.000000000000000000, 0.007781995580013368816 ) ) ;
#24731 = EDGE_CURVE ( 'NONE', #5706, #45380, #38677, .T. ) ;
#24732 = VECTOR ( 'NONE', #2138, 1000.000000000000114 ) ;
#24733 = EDGE_CURVE ( 'NONE', #3673, #22994, #21347, .T. ) ;
#24734 = EDGE_CURVE ( 'NONE', #5052, #43426, #25057, .T. ) ;
#24735 = DIRECTION ( 'NONE',  ( -0.000000000000000000, -0.000000000000000000, -1.000000000000000000 ) ) ;
#24736 = ORIENTED_EDGE ( 'NONE', *, *, #8488, .F. ) ;
#24737 = DIRECTION ( 'NONE',  ( 0.005002170337468016433, -0.7660444431189770143, -0.6427681459581293666 ) ) ;
#24738 = AXIS2_PLACEMENT_3D ( 'NONE', #46045, #44934, #19910 ) ;
#24739 = VERTEX_POINT ( 'NONE', #33835 ) ;
#24740 = LINE ( 'NONE', #46054, #9346 ) ;
#24741 = ORIENTED_EDGE ( 'NONE', *, *, #35662, .T. ) ;
#24742 = ORIENTED_EDGE ( 'NONE', *, *, #5545, .F. ) ;
#24743 = ORIENTED_EDGE ( 'NONE', *, *, #52743, .T. ) ;
#24744 = CARTESIAN_POINT ( 'NONE',  ( -14.93495759592298988, 0.000000000000000000, 12.77129166681078409 ) ) ;
#24745 = VECTOR ( 'NONE', #20498, 1000.000000000000227 ) ;
#24746 = PLANE ( 'NONE',  #23244 ) ;
#24747 = DIRECTION ( 'NONE',  ( -0.5364919789714478471, 0.6444004775717705469, -0.5449076811759709926 ) ) ;
#24748 = AXIS2_PLACEMENT_3D ( 'NONE', #46211, #41130, #55048 ) ;
#24749 = VECTOR ( 'NONE', #42877, 1000.000000000000227 ) ;
#24750 = CARTESIAN_POINT ( 'NONE',  ( -12.33850799832341849, 0.000000000000000000, 11.68350162852954632 ) ) ;
#24751 = EDGE_CURVE ( 'NONE', #20238, #31826, #29604, .T. ) ;
#24752 = ORIENTED_EDGE ( 'NONE', *, *, #1067, .T. ) ;
#24754 = EDGE_LOOP ( 'NONE', ( #52083, #16961, #45478, #25216 ) ) ;
#24753 = EDGE_CURVE ( 'NONE', #28378, #54423, #17091, .T. ) ;
#24755 = VECTOR ( 'NONE', #38442, 999.9999999999998863 ) ;
#24756 = VERTEX_POINT ( 'NONE', #12555 ) ;
#24757 = LINE ( 'NONE', #3180, #46736 ) ;
#24758 = VECTOR ( 'NONE', #13690, 999.9999999999998863 ) ;
#24759 = B_SPLINE_CURVE_WITH_KNOTS ( 'NONE', 3,
 ( #55086, #46251, #54783, #7654, #11643, #42569, #54490, #33760, #3662, #38035, #50801, #38302, #32926, #46005, #55343, #55622, #34067, #50243, #7111, #24403 ),
 .UNSPECIFIED., .F., .F.,
 ( 4, 2, 2, 2, 2, 2, 2, 2, 2, 4 ),
 ( 6.071532165918829453E-18, 0.001980665692890086396, 0.003961331385780166719, 0.005941997078670247477, 0.006932329925115283085, 0.007922662771560321296, 0.009903328464450394247, 0.01188399415734046893, 0.01386465985023054015, 0.01584532554312061484 ),
 .UNSPECIFIED. ) ;
#24760 = CARTESIAN_POINT ( 'NONE',  ( -22.40634380310664397, 0.000000000000000000, 5.584705972946605534 ) ) ;
#24761 = ADVANCED_FACE ( 'NONE', ( #43226 ), #47166, .F. ) ;
#24762 = ORIENTED_EDGE ( 'NONE', *, *, #29334, .T. ) ;
#24763 = FACE_BOUND ( 'NONE', #50540, .T. ) ;
#24764 = EDGE_LOOP ( 'NONE', ( #40469, #24856, #16054, #21197 ) ) ;
#24765 = CARTESIAN_POINT ( 'NONE',  ( -23.66772770479517618, 18.99370688441070953, -4.657437592157546824 ) ) ;
#24766 = DIRECTION ( 'NONE',  ( 0.007781995580012662783, 0.000000000000000000, -0.9999697198139514409 ) ) ;
#24767 = EDGE_CURVE ( 'NONE', #33148, #28250, #51708, .T. ) ;
#24768 = VERTEX_POINT ( 'NONE', #37836 ) ;
#24770 = AXIS2_PLACEMENT_3D ( 'NONE', #5103, #27221, #52766 ) ;
#24769 = CARTESIAN_POINT ( 'NONE',  ( 2.072287782118878319, 0.000000000000000000, -2.950529333540147015 ) ) ;
#24771 = ORIENTED_EDGE ( 'NONE', *, *, #9383, .F. ) ;
#24772 = VECTOR ( 'NONE', #15814, 1000.000000000000227 ) ;
#24773 = CARTESIAN_POINT ( 'NONE',  ( -14.20280369269832832, 0.000000000000000000, 12.40765738797303719 ) ) ;
#24774 = DIRECTION ( 'NONE',  ( -0.8531650599175527594, 0.4028455766673922356, 0.3313982828793700652 ) ) ;
#24775 = LINE ( 'NONE', #42090, #12372 ) ;
#24776 = FACE_OUTER_BOUND ( 'NONE', #37619, .T. ) ;
#24777 = CARTESIAN_POINT ( 'NONE',  ( -19.71756863920010616, -1.327505506330655782, 6.519567697922603600 ) ) ;
#24778 = DIRECTION ( 'NONE',  ( 0.005961354470445682716, -0.6427876096865404731, -0.7660212471507180654 ) ) ;
#24779 = VERTEX_POINT ( 'NONE', #16234 ) ;
#24780 = VECTOR ( 'NONE', #51797, 999.9999999999998863 ) ;
#24781 = VERTEX_POINT ( 'NONE', #8272 ) ;
#24782 = DIRECTION ( 'NONE',  ( -0.1139275668495183524, 0.9934890585767659488, 4.694855797473117491E-16 ) ) ;
#24783 = PLANE ( 'NONE',  #52959 ) ;
#24784 = VECTOR ( 'NONE', #52050, 1000.000000000000227 ) ;
#24785 = CARTESIAN_POINT ( 'NONE',  ( -18.80686481966623802, -4.079838673713161334, 10.68286703394162629 ) ) ;
#24786 = DIRECTION ( 'NONE',  ( 0.007781995580012662783, 0.000000000000000000, -0.9999697198139514409 ) ) ;
#24787 = DIRECTION ( 'NONE',  ( 0.000000000000000000, -0.000000000000000000, -1.000000000000000000 ) ) ;
#24788 = CARTESIAN_POINT ( 'NONE',  ( -10.47421230394850866, 0.000000000000000000, 10.95934586908605723 ) ) ;
#24789 = ORIENTED_EDGE ( 'NONE', *, *, #45270, .T. ) ;
#24790 = CARTESIAN_POINT ( 'NONE',  ( -16.00432305936900690, 0.000000000000000000, 5.065189852669833570 ) ) ;
#24791 = LINE ( 'NONE', #9150, #8723 ) ;
#24792 = ORIENTED_EDGE ( 'NONE', *, *, #17873, .F. ) ;
#24793 = AXIS2_PLACEMENT_3D ( 'NONE', #26571, #43892, #14378 ) ;
#24794 = CARTESIAN_POINT ( 'NONE',  ( -11.77243710274829525, -0.1191753592594197858, 11.50324088822667612 ) ) ;
#24795 = EDGE_LOOP ( 'NONE', ( #2277, #53105, #34463, #9999, #2936 ) ) ;
#24796 = VECTOR ( 'NONE', #30740, 1000.000000000000000 ) ;
#24797 = CIRCLE ( 'NONE', #29345, 6.000000000000001776 ) ;
#24798 = CARTESIAN_POINT ( 'NONE',  ( -16.81267852042391198, -0.1191753592594197858, 3.312241722634738039 ) ) ;
#24799 = CARTESIAN_POINT ( 'NONE',  ( -14.20280369269832832, 0.000000000000000000, 12.40765738797303719 ) ) ;
#24800 = EDGE_CURVE ( 'NONE', #41133, #43762, #33301, .T. ) ;
#24801 = DIRECTION ( 'NONE',  ( 0.5449076811759707706, 0.6444004775717708799, -0.5364919789714476250 ) ) ;
#24802 = CARTESIAN_POINT ( 'NONE',  ( 2.072287782118878319, 0.000000000000000000, -2.950529333540147015 ) ) ;
#24803 = CARTESIAN_POINT ( 'NONE',  ( -69.06384020419240244, 0.1330099063031576490, -6.182688104192161305 ) ) ;
#24804 = ORIENTED_EDGE ( 'NONE', *, *, #20620, .F. ) ;
#24805 = VECTOR ( 'NONE', #38947, 1000.000000000000227 ) ;
#24806 = EDGE_CURVE ( 'NONE', #9324, #55008, #8567, .T. ) ;
#24807 = VECTOR ( 'NONE', #9034, 1000.000000000000227 ) ;
#24808 = ORIENTED_EDGE ( 'NONE', *, *, #4604, .T. ) ;
#24809 = LINE ( 'NONE', #29355, #29434 ) ;
#24810 = DIRECTION ( 'NONE',  ( 0.005961354470445682716, -0.6427876096865404731, -0.7660212471507180654 ) ) ;
#24811 = LINE ( 'NONE', #6959, #45116 ) ;
#24812 = ADVANCED_FACE ( 'NONE', ( #15964 ), #20777, .F. ) ;
#24813 = EDGE_CURVE ( 'NONE', #27552, #25905, #29017, .T. ) ;
#24814 = EDGE_CURVE ( 'NONE', #10480, #7041, #11959, .T. ) ;
#24815 = CARTESIAN_POINT ( 'NONE',  ( -16.79925329029790149, 0.000000000000000000, 13.49544742625427496 ) ) ;
#24816 = FACE_OUTER_BOUND ( 'NONE', #48324, .T. ) ;
#24817 = LINE ( 'NONE', #33063, #9488 ) ;
#24819 = EDGE_CURVE ( 'NONE', #23263, #53826, #16806, .T. ) ;
#24818 = ORIENTED_EDGE ( 'NONE', *, *, #46781, .T. ) ;
#24820 = DIRECTION ( 'NONE',  ( -0.5449076811759708816, 0.6444004775717707689, 0.5364919789714475140 ) ) ;
#24821 = DIRECTION ( 'NONE',  ( -0.9999697198139514409, -0.000000000000000000, -0.007781995580013368816 ) ) ;
#24822 = CARTESIAN_POINT ( 'NONE',  ( -14.01623497886158454, -0.1191753592594203132, 2.226008083469503518 ) ) ;
#24823 = ORIENTED_EDGE ( 'NONE', *, *, #22475, .F. ) ;
#24824 = VECTOR ( 'NONE', #56076, 999.9999999999998863 ) ;
#24825 = CARTESIAN_POINT ( 'NONE',  ( -12.26291780220878103, 0.000000000000000000, 1.970323761456820755 ) ) ;
#24826 = CARTESIAN_POINT ( 'NONE',  ( -61.38973930853472183, 7.404220597074748333, 2.999999999999993339 ) ) ;
#24827 = AXIS2_PLACEMENT_3D ( 'NONE', #56153, #4208, #26600 ) ;
#24828 = DIRECTION ( 'NONE',  ( -0.005961354470445682716, -0.6427876096865404731, 0.7660212471507180654 ) ) ;
#24829 = ORIENTED_EDGE ( 'NONE', *, *, #27536, .T. ) ;
#24830 = DIRECTION ( 'NONE',  ( 0.005002170337468016433, -0.7660444431189770143, -0.6427681459581293666 ) ) ;
#24831 = AXIS2_PLACEMENT_3D ( 'NONE', #9871, #22912, #45597 ) ;
#24832 = EDGE_LOOP ( 'NONE', ( #47253, #10092, #8623, #15961 ) ) ;
#24833 = ADVANCED_FACE ( 'NONE', ( #17939 ), #9702, .T. ) ;
#24834 = VERTEX_POINT ( 'NONE', #13932 ) ;
#24835 = EDGE_LOOP ( 'NONE', ( #32272, #5929, #40203, #13945 ) ) ;
#24836 = ADVANCED_FACE ( 'NONE', ( #18472 ), #13405, .F. ) ;
#24837 = ORIENTED_EDGE ( 'NONE', *, *, #15351, .F. ) ;
#24838 = VECTOR ( 'NONE', #3173, 1000.000000000000227 ) ;
#24839 = CARTESIAN_POINT ( 'NONE',  ( -17.95536891708715999, -0.3560938001956550081, 4.240817377596695970 ) ) ;
#24840 = ORIENTED_EDGE ( 'NONE', *, *, #34617, .F. ) ;
#24841 = VECTOR ( 'NONE', #6231, 1000.000000000000227 ) ;
#24842 = EDGE_CURVE ( 'NONE', #55136, #26740, #30718, .T. ) ;
#24843 = ORIENTED_EDGE ( 'NONE', *, *, #33495, .T. ) ;
#24844 = CARTESIAN_POINT ( 'NONE',  ( -26.26580391614848864, 17.49370688441070953, -4.657437592157546824 ) ) ;
#24845 = ORIENTED_EDGE ( 'NONE', *, *, #11083, .T. ) ;
#24846 = ORIENTED_EDGE ( 'NONE', *, *, #6264, .T. ) ;
#24847 = EDGE_CURVE ( 'NONE', #2618, #280, #31195, .T. ) ;
#24848 = VECTOR ( 'NONE', #49934, 1000.000000000000114 ) ;
#24849 = AXIS2_PLACEMENT_3D ( 'NONE', #49255, #10669, #19428 ) ;
#24850 = CARTESIAN_POINT ( 'NONE',  ( -16.75946939063593177, 0.000000000000000000, 8.383301757569700641 ) ) ;
#24851 = CARTESIAN_POINT ( 'NONE',  ( -15.63164134753341372, -4.727446477803162850, 10.51233714212408543 ) ) ;
#24852 = DIRECTION ( 'NONE',  ( 0.007781995580012662783, 0.000000000000000000, -0.9999697198139514409 ) ) ;
#24853 = DIRECTION ( 'NONE',  ( -0.5364919789714478471, 0.6444004775717705469, -0.5449076811759709926 ) ) ;
#24854 = CARTESIAN_POINT ( 'NONE',  ( -13.92721955262090106, 0.000000000000000000, 2.696035920016314424 ) ) ;
#24855 = ORIENTED_EDGE ( 'NONE', *, *, #1417, .T. ) ;
#24856 = ORIENTED_EDGE ( 'NONE', *, *, #55021, .T. ) ;
#24857 = FACE_OUTER_BOUND ( 'NONE', #41915, .T. ) ;
#24858 = CARTESIAN_POINT ( 'NONE',  ( -6.086429055005921462, -7.947879803594625869, 5.582549316628845126 ) ) ;
#24859 = DIRECTION ( 'NONE',  ( 0.9999697198139515519, 0.000000000000000000, 0.007781995580013368816 ) ) ;
#24860 = CIRCLE ( 'NONE', #4027, 1.750000000000003331 ) ;
#24861 = FACE_OUTER_BOUND ( 'NONE', #592, .T. ) ;
#24862 = AXIS2_PLACEMENT_3D ( 'NONE', #25060, #55999, #17093 ) ;
#24863 = CARTESIAN_POINT ( 'NONE',  ( -22.04727804374295275, 19.65758491770980143, 4.422150965879553475 ) ) ;
#24864 = DIRECTION ( 'NONE',  ( -0.6427681459581293666, -0.7660444431189770143, -0.005002170337467561935 ) ) ;
#24865 = ORIENTED_EDGE ( 'NONE', *, *, #19761, .F. ) ;
#24866 = DIRECTION ( 'NONE',  ( -0.7660212471507179544, -0.6427876096865405842, -0.005961354470445141482 ) ) ;
#24867 = LINE ( 'NONE', #25171, #25848 ) ;
#24868 = VECTOR ( 'NONE', #5806, 1000.000000000000114 ) ;
#24869 = EDGE_LOOP ( 'NONE', ( #6046, #7510, #47309 ) ) ;
#24870 = DIRECTION ( 'NONE',  ( 0.9999697198139515519, 0.000000000000000000, 0.007781995580013368816 ) ) ;
#24871 = FACE_OUTER_BOUND ( 'NONE', #37740, .T. ) ;
#24872 = DIRECTION ( 'NONE',  ( -0.005002170337468016433, -0.7660444431189770143, 0.6427681459581293666 ) ) ;
#24873 = VECTOR ( 'NONE', #13044, 1000.000000000000114 ) ;
#24874 = DIRECTION ( 'NONE',  ( 0.9999697198139515519, 0.000000000000000000, 0.007781995580013368816 ) ) ;
#24875 = CARTESIAN_POINT ( 'NONE',  ( -17.73140113748535285, 0.000000000000000000, 13.85752530597602039 ) ) ;
#24876 = ORIENTED_EDGE ( 'NONE', *, *, #51818, .T. ) ;
#24877 = ORIENTED_EDGE ( 'NONE', *, *, #30823, .F. ) ;
#24878 = AXIS2_PLACEMENT_3D ( 'NONE', #541, #49066, #14708 ) ;
#24879 = LINE ( 'NONE', #33668, #11266 ) ;
#24880 = LINE ( 'NONE', #3311, #48531 ) ;
#24881 = CARTESIAN_POINT ( 'NONE',  ( -14.49394927539066025, -0.1191753592594189670, 2.960954539966670573 ) ) ;
#24882 = VECTOR ( 'NONE', #28915, 1000.000000000000227 ) ;
#24883 = ADVANCED_FACE ( 'NONE', ( #22182 ), #1137, .F. ) ;
#24884 = B_SPLINE_CURVE_WITH_KNOTS ( 'NONE', 3,
 ( #41515, #32694, #33541, #45755 ),
 .UNSPECIFIED., .F., .F.,
 ( 4, 4 ),
 ( 0.000000000000000000, 7.270906544745860773E-05 ),
 .UNSPECIFIED. ) ;
#24885 = CARTESIAN_POINT ( 'NONE',  ( 2.072287782118878319, 0.000000000000000000, -2.950529333540147015 ) ) ;
#24886 = CARTESIAN_POINT ( 'NONE',  ( -22.36894862246310822, -5.051250379848164052, 5.409019081522692396 ) ) ;
#24887 = EDGE_CURVE ( 'NONE', #35148, #23097, #22482, .T. ) ;
#24888 = CARTESIAN_POINT ( 'NONE',  ( -13.00639936336226476, 25.14902767225597913, -3.505746236942866911 ) ) ;
#24889 = EDGE_CURVE ( 'NONE', #9162, #28180, #39517, .T. ) ;
#24890 = LINE ( 'NONE', #37954, #10211 ) ;
#24891 = VECTOR ( 'NONE', #16155, 999.9999999999998863 ) ;
#24892 = DIRECTION ( 'NONE',  ( 0.5364919789714477361, 0.6444004775717706579, 0.5449076811759711036 ) ) ;
#24893 = VECTOR ( 'NONE', #48647, 1000.000000000000227 ) ;
#24894 = LINE ( 'NONE', #736, #639 ) ;
#24895 =( BOUNDED_CURVE ( )  B_SPLINE_CURVE ( 3, ( #495, #27172, #39105, #39946 ),
 .UNSPECIFIED., .F., .F. ) 
 B_SPLINE_CURVE_WITH_KNOTS ( ( 4, 4 ),
 ( 5.898329122556059900, 6.283185307179586232 ),
 .UNSPECIFIED. ) 
 CURVE ( )  GEOMETRIC_REPRESENTATION_ITEM ( )  RATIONAL_B_SPLINE_CURVE ( ( 1.000000000000000000, 0.9876951826469673179, 0.9876951826469673179, 1.000000000000000000 ) ) 
 REPRESENTATION_ITEM ( '' )  );
#24896 = CARTESIAN_POINT ( 'NONE',  ( -22.40478740399063895, 0.000000000000000000, 5.384712028983816623 ) ) ;
#24897 = ORIENTED_EDGE ( 'NONE', *, *, #30439, .F. ) ;
#24898 = DIRECTION ( 'NONE',  ( -0.6427681459581293666, -0.7660444431189770143, -0.005002170337467561935 ) ) ;
#24899 = ORIENTED_EDGE ( 'NONE', *, *, #12784, .T. ) ;
#24900 = AXIS2_PLACEMENT_3D ( 'NONE', #53924, #32899, #50216 ) ;
#24901 = VERTEX_POINT ( 'NONE', #35261 ) ;
#24902 = VERTEX_POINT ( 'NONE', #30965 ) ;
#24903 = EDGE_LOOP ( 'NONE', ( #38453, #9969, #24393, #28117 ) ) ;
#24904 = VECTOR ( 'NONE', #49437, 999.9999999999998863 ) ;
#24905 = ORIENTED_EDGE ( 'NONE', *, *, #37641, .F. ) ;
#24906 = CARTESIAN_POINT ( 'NONE',  ( -17.46532115785441519, 0.000000000000000000, 13.67492996699914265 ) ) ;
#24907 = LINE ( 'NONE', #24604, #36577 ) ;
#24908 = CARTESIAN_POINT ( 'NONE',  ( -7.159975159455704841, 6.987782224127484731, 5.999551081376306882 ) ) ;
#24909 = VECTOR ( 'NONE', #55111, 1000.000000000000114 ) ;
#24910 = ORIENTED_EDGE ( 'NONE', *, *, #20660, .F. ) ;
#24911 = DIRECTION ( 'NONE',  ( -0.1139275668495183386, 0.9934890585767658377, 4.694855797473113547E-16 ) ) ;
#24912 = EDGE_LOOP ( 'NONE', ( #24151, #2353, #32770, #56092 ) ) ;
#24913 = VECTOR ( 'NONE', #17955, 999.9999999999998863 ) ;
#24914 = CARTESIAN_POINT ( 'NONE',  ( -66.74449147233332269, -11.36157748060019301, 7.448312483692313357 ) ) ;
#24915 = VERTEX_POINT ( 'NONE', #26427 ) ;
#24916 = ADVANCED_FACE ( 'NONE', ( #48587 ), #44585, .F. ) ;
#24917 = VECTOR ( 'NONE', #12587, 1000.000000000000227 ) ;
#24918 = CARTESIAN_POINT ( 'NONE',  ( -66.55855263966657276, -8.722205571141092406, -0.3415480826687185001 ) ) ;
#24919 = EDGE_CURVE ( 'NONE', #14383, #40367, #27014, .T. ) ;
#24920 = VECTOR ( 'NONE', #29876, 999.9999999999998863 ) ;
#24921 = FACE_OUTER_BOUND ( 'NONE', #41096, .T. ) ;
#24922 = CARTESIAN_POINT ( 'NONE',  ( -19.45503627000849889, -1.000000000000000000, 7.556996783084074742 ) ) ;
#24923 = ORIENTED_EDGE ( 'NONE', *, *, #2728, .T. ) ;
#24924 = FACE_OUTER_BOUND ( 'NONE', #28308, .T. ) ;
#24925 = ORIENTED_EDGE ( 'NONE', *, *, #53471, .T. ) ;
#24926 = AXIS2_PLACEMENT_3D ( 'NONE', #53378, #26984, #10201 ) ;
#24927 = FACE_OUTER_BOUND ( 'NONE', #6462, .T. ) ;
#24928 = EDGE_CURVE ( 'NONE', #17689, #25841, #4858, .T. ) ;
#24929 = CARTESIAN_POINT ( 'NONE',  ( -13.67119876025844860, 0.000000000000000000, 3.806024542441613701 ) ) ;
#24930 = VECTOR ( 'NONE', #19147, 1000.000000000000000 ) ;
#24931 = DIRECTION ( 'NONE',  ( -0.5449076811759708816, 0.6444004775717707689, 0.5364919789714475140 ) ) ;
#24932 = VECTOR ( 'NONE', #52096, 1000.000000000000114 ) ;
#24933 = LINE ( 'NONE', #51030, #32224 ) ;
#24934 = FACE_BOUND ( 'NONE', #27758, .T. ) ;
#24935 = CARTESIAN_POINT ( 'NONE',  ( -69.34476620134752523, -0.4004433531566040649, -7.487678583014045763 ) ) ;
#24936 = LINE ( 'NONE', #15843, #20284 ) ;
#24937 = DIRECTION ( 'NONE',  ( -0.6246952433987893460, -0.7422098413412802076, 0.2426528472758542054 ) ) ;
#24938 = ORIENTED_EDGE ( 'NONE', *, *, #365, .F. ) ;
#24939 = LINE ( 'NONE', #3366, #54657 ) ;
#24940 = VERTEX_POINT ( 'NONE', #21891 ) ;
#24941 = LINE ( 'NONE', #42263, #23829 ) ;
#24942 = CARTESIAN_POINT ( 'NONE',  ( -11.36984871579436174, -0.8417996532631562001, 1.270898663839582943 ) ) ;
#24943 = FACE_OUTER_BOUND ( 'NONE', #17099, .T. ) ;
#24944 = CARTESIAN_POINT ( 'NONE',  ( -11.78272344325496945, 1.095915999411504194, 1.223776201692182930 ) ) ;
#24945 = CARTESIAN_POINT ( 'NONE',  ( -9.977096013572023026, 0.000000000000000000, 6.789429462647804669 ) ) ;
#24946 = VECTOR ( 'NONE', #40177, 1000.000000000000114 ) ;
#24947 = LINE ( 'NONE', #50515, #23902 ) ;
#24948 = VECTOR ( 'NONE', #34839, 999.9999999999998863 ) ;
#24949 = ORIENTED_EDGE ( 'NONE', *, *, #2442, .F. ) ;
#24950 = DIRECTION ( 'NONE',  ( -0.7660212471507179544, -0.6427876096865405842, -0.005961354470445141482 ) ) ;
#24951 = DIRECTION ( 'NONE',  ( -8.881784197001252323E-16, 0.000000000000000000, -1.000000000000000000 ) ) ;
#24952 = CARTESIAN_POINT ( 'NONE',  ( -11.33939211553717286, 0.000000000000000000, 2.716174991508366610 ) ) ;
#24953 = ADVANCED_FACE ( 'NONE', ( #4578 ), #39791, .F. ) ;
#24954 = DIRECTION ( 'NONE',  ( 0.005002170337468016433, -0.7660444431189770143, -0.6427681459581293666 ) ) ;
#24955 = VECTOR ( 'NONE', #14470, 1000.000000000000114 ) ;
#24956 = DIRECTION ( 'NONE',  ( -0.5449076811759708816, 0.6444004775717707689, 0.5364919789714475140 ) ) ;
#24957 = VECTOR ( 'NONE', #48770, 999.9999999999998863 ) ;
#24958 = CARTESIAN_POINT ( 'NONE',  ( -26.13337879274045505, 0.000000000000000000, 6.833023547870798353 ) ) ;
#24959 = DIRECTION ( 'NONE',  ( 0.9999697198139515519, 0.000000000000000000, 0.007781995580013368816 ) ) ;
#24960 = EDGE_CURVE ( 'NONE', #873, #44414, #44324, .T. ) ;
#24961 = ORIENTED_EDGE ( 'NONE', *, *, #39238, .F. ) ;
#24962 = LINE ( 'NONE', #45684, #399 ) ;
#24963 = AXIS2_PLACEMENT_3D ( 'NONE', #9195, #44132, #5242 ) ;
#24964 = CARTESIAN_POINT ( 'NONE',  ( -18.36790206993104846, -4.727446477803164626, 3.865207764181160854 ) ) ;
#24965 = VECTOR ( 'NONE', #20364, 1000.000000000000227 ) ;
#24966 = ORIENTED_EDGE ( 'NONE', *, *, #23973, .F. ) ;
#24967 = VECTOR ( 'NONE', #402, 1000.000000000000227 ) ;
#24968 = EDGE_LOOP ( 'NONE', ( #43230, #30759, #5012, #25815 ) ) ;
#24969 = LINE ( 'NONE', #29801, #12887 ) ;
#24970 = AXIS2_PLACEMENT_3D ( 'NONE', #16701, #38269, #46810 ) ;
#24971 = ORIENTED_EDGE ( 'NONE', *, *, #20747, .T. ) ;
#24972 = VECTOR ( 'NONE', #17583, 1000.000000000000000 ) ;
#24973 = ORIENTED_EDGE ( 'NONE', *, *, #28373, .F. ) ;
#24974 = CARTESIAN_POINT ( 'NONE',  ( -17.17779978478095515, -1.651309408375659871, 3.501076498445555352 ) ) ;
#24975 = ADVANCED_FACE ( 'NONE', ( #16 ), #17345, .F. ) ;
#24976 = AXIS2_PLACEMENT_3D ( 'NONE', #1701, #32642, #49119 ) ;
#24977 = EDGE_LOOP ( 'NONE', ( #14915, #6669, #52934 ) ) ;
#24978 = VECTOR ( 'NONE', #41285, 1000.000000000000227 ) ;
#24979 = EDGE_LOOP ( 'NONE', ( #28851, #53960, #32913, #1157 ) ) ;
#24980 = EDGE_LOOP ( 'NONE', ( #15153, #15267, #36342, #24169, #29397 ) ) ;
#24981 = CARTESIAN_POINT ( 'NONE',  ( -14.16170213864708138, 0.000000000000000000, 7.126195959993483875 ) ) ;
#24982 = PLANE ( 'NONE',  #54974 ) ;
#24983 = PLANE ( 'NONE',  #33070 ) ;
#24984 = EDGE_LOOP ( 'NONE', ( #31973, #11510, #54569, #53229, #16281 ) ) ;
#24985 = ORIENTED_EDGE ( 'NONE', *, *, #26082, .T. ) ;
#24986 = AXIS2_PLACEMENT_3D ( 'NONE', #54840, #50591, #50296 ) ;
#24987 = CARTESIAN_POINT ( 'NONE',  ( -25.20123094555300369, 0.000000000000000000, 6.470945668149052032 ) ) ;
#24988 = LINE ( 'NONE', #42313, #53581 ) ;
#24989 = VECTOR ( 'NONE', #18770, 1000.000000000000114 ) ;
#24990 = ORIENTED_EDGE ( 'NONE', *, *, #50480, .T. ) ;
#24991 = FACE_OUTER_BOUND ( 'NONE', #53687, .T. ) ;
#24992 = ORIENTED_EDGE ( 'NONE', *, *, #5881, .F. ) ;
#24993 = VECTOR ( 'NONE', #44481, 1000.000000000000227 ) ;
#24994 = DIRECTION ( 'NONE',  ( -0.5449076811759708816, 0.6444004775717707689, 0.5364919789714475140 ) ) ;
#24995 = LINE ( 'NONE', #3414, #4835 ) ;
#24996 = EDGE_LOOP ( 'NONE', ( #45535, #18075, #48913, #47451 ) ) ;
#24997 = DIRECTION ( 'NONE',  ( -0.005961354470445682716, -0.6427876096865404731, 0.7660212471507180654 ) ) ;
#24998 = EDGE_CURVE ( 'NONE', #13188, #6357, #13107, .T. ) ;
#24999 = VECTOR ( 'NONE', #16765, 1000.000000000000227 ) ;
#25000 = CARTESIAN_POINT ( 'NONE',  ( -23.33693525117809386, 0.000000000000000000, 5.746789908705562944 ) ) ;
#25001 = AXIS2_PLACEMENT_3D ( 'NONE', #50621, #38107, #2624 ) ;
#25002 = AXIS2_PLACEMENT_3D ( 'NONE', #20215, #54564, #49781 ) ;
#25003 = ORIENTED_EDGE ( 'NONE', *, *, #31474, .T. ) ;
#25004 = CARTESIAN_POINT ( 'NONE',  ( -14.94760462649100496, 0.000000000000000000, 2.488088991209854051 ) ) ;
#25005 = LINE ( 'NONE', #43438, #51967 ) ;
#25006 = CARTESIAN_POINT ( 'NONE',  ( -18.91281239749552867, -5.375054281893166142, 4.056207361090260477 ) ) ;
#25007 = FACE_OUTER_BOUND ( 'NONE', #44463, .T. ) ;
#25008 = ORIENTED_EDGE ( 'NONE', *, *, #34926, .F. ) ;
#25009 = AXIS2_PLACEMENT_3D ( 'NONE', #10069, #9521, #26274 ) ;
#25010 = EDGE_CURVE ( 'NONE', #32117, #22899, #17642, .T. ) ;
#25011 = AXIS2_PLACEMENT_3D ( 'NONE', #1658, #30911, #18983 ) ;
#25012 = DIRECTION ( 'NONE',  ( 0.007781995580012663651, -3.146120232559066537E-19, -0.9999697198139514409 ) ) ;
#25013 = LINE ( 'NONE', #42595, #19639 ) ;
#25014 = FACE_OUTER_BOUND ( 'NONE', #10992, .T. ) ;
#25015 = AXIS2_PLACEMENT_3D ( 'NONE', #14433, #39718, #36031 ) ;
#25016 = DIRECTION ( 'NONE',  ( 0.007781995580012663651, -3.146120232559066537E-19, -0.9999697198139514409 ) ) ;
#25017 = EDGE_CURVE ( 'NONE', #22830, #36235, #18784, .T. ) ;
#25018 = CARTESIAN_POINT ( 'NONE',  ( -23.33849165029409889, 0.000000000000000000, 5.946783852668351855 ) ) ;
#25020 = EDGE_CURVE ( 'NONE', #22456, #23017, #41840, .T. ) ;
#25019 = DIRECTION ( 'NONE',  ( 0.9999697198139515519, 0.000000000000000000, 0.007781995580013368816 ) ) ;
#25021 = VECTOR ( 'NONE', #38512, 1000.000000000000227 ) ;
#25022 = AXIS2_PLACEMENT_3D ( 'NONE', #31160, #8773, #25789 ) ;
#25023 = DIRECTION ( 'NONE',  ( 0.000000000000000000, 0.000000000000000000, 1.000000000000000000 ) ) ;
#25024 = ORIENTED_EDGE ( 'NONE', *, *, #2240, .F. ) ;
#25025 = DIRECTION ( 'NONE',  ( 0.005002170337468016433, -0.7660444431189770143, -0.6427681459581293666 ) ) ;
#25026 = CARTESIAN_POINT ( 'NONE',  ( 2.072287782118878319, 0.000000000000000000, -2.950529333540147015 ) ) ;
#25027 = ORIENTED_EDGE ( 'NONE', *, *, #36360, .T. ) ;
#25028 = DIRECTION ( 'NONE',  ( 0.005961354470445682716, -0.6427876096865404731, -0.7660212471507180654 ) ) ;
#25029 = ADVANCED_FACE ( 'NONE', ( #45174 ), #10238, .F. ) ;
#25030 = CARTESIAN_POINT ( 'NONE',  ( -12.02422819173196089, 1.905425754524007198, 4.679067971174708518 ) ) ;
#25031 = ADVANCED_FACE ( 'NONE', ( #2269 ), #40892, .F. ) ;
#25032 = DIRECTION ( 'NONE',  ( 0.005961354470445682716, -0.6427876096865404731, -0.7660212471507180654 ) ) ;
#25033 = PLANE ( 'NONE',  #51410 ) ;
#25034 = EDGE_CURVE ( 'NONE', #40075, #21894, #10543, .T. ) ;
#25035 = DIRECTION ( 'NONE',  ( -0.7660212471507179544, -0.6427876096865405842, -0.005961354470445141482 ) ) ;
#25036 = AXIS2_PLACEMENT_3D ( 'NONE', #43352, #14084, #31413 ) ;
#25037 = EDGE_LOOP ( 'NONE', ( #48946, #12856, #17232, #17565 ) ) ;
#25038 = EDGE_LOOP ( 'NONE', ( #4163, #25927, #41843, #35258 ) ) ;
#25039 = LINE ( 'NONE', #37232, #54943 ) ;
#25040 = CARTESIAN_POINT ( 'NONE',  ( -13.66427238189300830, -2.460819163488160655, 2.110475535834075433 ) ) ;
#25041 = VECTOR ( 'NONE', #9511, 1000.000000000000227 ) ;
#25042 = DIRECTION ( 'NONE',  ( 0.9999697198139515519, 0.000000000000000000, 0.007781995580013368816 ) ) ;
#25043 = EDGE_CURVE ( 'NONE', #23769, #16052, #53667, .T. ) ;
#25044 = VERTEX_POINT ( 'NONE', #54238 ) ;
#25045 = FACE_OUTER_BOUND ( 'NONE', #2923, .T. ) ;
#25046 = VECTOR ( 'NONE', #28081, 1000.000000000000227 ) ;
#25047 = EDGE_LOOP ( 'NONE', ( #27895, #2678, #27302, #7364, #47310 ) ) ;
#25048 = DIRECTION ( 'NONE',  ( 0.007781995580012663651, -3.146120232559066537E-19, -0.9999697198139514409 ) ) ;
#25049 = ADVANCED_FACE ( 'NONE', ( #1970 ), #31818, .F. ) ;
#25050 = AXIS2_PLACEMENT_3D ( 'NONE', #49384, #23280, #31787 ) ;
#25051 = AXIS2_PLACEMENT_3D ( 'NONE', #51179, #51731, #55428 ) ;
#25052 = ORIENTED_EDGE ( 'NONE', *, *, #27459, .T. ) ;
#25053 = ORIENTED_EDGE ( 'NONE', *, *, #17379, .F. ) ;
#25054 = ORIENTED_EDGE ( 'NONE', *, *, #32580, .F. ) ;
#25055 = PLANE ( 'NONE',  #52894 ) ;
#25056 = FACE_OUTER_BOUND ( 'NONE', #19721, .T. ) ;
#25057 = LINE ( 'NONE', #55697, #28478 ) ;
#25058 = AXIS2_PLACEMENT_3D ( 'NONE', #7834, #2437, #42461 ) ;
#25059 = VECTOR ( 'NONE', #39097, 1000.000000000000000 ) ;
#25060 = CARTESIAN_POINT ( 'NONE',  ( -24.96676581047183063, 18.24370688441070953, -4.657437592157546824 ) ) ;
#25061 = ORIENTED_EDGE ( 'NONE', *, *, #11613, .F. ) ;
#25062 = AXIS2_PLACEMENT_3D ( 'NONE', #17938, #12815, #18471 ) ;
#25063 = ORIENTED_EDGE ( 'NONE', *, *, #50599, .F. ) ;
#25064 = VECTOR ( 'NONE', #47808, 1000.000000000000227 ) ;
#25065 = EDGE_LOOP ( 'NONE', ( #37265, #54946, #14169, #26731 ) ) ;
#25066 = DIRECTION ( 'NONE',  ( 0.6427681459581294776, -0.7660444431189769032, 0.005002170337467562802 ) ) ;
#25067 = DIRECTION ( 'NONE',  ( -0.005002170337468016433, -0.7660444431189770143, 0.6427681459581293666 ) ) ;
#25068 = ORIENTED_EDGE ( 'NONE', *, *, #52470, .F. ) ;
#25069 = FACE_OUTER_BOUND ( 'NONE', #26858, .T. ) ;
#25070 = ORIENTED_EDGE ( 'NONE', *, *, #7853, .F. ) ;
#25071 = DIRECTION ( 'NONE',  ( 0.6427681459581294776, -0.7660444431189769032, 0.005002170337467562802 ) ) ;
#25072 = CARTESIAN_POINT ( 'NONE',  ( -1.300095020133916979, 4.816411402586080470, 3.723374632896542025 ) ) ;
#25073 = ORIENTED_EDGE ( 'NONE', *, *, #48608, .T. ) ;
#25074 = DIRECTION ( 'NONE',  ( 0.000000000000000000, -0.000000000000000000, -1.000000000000000000 ) ) ;
#25075 = EDGE_CURVE ( 'NONE', #30608, #20261, #41470, .T. ) ;
#25076 = ORIENTED_EDGE ( 'NONE', *, *, #44256, .F. ) ;
#25077 = VECTOR ( 'NONE', #5840, 1000.000000000000227 ) ;
#25078 = DIRECTION ( 'NONE',  ( -0.5449076811759708816, 0.6444004775717707689, 0.5364919789714475140 ) ) ;
#25079 = CARTESIAN_POINT ( 'NONE',  ( -14.44189180272386430, 2.553033558614007603, 6.681005357687642032 ) ) ;
#25080 = ORIENTED_EDGE ( 'NONE', *, *, #42982, .F. ) ;
#25081 = DIRECTION ( 'NONE',  ( -0.1139275668495183524, 0.9934890585767659488, 4.694855797473114533E-16 ) ) ;
#25082 = LINE ( 'NONE', #34168, #53822 ) ;
#25083 = LINE ( 'NONE', #560, #34143 ) ;
#25084 = DIRECTION ( 'NONE',  ( 0.9335804264972044075, -0.3583679495452936070, 8.673617379884025611E-16 ) ) ;
#25085 = VECTOR ( 'NONE', #52792, 1000.000000000000000 ) ;
#25086 = ORIENTED_EDGE ( 'NONE', *, *, #56086, .F. ) ;
#25087 = ADVANCED_FACE ( 'NONE', ( #15593 ), #27557, .F. ) ;
#25088 = ADVANCED_FACE ( 'NONE', ( #49708 ), #23575, .F. ) ;
#25089 = EDGE_LOOP ( 'NONE', ( #24217, #16231, #2798, #53132 ) ) ;
#25090 = CARTESIAN_POINT ( 'NONE',  ( -56.75000000000001421, 4.436683557093994423, 2.449489742783185875 ) ) ;
#25091 = VECTOR ( 'NONE', #25510, 1000.000000000000227 ) ;
#25092 = LINE ( 'NONE', #46644, #20316 ) ;
#25093 = DIRECTION ( 'NONE',  ( -0.6246952433987894571, 0.7422098413412802076, 0.2426528472758539834 ) ) ;
#25094 = CARTESIAN_POINT ( 'NONE',  ( -27.99767448711536133, 0.000000000000000000, 7.557179307314289218 ) ) ;
#25096 = EDGE_CURVE ( 'NONE', #17177, #940, #36645, .T. ) ;
#25095 = DIRECTION ( 'NONE',  ( -0.7660212471507179544, -0.6427876096865405842, -0.005961354470445141482 ) ) ;
#25097 = VECTOR ( 'NONE', #7923, 999.9999999999998863 ) ;
#25098 = PLANE ( 'NONE',  #50323 ) ;
#25099 = ORIENTED_EDGE ( 'NONE', *, *, #1559, .F. ) ;
#25100 = DIRECTION ( 'NONE',  ( 0.007781995580012663651, -3.146120232559066537E-19, -0.9999697198139514409 ) ) ;
#25101 = DIRECTION ( 'NONE',  ( 0.7660212471507180654, -0.6427876096865404731, 0.005961354470445141482 ) ) ;
#25102 = VERTEX_POINT ( 'NONE', #44881 ) ;
#25103 = CARTESIAN_POINT ( 'NONE',  ( -19.17512305244570214, 4.819660872929010687, 12.23947469159592494 ) ) ;
#25104 = ORIENTED_EDGE ( 'NONE', *, *, #20659, .T. ) ;
#25105 = CARTESIAN_POINT ( 'NONE',  ( -27.06708303904391144, 0.000000000000000000, 7.395095371555332697 ) ) ;
#25106 = CARTESIAN_POINT ( 'NONE',  ( -19.60912206198628027, -0.1191753592594197858, 4.398475361799976113 ) ) ;
#25107 = AXIS2_PLACEMENT_3D ( 'NONE', #50040, #11152, #11455 ) ;
#25108 = EDGE_CURVE ( 'NONE', #9654, #17188, #28688, .T. ) ;
#25109 = PLANE ( 'NONE',  #41353 ) ;
#25110 = CARTESIAN_POINT ( 'NONE',  ( 2.072287782118878319, 0.000000000000000000, -2.950529333540147015 ) ) ;
#25111 = VECTOR ( 'NONE', #16659, 1000.000000000000227 ) ;
#25112 = ADVANCED_FACE ( 'NONE', ( #36104 ), #23844, .F. ) ;
#25113 = CARTESIAN_POINT ( 'NONE',  ( -66.97721288434047437, 1.999999999999990452, 6.550948917179798769 ) ) ;
#25114 = ORIENTED_EDGE ( 'NONE', *, *, #106, .T. ) ;
#25115 = VECTOR ( 'NONE', #28666, 999.9999999999998863 ) ;
#25116 = VERTEX_POINT ( 'NONE', #53958 ) ;
#25117 = DIRECTION ( 'NONE',  ( -0.5364919789714478471, 0.6444004775717705469, -0.5449076811759709926 ) ) ;
#25118 = LINE ( 'NONE', #38143, #53961 ) ;
#25119 = DIRECTION ( 'NONE',  ( 0.007781995580012662783, 0.000000000000000000, -0.9999697198139514409 ) ) ;
#25120 = LINE ( 'NONE', #24815, #33163 ) ;
#25121 = EDGE_CURVE ( 'NONE', #42656, #11634, #11354, .T. ) ;
#25122 = CARTESIAN_POINT ( 'NONE',  ( -26.13337879274045505, 0.000000000000000000, 6.833023547870798353 ) ) ;
#25123 = CARTESIAN_POINT ( 'NONE',  ( -15.82600388905919608, 0.000000000000000000, 7.851908118552977989 ) ) ;
#25124 = EDGE_LOOP ( 'NONE', ( #12357, #46022, #18257, #26364 ) ) ;
#25125 = CARTESIAN_POINT ( 'NONE',  ( -21.49419195319602238, -4.565544526780663581, 5.084730443979996295 ) ) ;
#25126 = VECTOR ( 'NONE', #40010, 999.9999999999998863 ) ;
#25127 = CARTESIAN_POINT ( 'NONE',  ( -8.024318355659660895, -0.1191753592594181205, 6.335291332000426046 ) ) ;
#25128 = CARTESIAN_POINT ( 'NONE',  ( -23.33849165029409889, 0.000000000000000000, 5.946783852668351855 ) ) ;
#25129 = ORIENTED_EDGE ( 'NONE', *, *, #23603, .F. ) ;
#25130 = LINE ( 'NONE', #15455, #1159 ) ;
#25131 = CARTESIAN_POINT ( 'NONE',  ( 2.072287782118878319, 0.000000000000000000, -2.950529333540147015 ) ) ;
#25132 = LINE ( 'NONE', #4386, #6684 ) ;
#25133 = ORIENTED_EDGE ( 'NONE', *, *, #51842, .F. ) ;
#25134 = DIRECTION ( 'NONE',  ( -0.005002170337468016433, -0.7660444431189770143, 0.6427681459581293666 ) ) ;
#25135 = VECTOR ( 'NONE', #18696, 999.9999999999998863 ) ;
#25136 = ORIENTED_EDGE ( 'NONE', *, *, #41198, .T. ) ;
#25137 = EDGE_LOOP ( 'NONE', ( #48373, #16173, #21505, #45108 ) ) ;
#25138 = VECTOR ( 'NONE', #1810, 1000.000000000000000 ) ;
#25139 = VERTEX_POINT ( 'NONE', #40342 ) ;
#25140 = VERTEX_POINT ( 'NONE', #1442 ) ;
#25141 = DIRECTION ( 'NONE',  ( 0.9999697198139515519, 0.000000000000000000, 0.007781995580013368816 ) ) ;
#25143 = EDGE_CURVE ( 'NONE', #46034, #6528, #23319, .T. ) ;
#25142 = VERTEX_POINT ( 'NONE', #15072 ) ;
#25144 = DIRECTION ( 'NONE',  ( -0.6246952433987894571, 0.7422098413412802076, 0.2426528472758539834 ) ) ;
#25145 = AXIS2_PLACEMENT_3D ( 'NONE', #11594, #2756, #20080 ) ;
#25146 = VERTEX_POINT ( 'NONE', #45419 ) ;
#25147 = CARTESIAN_POINT ( 'NONE',  ( -21.47419595591918906, 0.000000000000000000, 5.222628093224860102 ) ) ;
#25148 = ORIENTED_EDGE ( 'NONE', *, *, #40097, .F. ) ;
#25149 = EDGE_CURVE ( 'NONE', #15196, #31624, #6534, .T. ) ;
#25150 = ORIENTED_EDGE ( 'NONE', *, *, #18306, .T. ) ;
#25151 = DIRECTION ( 'NONE',  ( 0.007781995580012662783, 0.000000000000000000, -0.9999697198139514409 ) ) ;
#25152 = CARTESIAN_POINT ( 'NONE',  ( -16.05094756644385967, 4.981562823951511731, 11.29164751933717525 ) ) ;
#25153 = EDGE_CURVE ( 'NONE', #38932, #26788, #54784, .T. ) ;
#25154 = DIRECTION ( 'NONE',  ( -0.3583679495452941066, -0.9335804264972041855, 0.000000000000000000 ) ) ;
#25155 = CARTESIAN_POINT ( 'NONE',  ( -26.13493519185646008, 0.000000000000000000, 7.033017491833586377 ) ) ;
#25156 = CARTESIAN_POINT ( 'NONE',  ( -27.06708303904391144, 0.000000000000000000, 7.395095371555332697 ) ) ;
#25157 = ORIENTED_EDGE ( 'NONE', *, *, #1345, .F. ) ;
#25158 = EDGE_CURVE ( 'NONE', #23927, #38022, #37464, .T. ) ;
#25159 = EDGE_CURVE ( 'NONE', #8086, #4449, #34347, .T. ) ;
#25160 = ADVANCED_FACE ( 'NONE', ( #38036 ), #51079, .F. ) ;
#25161 = EDGE_LOOP ( 'NONE', ( #19456, #10529, #47992, #7379 ) ) ;
#25162 = CARTESIAN_POINT ( 'NONE',  ( -23.33693525117809386, 0.000000000000000000, 5.746789908705562944 ) ) ;
#25163 = CARTESIAN_POINT ( 'NONE',  ( -19.16905877885434606, -0.1191753592594168992, 6.617892454864216845 ) ) ;
#25164 = EDGE_CURVE ( 'NONE', #49938, #37899, #46536, .T. ) ;
#25165 = CARTESIAN_POINT ( 'NONE',  ( -15.88130887279446490, 0.000000000000000000, 3.050160814894388839 ) ) ;
#25166 = LINE ( 'NONE', #7261, #40324 ) ;
#25167 = CARTESIAN_POINT ( 'NONE',  ( -19.45503627000849889, -1.000000000000000000, 7.556996783084074742 ) ) ;
#25168 = FACE_OUTER_BOUND ( 'NONE', #25980, .T. ) ;
#25169 = ORIENTED_EDGE ( 'NONE', *, *, #24608, .T. ) ;
#25170 = CARTESIAN_POINT ( 'NONE',  ( -16.81345671998191449, 0.000000000000000000, 3.412238694616132495 ) ) ;
#25171 = CARTESIAN_POINT ( 'NONE',  ( -14.94916102560700821, 0.000000000000000000, 2.688082935172642962 ) ) ;
#25172 = ORIENTED_EDGE ( 'NONE', *, *, #26390, .T. ) ;
#25173 = CARTESIAN_POINT ( 'NONE',  ( 2.072287782118878319, 0.000000000000000000, -2.950529333540147015 ) ) ;
#25174 = LINE ( 'NONE', #50710, #8774 ) ;
#25175 = CARTESIAN_POINT ( 'NONE',  ( -11.60690912192075075, 0.000000000000000000, 3.083425182114127416 ) ) ;
#25176 = EDGE_CURVE ( 'NONE', #6270, #48144, #50802, .T. ) ;
#25177 = DIRECTION ( 'NONE',  ( -0.005961354470445682716, -0.6427876096865404731, 0.7660212471507180654 ) ) ;
#25178 = DIRECTION ( 'NONE',  ( -0.5449076811759708816, 0.6444004775717707689, 0.5364919789714475140 ) ) ;
#25179 = EDGE_CURVE ( 'NONE', #22744, #48082, #29221, .T. ) ;
#25180 = VECTOR ( 'NONE', #8707, 1000.000000000000114 ) ;
#25181 = VERTEX_POINT ( 'NONE', #16437 ) ;
#25182 = ORIENTED_EDGE ( 'NONE', *, *, #7927, .F. ) ;
#25183 = EDGE_CURVE ( 'NONE', #20216, #10313, #7112, .T. ) ;
#25184 = DIRECTION ( 'NONE',  ( 0.005961354470445682716, -0.6427876096865404731, -0.7660212471507180654 ) ) ;
#25185 = LINE ( 'NONE', #29982, #8665 ) ;
#25186 = DIRECTION ( 'NONE',  ( 0.000000000000000000, -1.000000000000000000, 0.000000000000000000 ) ) ;
#25187 = ADVANCED_FACE ( 'NONE', ( #7655 ), #20720, .F. ) ;
#25188 = VECTOR ( 'NONE', #113, 1000.000000000000227 ) ;
#25189 = LINE ( 'NONE', #7558, #6521 ) ;
#25190 = FACE_OUTER_BOUND ( 'NONE', #22588, .T. ) ;
#25191 = DIRECTION ( 'NONE',  ( -0.5364919789714478471, 0.6444004775717705469, -0.5449076811759709926 ) ) ;
#25192 = PLANE ( 'NONE',  #41923 ) ;
#25193 = EDGE_CURVE ( 'NONE', #13033, #25808, #55931, .T. ) ;
#25194 = DIRECTION ( 'NONE',  ( 0.007781995580012663651, -3.146120232559066537E-19, -0.9999697198139514409 ) ) ;
#25195 = CARTESIAN_POINT ( 'NONE',  ( -68.50231803695028532, -8.543494007632164156, -5.847034362371243965 ) ) ;
#25196 = CARTESIAN_POINT ( 'NONE',  ( -19.45503627000849889, -1.000000000000000000, 7.556996783084074742 ) ) ;
#25197 = ORIENTED_EDGE ( 'NONE', *, *, #52228, .T. ) ;
#25198 = DIRECTION ( 'NONE',  ( 0.007781995580012663651, 0.000000000000000000, -0.9999697198139515519 ) ) ;
#25199 = VERTEX_POINT ( 'NONE', #15893 ) ;
#25200 = VERTEX_POINT ( 'NONE', #20433 ) ;
#25201 = VERTEX_POINT ( 'NONE', #46847 ) ;
#25202 = ORIENTED_EDGE ( 'NONE', *, *, #25731, .F. ) ;
#25203 = ORIENTED_EDGE ( 'NONE', *, *, #14271, .T. ) ;
#25204 = VERTEX_POINT ( 'NONE', #25524 ) ;
#25205 = FACE_OUTER_BOUND ( 'NONE', #31099, .T. ) ;
#25206 = CARTESIAN_POINT ( 'NONE',  ( -15.84391369215092737, -5.051250379848164940, 2.874473923470473480 ) ) ;
#25207 = DIRECTION ( 'NONE',  ( -0.005002170337468016433, -0.7660444431189770143, 0.6427681459581293666 ) ) ;
#25208 = EDGE_LOOP ( 'NONE', ( #42520, #48147, #36668, #48921 ) ) ;
#25209 = PLANE ( 'NONE',  #46710 ) ;
#25210 = ORIENTED_EDGE ( 'NONE', *, *, #10925, .F. ) ;
#25211 = FACE_OUTER_BOUND ( 'NONE', #39153, .T. ) ;
#25212 = ORIENTED_EDGE ( 'NONE', *, *, #18813, .F. ) ;
#25213 = CARTESIAN_POINT ( 'NONE',  ( -66.84355256359847886, -8.754982504685631994, 2.715629364116394218 ) ) ;
#25214 = CARTESIAN_POINT ( 'NONE',  ( -14.42766274591465425, 0.000000000000000000, 7.293452206636453106 ) ) ;
#25215 = DIRECTION ( 'NONE',  ( -0.6427681459581293666, -0.7660444431189770143, -0.005002170337467561935 ) ) ;
#25216 = ORIENTED_EDGE ( 'NONE', *, *, #8320, .T. ) ;
#25217 = CARTESIAN_POINT ( 'NONE',  ( 2.072287782118878319, 0.000000000000000000, -2.950529333540147015 ) ) ;
#25218 = EDGE_LOOP ( 'NONE', ( #17494, #2443, #24356, #33839 ) ) ;
#25219 = ADVANCED_FACE ( 'NONE', ( #33498 ), #24983, .F. ) ;
#25220 = ADVANCED_FACE ( 'NONE', ( #51391 ), #17030, .F. ) ;
#25221 = AXIS2_PLACEMENT_3D ( 'NONE', #10580, #1474, #46031 ) ;
#25222 = CARTESIAN_POINT ( 'NONE',  ( -7.851256608156574224, 5.553015032381929394, -0.1686788792590568631 ) ) ;
#25223 = DIRECTION ( 'NONE',  ( -0.005002170337468016433, -0.7660444431189770143, 0.6427681459581293666 ) ) ;
#25224 = EDGE_CURVE ( 'NONE', #43677, #45113, #47111, .T. ) ;
#25225 = DIRECTION ( 'NONE',  ( 0.7660212471507180654, -0.6427876096865404731, 0.005961354470445141482 ) ) ;
#25226 = DIRECTION ( 'NONE',  ( 0.5449076811759707706, 0.6444004775717708799, -0.5364919789714476250 ) ) ;
#25227 = DIRECTION ( 'NONE',  ( 0.007781995580012663651, -3.146120232559066537E-19, -0.9999697198139514409 ) ) ;
#25228 = CARTESIAN_POINT ( 'NONE',  ( -19.12962290826653700, 0.000000000000000000, 14.40064212555863854 ) ) ;
#25229 = DIRECTION ( 'NONE',  ( -0.9999697198139514409, -0.000000000000000000, -0.007781995580013368816 ) ) ;
#25230 = CARTESIAN_POINT ( 'NONE',  ( -14.02149608406334380, -0.1166911823299071477, 2.228051675397754394 ) ) ;
#25231 = ORIENTED_EDGE ( 'NONE', *, *, #25780, .F. ) ;
#25232 = CARTESIAN_POINT ( 'NONE',  ( -56.75000000000001421, 6.148917331397711017, -2.449489742783171664 ) ) ;
#25233 = ORIENTED_EDGE ( 'NONE', *, *, #6917, .T. ) ;
#25234 = CARTESIAN_POINT ( 'NONE',  ( 2.072287782118878319, 0.000000000000000000, -2.950529333540147015 ) ) ;
#25235 = CARTESIAN_POINT ( 'NONE',  ( -10.21587248490277844, 0.000000000000000000, 3.463582620675918378 ) ) ;
#25236 = CARTESIAN_POINT ( 'NONE',  ( -19.74467861466184715, -3.594132820645662196, 4.436153168894599652 ) ) ;
#25237 = DIRECTION ( 'NONE',  ( -0.7660212471507179544, -0.6427876096865405842, -0.005961354470445141482 ) ) ;
#25238 = DIRECTION ( 'NONE',  ( 0.5364919789714477361, 0.6444004775717706579, 0.5449076811759711036 ) ) ;
#25239 = LINE ( 'NONE', #24377, #55643 ) ;
#25240 = EDGE_LOOP ( 'NONE', ( #28965, #821, #47392, #43273 ) ) ;
#25241 = CARTESIAN_POINT ( 'NONE',  ( -17.26532721389163072, 0.000000000000000000, 13.67648636611514590 ) ) ;
#25242 = DIRECTION ( 'NONE',  ( -0.005961354470445682716, -0.6427876096865404731, 0.7660212471507180654 ) ) ;
#25243 = CARTESIAN_POINT ( 'NONE',  ( -22.40634380310664397, 0.000000000000000000, 5.584705972946605534 ) ) ;
#25244 = DIRECTION ( 'NONE',  ( 0.005002170337468016433, -0.7660444431189770143, -0.6427681459581293666 ) ) ;
#25245 = FACE_OUTER_BOUND ( 'NONE', #37783, .T. ) ;
#25246 = DIRECTION ( 'NONE',  ( 0.005002170337468016433, -0.7660444431189770143, -0.6427681459581293666 ) ) ;
#25247 = EDGE_CURVE ( 'NONE', #8547, #722, #41714, .T. ) ;
#25248 = CARTESIAN_POINT ( 'NONE',  ( -14.15882808514179736, 0.000000000000000000, 6.756886256735718632 ) ) ;
#25249 = CARTESIAN_POINT ( 'NONE',  ( -23.33771345073609638, -0.1191753592594197858, 5.846786880686956955 ) ) ;
#25250 = VERTEX_POINT ( 'NONE', #11644 ) ;
#25251 = DIRECTION ( 'NONE',  ( 0.6427681459581294776, -0.7660444431189769032, 0.005002170337467562802 ) ) ;
#25252 = PLANE ( 'NONE',  #21443 ) ;
#25253 = EDGE_LOOP ( 'NONE', ( #22674, #52541, #32932, #43787 ) ) ;
#25254 = EDGE_CURVE ( 'NONE', #26165, #6886, #12754, .T. ) ;
#25255 = EDGE_LOOP ( 'NONE', ( #52432, #28655, #28533, #7191 ) ) ;
#25256 = CARTESIAN_POINT ( 'NONE',  ( -11.83276954743108256, 0.000000000000000000, 6.405656112318003359 ) ) ;
#25257 = ADVANCED_FACE ( 'NONE', ( #28960 ), #46252, .F. ) ;
#25258 = AXIS2_PLACEMENT_3D ( 'NONE', #4825, #21856, #9360 ) ;
#25259 = VERTEX_POINT ( 'NONE', #26361 ) ;
#25260 = EDGE_CURVE ( 'NONE', #34711, #22670, #25824, .T. ) ;
#25261 = CARTESIAN_POINT ( 'NONE',  ( -12.56204939715046720, 0.000000000000000000, 6.399980687897988574 ) ) ;
#25262 = ORIENTED_EDGE ( 'NONE', *, *, #23798, .F. ) ;
#25263 = VERTEX_POINT ( 'NONE', #30072 ) ;
#25264 = ORIENTED_EDGE ( 'NONE', *, *, #31100, .T. ) ;
#25265 = FACE_OUTER_BOUND ( 'NONE', #8371, .T. ) ;
#25266 = CARTESIAN_POINT ( 'NONE',  ( -14.56888064431065821, -0.1191753592594197858, 12.58947452739191064 ) ) ;
#25267 = CARTESIAN_POINT ( 'NONE',  ( -14.94916102560700821, 0.000000000000000000, 2.688082935172642962 ) ) ;
#25268 = ORIENTED_EDGE ( 'NONE', *, *, #49320, .T. ) ;
#25269 = ORIENTED_EDGE ( 'NONE', *, *, #39942, .F. ) ;
#25270 = CARTESIAN_POINT ( 'NONE',  ( -10.81400064959561469, -0.1159828484229834950, 7.418898672974625796 ) ) ;
#25271 = LINE ( 'NONE', #17037, #38173 ) ;
#25272 = ORIENTED_EDGE ( 'NONE', *, *, #23589, .F. ) ;
#25273 = LINE ( 'NONE', #38044, #2821 ) ;
#25274 = DIRECTION ( 'NONE',  ( -0.7660212471507179544, -0.6427876096865405842, -0.005961354470445141482 ) ) ;
#25275 = ORIENTED_EDGE ( 'NONE', *, *, #7360, .T. ) ;
#25276 = PLANE ( 'NONE',  #6744 ) ;
#25277 = CARTESIAN_POINT ( 'NONE',  ( -19.78515715608675762, 1.969473882990073754, 6.707120304835959779 ) ) ;
#25279 = VERTEX_POINT ( 'NONE', #17571 ) ;
#25278 = EDGE_CURVE ( 'NONE', #7048, #17764, #34602, .T. ) ;
#25280 = LINE ( 'NONE', #26375, #48180 ) ;
#25281 = EDGE_CURVE ( 'NONE', #48572, #34537, #26950, .T. ) ;
#25282 = ADVANCED_FACE ( 'NONE', ( #34909 ), #13862, .F. ) ;
#25283 = LINE ( 'NONE', #4276, #20018 ) ;
#25284 = ORIENTED_EDGE ( 'NONE', *, *, #21752, .T. ) ;
#25285 = DIRECTION ( 'NONE',  ( -0.5364919789714478471, 0.6444004775717705469, -0.5449076811759709926 ) ) ;
#25286 = PLANE ( 'NONE',  #4793 ) ;
#25287 = DIRECTION ( 'NONE',  ( 0.5449076811759707706, 0.6444004775717708799, -0.5364919789714476250 ) ) ;
#25288 = CARTESIAN_POINT ( 'NONE',  ( -17.40110780339754371, 0.000000000000000000, 5.423651820623570430 ) ) ;
#25289 = ORIENTED_EDGE ( 'NONE', *, *, #10620, .F. ) ;
#25290 = VECTOR ( 'NONE', #18228, 999.9999999999998863 ) ;
#25291 = DIRECTION ( 'NONE',  ( 0.007781995580012662783, 0.000000000000000000, -0.9999697198139514409 ) ) ;
#25292 = PLANE ( 'NONE',  #32340 ) ;
#25293 = CARTESIAN_POINT ( 'NONE',  ( -10.71056757118597069, 0.000000000000000000, 7.322379500780528794 ) ) ;
#25294 = FACE_OUTER_BOUND ( 'NONE', #52622, .T. ) ;
#25295 = LINE ( 'NONE', #42599, #26747 ) ;
#25296 = DIRECTION ( 'NONE',  ( 0.007781995580012663651, 0.000000000000000000, -0.9999697198139515519 ) ) ;
#25297 = EDGE_CURVE ( 'NONE', #23151, #23833, #48515, .T. ) ;
#25298 = CARTESIAN_POINT ( 'NONE',  ( -67.26331940870433357, -11.42107366115092226, -8.215550190278584353 ) ) ;
#25299 = VERTEX_POINT ( 'NONE', #21826 ) ;
#25300 = CARTESIAN_POINT ( 'NONE',  ( -67.09849928827489407, 4.336808689942017736E-15, 6.231849021622052121 ) ) ;
#25301 = ORIENTED_EDGE ( 'NONE', *, *, #24049, .F. ) ;
#25302 = CARTESIAN_POINT ( 'NONE',  ( -19.60834386242827776, 0.000000000000000000, 4.298478389818581213 ) ) ;
#25303 = PLANE ( 'NONE',  #55373 ) ;
#25304 = PLANE ( 'NONE',  #11340 ) ;
#25305 = DIRECTION ( 'NONE',  ( -0.9999697198139514409, -0.000000000000000000, -0.007781995580013368816 ) ) ;
#25306 = DIRECTION ( 'NONE',  ( -0.5449076811759708816, 0.6444004775717707689, 0.5364919789714475140 ) ) ;
#25307 = ORIENTED_EDGE ( 'NONE', *, *, #24144, .F. ) ;
#25308 = VERTEX_POINT ( 'NONE', #48210 ) ;
#25309 = DIRECTION ( 'NONE',  ( -0.005961354470445682716, -0.6427876096865404731, 0.7660212471507180654 ) ) ;
#25310 = DIRECTION ( 'NONE',  ( -0.005961354470445682716, -0.6427876096865404731, 0.7660212471507180654 ) ) ;
#25311 = VERTEX_POINT ( 'NONE', #35198 ) ;
#25312 = CARTESIAN_POINT ( 'NONE',  ( -50.02554558092695913, 3.776013638374815962, 5.000000000000000000 ) ) ;
#25313 = ORIENTED_EDGE ( 'NONE', *, *, #46376, .T. ) ;
#25314 = CARTESIAN_POINT ( 'NONE',  ( -24.26908309836554878, 0.000000000000000000, 6.108867788427308376 ) ) ;
#25315 = ADVANCED_FACE ( 'NONE', ( #47386 ), #21575, .F. ) ;
#25316 = ORIENTED_EDGE ( 'NONE', *, *, #37666, .F. ) ;
#25317 = FACE_OUTER_BOUND ( 'NONE', #50060, .T. ) ;
#25318 = ORIENTED_EDGE ( 'NONE', *, *, #3134, .T. ) ;
#25319 = VERTEX_POINT ( 'NONE', #9633 ) ;
#25320 = VERTEX_POINT ( 'NONE', #22672 ) ;
#25321 = CARTESIAN_POINT ( 'NONE',  ( -17.74404816805336793, 0.000000000000000000, 3.574322630375089460 ) ) ;
#25322 = CARTESIAN_POINT ( 'NONE',  ( 2.072287782118878319, 0.000000000000000000, -2.950529333540147015 ) ) ;
#25323 = CARTESIAN_POINT ( 'NONE',  ( -13.64701913762987573, 1.095915999411505526, 1.947931961135673129 ) ) ;
#25324 = EDGE_CURVE ( 'NONE', #16295, #38023, #53060, .T. ) ;
#25325 =( GEOMETRIC_REPRESENTATION_CONTEXT ( 3 ) GLOBAL_UNCERTAINTY_ASSIGNED_CONTEXT ( ( #2446 ) ) GLOBAL_UNIT_ASSIGNED_CONTEXT ( ( #16772, #8840, #22151 ) ) REPRESENTATION_CONTEXT ( 'NONE', 'WORKASPACE' ) );
#25326 = FACE_OUTER_BOUND ( 'NONE', #1464, .T. ) ;
#25327 = ORIENTED_EDGE ( 'NONE', *, *, #13822, .T. ) ;
#25328 = EDGE_CURVE ( 'NONE', #49293, #30466, #38889, .T. ) ;
#25329 = EDGE_CURVE ( 'NONE', #48860, #28185, #13335, .T. ) ;
#25330 = ORIENTED_EDGE ( 'NONE', *, *, #25353, .T. ) ;
#25331 = EDGE_LOOP ( 'NONE', ( #45488, #50601, #36175, #42621 ) ) ;
#25332 = DIRECTION ( 'NONE',  ( -0.5449076811759708816, 0.6444004775717707689, 0.5364919789714475140 ) ) ;
#25333 = FACE_OUTER_BOUND ( 'NONE', #28884, .T. ) ;
#25334 = VERTEX_POINT ( 'NONE', #44264 ) ;
#25335 = DIRECTION ( 'NONE',  ( 0.9999697198139515519, 0.000000000000000000, 0.007781995580013368816 ) ) ;
#25336 = ADVANCED_FACE ( 'NONE', ( #30367 ), #43421, .F. ) ;
#25337 = ORIENTED_EDGE ( 'NONE', *, *, #46582, .T. ) ;
#25338 = PLANE ( 'NONE',  #54141 ) ;
#25339 = CARTESIAN_POINT ( 'NONE',  ( -14.43628490643050277, 0.000000000000000000, 8.401381316409748834 ) ) ;
#25340 = EDGE_LOOP ( 'NONE', ( #29146, #26698, #14934, #9841 ) ) ;
#25341 = EDGE_CURVE ( 'NONE', #38808, #12870, #43150, .T. ) ;
#25342 = PLANE ( 'NONE',  #46767 ) ;
#25343 = EDGE_LOOP ( 'NONE', ( #33237, #52193, #72, #6999 ) ) ;
#25344 = ADVANCED_FACE ( 'NONE', ( #4259 ), #9323, .F. ) ;
#25345 = LINE ( 'NONE', #4344, #7417 ) ;
#25346 = CARTESIAN_POINT ( 'NONE',  ( -22.40556560354864146, -0.1191753592594197858, 5.484709000965211523 ) ) ;
#25347 = EDGE_LOOP ( 'NONE', ( #24525, #49569, #55096, #25368 ) ) ;
#25348 = FACE_OUTER_BOUND ( 'NONE', #18537, .T. ) ;
#25349 = LINE ( 'NONE', #43252, #42962 ) ;
#25350 = CARTESIAN_POINT ( 'NONE',  ( -13.80469194557137769, 2.391131607591508335, 1.967853275232125609 ) ) ;
#25351 = LINE ( 'NONE', #55169, #19199 ) ;
#25352 = ORIENTED_EDGE ( 'NONE', *, *, #10225, .T. ) ;
#25353 = EDGE_CURVE ( 'NONE', #35444, #30427, #47957, .T. ) ;
#25354 = ORIENTED_EDGE ( 'NONE', *, *, #22408, .F. ) ;
#25355 = CARTESIAN_POINT ( 'NONE',  ( -15.97319677381126013, -1.327505506330657781, 3.043498820269260552 ) ) ;
#25356 = CARTESIAN_POINT ( 'NONE',  ( -67.50810339439870233, 2.000000000000000000, 7.448312483692316022 ) ) ;
#25357 = LINE ( 'NONE', #42659, #18688 ) ;
#25358 = DIRECTION ( 'NONE',  ( 0.005961354470445682716, -0.6427876096865404731, -0.7660212471507180654 ) ) ;
#25359 = FACE_OUTER_BOUND ( 'NONE', #1622, .T. ) ;
#25360 = EDGE_CURVE ( 'NONE', #36655, #48938, #8497, .T. ) ;
#25361 = PLANE ( 'NONE',  #20415 ) ;
#25362 = EDGE_LOOP ( 'NONE', ( #21424, #35071, #34614, #42685 ) ) ;
#25363 = DIRECTION ( 'NONE',  ( 0.9999697198139515519, 0.000000000000000000, 0.007781995580013368816 ) ) ;
#25364 = PLANE ( 'NONE',  #49464 ) ;
#25365 = CARTESIAN_POINT ( 'NONE',  ( -17.43272239195565376, 0.000000000000000000, 9.486058556458980107 ) ) ;
#25366 = ORIENTED_EDGE ( 'NONE', *, *, #17134, .F. ) ;
#25367 = DIRECTION ( 'NONE',  ( 0.7660212471507180654, -0.6427876096865404731, 0.005961354470445141482 ) ) ;
#25368 = ORIENTED_EDGE ( 'NONE', *, *, #44572, .F. ) ;
#25369 = PRODUCT_DEFINITION_FORMATION_WITH_SPECIFIED_SOURCE ( 'ANY', '', #53221, .NOT_KNOWN. ) ;
#25370 = CARTESIAN_POINT ( 'NONE',  ( -21.93567689722629765, 19.99370688441071309, 4.408989160011352659 ) ) ;
#25371 = FACE_OUTER_BOUND ( 'NONE', #41883, .T. ) ;
#25372 = PLANE ( 'NONE',  #29613 ) ;
#25373 = CARTESIAN_POINT ( 'NONE',  ( -68.62740991863962847, 1.999999999996196598, 5.667235587295348154 ) ) ;
#25374 = ORIENTED_EDGE ( 'NONE', *, *, #27906, .F. ) ;
#25375 = ORIENTED_EDGE ( 'NONE', *, *, #2504, .F. ) ;
#25376 = CARTESIAN_POINT ( 'NONE',  ( -31.72782227498118601, 0.000000000000000000, 9.205484770164058972 ) ) ;
#25377 = LINE ( 'NONE', #42678, #6828 ) ;
#25378 = FACE_OUTER_BOUND ( 'NONE', #32815, .T. ) ;
#25379 = DIRECTION ( 'NONE',  ( -0.9999697198139514409, -0.000000000000000000, -0.007781995580013368816 ) ) ;
#25380 = DIRECTION ( 'NONE',  ( 0.5364919789714477361, 0.6444004775717706579, 0.5449076811759711036 ) ) ;
#25381 = CARTESIAN_POINT ( 'NONE',  ( -17.33011717104096405, -0.1117717739993967785, 9.949979618152523742 ) ) ;
#25382 = ADVANCED_FACE ( 'NONE', ( #9056 ), #43674, .F. ) ;
#25383 = EDGE_LOOP ( 'NONE', ( #26239, #11656, #6540, #826 ) ) ;
#25384 = CARTESIAN_POINT ( 'NONE',  ( -17.60792775650470077, -3.270328918600661883, 3.616497610996559420 ) ) ;
#25385 = FACE_OUTER_BOUND ( 'NONE', #13757, .T. ) ;
#25386 = LINE ( 'NONE', #3790, #43257 ) ;
#25387 = EDGE_LOOP ( 'NONE', ( #30710, #49651, #19940, #8721 ) ) ;
#25388 = CARTESIAN_POINT ( 'NONE',  ( -15.32400429664943609, 0.000000000000000000, 3.054497887970051284 ) ) ;
#25389 = DIRECTION ( 'NONE',  ( -0.5449076811759708816, 0.6444004775717707689, 0.5364919789714475140 ) ) ;
#25390 = CARTESIAN_POINT ( 'NONE',  ( -14.94916102560700821, 0.000000000000000000, 2.688082935172642962 ) ) ;
#25391 = VERTEX_POINT ( 'NONE', #10165 ) ;
#25392 = CARTESIAN_POINT ( 'NONE',  ( -18.67619601524082285, 0.000000000000000000, 3.936400510096834893 ) ) ;
#25393 = ORIENTED_EDGE ( 'NONE', *, *, #56233, .F. ) ;
#25394 = EDGE_CURVE ( 'NONE', #12113, #5158, #28053, .T. ) ;
#25395 = VECTOR ( 'NONE', #52183, 1000.000000000000227 ) ;
#25396 = ORIENTED_EDGE ( 'NONE', *, *, #35003, .T. ) ;
#25397 = VERTEX_POINT ( 'NONE', #45358 ) ;
#25398 = ORIENTED_EDGE ( 'NONE', *, *, #43167, .T. ) ;
#25399 = CARTESIAN_POINT ( 'NONE',  ( -9.808144436391993182, 0.000000000000000000, 10.77986332834118777 ) ) ;
#25400 = EDGE_LOOP ( 'NONE', ( #19133, #51411, #22665, #34057 ) ) ;
#25401 = DIRECTION ( 'NONE',  ( -0.005002170337468016433, -0.7660444431189770143, 0.6427681459581293666 ) ) ;
#25402 = ORIENTED_EDGE ( 'NONE', *, *, #48918, .T. ) ;
#25403 = CARTESIAN_POINT ( 'NONE',  ( -25.20278734466900517, 0.000000000000000000, 6.670939612111840944 ) ) ;
#25404 = EDGE_CURVE ( 'NONE', #42504, #21903, #40272, .T. ) ;
#25405 = ORIENTED_EDGE ( 'NONE', *, *, #12269, .F. ) ;
#25406 = ORIENTED_EDGE ( 'NONE', *, *, #10498, .F. ) ;
#25407 = ADVANCED_FACE ( 'NONE', ( #1650 ), #54175, .F. ) ;
#25408 = LINE ( 'NONE', #39310, #23845 ) ;
#25409 = CARTESIAN_POINT ( 'NONE',  ( -17.74560456716937296, 0.000000000000000000, 3.774316574337878372 ) ) ;
#25410 = DIRECTION ( 'NONE',  ( 0.005002170337468016433, -0.7660444431189770143, -0.6427681459581293666 ) ) ;
#25411 = CARTESIAN_POINT ( 'NONE',  ( -50.02554558092695913, 3.776013638374817294, 5.000000000000000000 ) ) ;
#25412 = DIRECTION ( 'NONE',  ( 0.005002170337468016433, -0.7660444431189770143, -0.6427681459581293666 ) ) ;
#25413 = ORIENTED_EDGE ( 'NONE', *, *, #25858, .T. ) ;
#25414 = EDGE_CURVE ( 'NONE', #12684, #42224, #36292, .T. ) ;
#25415 = ORIENTED_EDGE ( 'NONE', *, *, #458, .T. ) ;
#25416 = LINE ( 'NONE', #4130, #53951 ) ;
#25417 = LINE ( 'NONE', #39038, #4931 ) ;
#25418 = CARTESIAN_POINT ( 'NONE',  ( -11.16813870662720909, 0.000000000000000000, 6.410828423202016069 ) ) ;
#25419 = ADVANCED_FACE ( 'NONE', ( #36872 ), #23251, .F. ) ;
#25420 = DIRECTION ( 'NONE',  ( 0.000000000000000000, 0.000000000000000000, 1.000000000000000000 ) ) ;
#25421 = DIRECTION ( 'NONE',  ( 0.000000000000000000, -0.000000000000000000, -1.000000000000000000 ) ) ;
#25422 = FACE_OUTER_BOUND ( 'NONE', #16587, .T. ) ;
#25423 = VERTEX_POINT ( 'NONE', #2488 ) ;
#25424 = LINE ( 'NONE', #42476, #14795 ) ;
#25425 = LINE ( 'NONE', #119, #41290 ) ;
#25426 = ORIENTED_EDGE ( 'NONE', *, *, #9306, .T. ) ;
#25427 = LINE ( 'NONE', #8693, #31585 ) ;
#25428 = DIRECTION ( 'NONE',  ( 0.000000000000000000, -1.000000000000000000, 0.000000000000000000 ) ) ;
#25429 = LINE ( 'NONE', #40094, #29074 ) ;
#25430 = DIRECTION ( 'NONE',  ( -0.6427681459581293666, -0.7660444431189770143, -0.005002170337467561935 ) ) ;
#25431 = DIRECTION ( 'NONE',  ( 0.005961354470445682716, -0.6427876096865404731, -0.7660212471507180654 ) ) ;
#25432 = AXIS2_PLACEMENT_3D ( 'NONE', #54401, #7017, #55521 ) ;
#25433 = ORIENTED_EDGE ( 'NONE', *, *, #15801, .F. ) ;
#25434 = ORIENTED_EDGE ( 'NONE', *, *, #16928, .F. ) ;
#25435 = CARTESIAN_POINT ( 'NONE',  ( -56.48844206942440138, 5.522788861961955398, 2.999999999999993339 ) ) ;
#25436 = DIRECTION ( 'NONE',  ( 0.9999697198139515519, 0.000000000000000000, 0.007781995580013368816 ) ) ;
#25437 = CARTESIAN_POINT ( 'NONE',  ( -24.26986129792355129, -0.1191753592594197858, 6.208864760408702388 ) ) ;
#25438 = DIRECTION ( 'NONE',  ( 0.007781995580012662783, 0.000000000000000000, -0.9999697198139514409 ) ) ;
#25439 = DIRECTION ( 'NONE',  ( 0.000000000000000000, -1.000000000000000000, 0.000000000000000000 ) ) ;
#25440 = EDGE_CURVE ( 'NONE', #20904, #9112, #40573, .T. ) ;
#25441 = DIRECTION ( 'NONE',  ( 0.000000000000000000, -0.000000000000000000, -1.000000000000000000 ) ) ;
#25442 = DIRECTION ( 'NONE',  ( 0.7660212471507180654, -0.6427876096865404731, 0.005961354470445141482 ) ) ;
#25443 = CARTESIAN_POINT ( 'NONE',  ( -10.94028622754223967, 0.000000000000000000, 11.14038480894692995 ) ) ;
#25444 = DIRECTION ( 'NONE',  ( 0.005002170337468016433, -0.7660444431189770143, -0.6427681459581293666 ) ) ;
#25445 = EDGE_CURVE ( 'NONE', #49287, #55547, #18977, .T. ) ;
#25446 = ADVANCED_FACE ( 'NONE', ( #27486 ), #53601, .F. ) ;
#25447 = DIRECTION ( 'NONE',  ( 0.6427681459581294776, -0.7660444431189769032, 0.005002170337467562802 ) ) ;
#25448 = VERTEX_POINT ( 'NONE', #45633 ) ;
#25449 = CARTESIAN_POINT ( 'NONE',  ( -9.110551994824897193, -1.000000000000000000, 3.538847790438064411 ) ) ;
#25450 = EDGE_CURVE ( 'NONE', #41560, #42137, #10467, .T. ) ;
#25451 = ADVANCED_FACE ( 'NONE', ( #53349 ), #48805, .F. ) ;
#25452 = ADVANCED_FACE ( 'NONE', ( #27210 ), #32333, .F. ) ;
#25453 = VERTEX_POINT ( 'NONE', #14443 ) ;
#25454 = ORIENTED_EDGE ( 'NONE', *, *, #55907, .T. ) ;
#25455 = VERTEX_POINT ( 'NONE', #1366 ) ;
#25456 = VERTEX_POINT ( 'NONE', #18710 ) ;
#25457 = EDGE_LOOP ( 'NONE', ( #29647, #39330, #33391, #5157 ) ) ;
#25458 = VERTEX_POINT ( 'NONE', #31759 ) ;
#25459 = CARTESIAN_POINT ( 'NONE',  ( -15.46582147666606488, -0.1117717739994045917, 9.225823858709038205 ) ) ;
#25460 = CARTESIAN_POINT ( 'NONE',  ( -12.70037056462282088, 3.848249166794011522, 1.492407668973236845 ) ) ;
#25461 = DIRECTION ( 'NONE',  ( -0.9999697198139514409, -0.000000000000000000, -0.007781995580013368816 ) ) ;
#25462 = VECTOR ( 'NONE', #14266, 999.9999999999998863 ) ;
#25463 = EDGE_LOOP ( 'NONE', ( #9139, #33078, #62, #27766 ) ) ;
#25464 = CARTESIAN_POINT ( 'NONE',  ( -21.47263955680318404, 0.000000000000000000, 5.022634149262071190 ) ) ;
#25465 = EDGE_CURVE ( 'NONE', #37343, #49177, #49350, .T. ) ;
#25466 = ORIENTED_EDGE ( 'NONE', *, *, #32249, .F. ) ;
#25467 = PLANE ( 'NONE',  #52210 ) ;
#25468 = ORIENTED_EDGE ( 'NONE', *, *, #28468, .T. ) ;
#25469 = AXIS2_PLACEMENT_3D ( 'NONE', #513, #5347, #203 ) ;
#25470 = EDGE_CURVE ( 'NONE', #41524, #48104, #6211, .T. ) ;
#25471 = DIRECTION ( 'NONE',  ( -0.9999697198139514409, -0.000000000000000000, -0.007781995580013368816 ) ) ;
#25472 = EDGE_CURVE ( 'NONE', #18589, #16426, #1903, .T. ) ;
#25473 = DIRECTION ( 'NONE',  ( 0.005961354470445682716, -0.6427876096865404731, -0.7660212471507180654 ) ) ;
#25474 = DIRECTION ( 'NONE',  ( 0.005961354470445682716, -0.6427876096865404731, -0.7660212471507180654 ) ) ;
#25475 = EDGE_LOOP ( 'NONE', ( #26327, #9052, #42475, #45661 ) ) ;
#25476 = CARTESIAN_POINT ( 'NONE',  ( -17.20973601995061131, 0.000000000000000000, 6.533137329512866742 ) ) ;
#25477 = VERTEX_POINT ( 'NONE', #49648 ) ;
#25478 = EDGE_CURVE ( 'NONE', #441, #29890, #10746, .T. ) ;
#25479 = CARTESIAN_POINT ( 'NONE',  ( -31.72782227498118601, 0.000000000000000000, 9.205484770164058972 ) ) ;
#25480 = DIRECTION ( 'NONE',  ( 0.8531650599175529814, -0.4028455766673920135, -0.3313982828793697877 ) ) ;
#25481 = DIRECTION ( 'NONE',  ( 0.6427681459581294776, -0.7660444431189769032, 0.005002170337467562802 ) ) ;
#25482 = FACE_OUTER_BOUND ( 'NONE', #33316, .T. ) ;
#25483 = CARTESIAN_POINT ( 'NONE',  ( -20.38711805380392406, 1.905425754524007642, 4.540187675463392303 ) ) ;
#25484 = LINE ( 'NONE', #47640, #53892 ) ;
#25485 = PLANE ( 'NONE',  #41166 ) ;
#25486 = CARTESIAN_POINT ( 'NONE',  ( -68.75329340164451253, -8.572274407770869686, 6.394134653913044808 ) ) ;
#25487 = ORIENTED_EDGE ( 'NONE', *, *, #10020, .F. ) ;
#25488 = CARTESIAN_POINT ( 'NONE',  ( -55.63255288014424593, 6.714018351055213607, -1.412117554830255362 ) ) ;
#25489 = ORIENTED_EDGE ( 'NONE', *, *, #20970, .F. ) ;
#25490 = VECTOR ( 'NONE', #27841, 1000.000000000000227 ) ;
#25491 = VECTOR ( 'NONE', #311, 999.9999999999998863 ) ;
#25492 = CARTESIAN_POINT ( 'NONE',  ( -16.94256912529133174, -4.079838673713161334, 9.958711274498135424 ) ) ;
#25493 = DIRECTION ( 'NONE',  ( 0.007781995580012663651, 0.000000000000000000, -0.9999697198139515519 ) ) ;
#25494 = FACE_OUTER_BOUND ( 'NONE', #19036, .T. ) ;
#25495 = CARTESIAN_POINT ( 'NONE',  ( -17.85327294482519633, -1.327505506330656893, 5.795411938479114511 ) ) ;
#25496 = DIRECTION ( 'NONE',  ( 0.007781995580012662783, 0.000000000000000000, -0.9999697198139514409 ) ) ;
#25497 = FACE_OUTER_BOUND ( 'NONE', #36928, .T. ) ;
#25498 = ORIENTED_EDGE ( 'NONE', *, *, #12906, .F. ) ;
#25499 = PLANE ( 'NONE',  #27528 ) ;
#25500 = LINE ( 'NONE', #46228, #33096 ) ;
#25501 = DIRECTION ( 'NONE',  ( -0.5449076811759708816, 0.6444004775717707689, 0.5364919789714475140 ) ) ;
#25502 = AXIS2_PLACEMENT_3D ( 'NONE', #19255, #15544, #24091 ) ;
#25503 = DIRECTION ( 'NONE',  ( 0.000000000000000000, -1.000000000000000000, 0.000000000000000000 ) ) ;
#25504 = DIRECTION ( 'NONE',  ( 0.6427681459581294776, -0.7660444431189769032, 0.005002170337467562802 ) ) ;
#25505 = CARTESIAN_POINT ( 'NONE',  ( -15.46920792515735243, -0.1191753592594181482, 8.862677968554882213 ) ) ;
#25506 = CARTESIAN_POINT ( 'NONE',  ( -21.47419595591918906, 0.000000000000000000, 5.222628093224860102 ) ) ;
#25507 = ORIENTED_EDGE ( 'NONE', *, *, #28090, .F. ) ;
#25508 = AXIS2_PLACEMENT_3D ( 'NONE', #18130, #48524, #9639 ) ;
#25509 = LINE ( 'NONE', #55610, #50294 ) ;
#25510 = DIRECTION ( 'NONE',  ( -0.9999697198139514409, -0.000000000000000000, -0.007781995580013368816 ) ) ;
#25511 = ORIENTED_EDGE ( 'NONE', *, *, #46279, .T. ) ;
#25512 = ORIENTED_EDGE ( 'NONE', *, *, #31540, .F. ) ;
#25513 = LINE ( 'NONE', #54770, #14709 ) ;
#25514 = EDGE_CURVE ( 'NONE', #329, #14660, #33694, .T. ) ;
#25515 = EDGE_CURVE ( 'NONE', #13391, #33224, #37973, .T. ) ;
#25516 = ORIENTED_EDGE ( 'NONE', *, *, #15748, .F. ) ;
#25517 = EDGE_CURVE ( 'NONE', #30666, #25884, #33993, .T. ) ;
#25518 = ORIENTED_EDGE ( 'NONE', *, *, #24498, .F. ) ;
#25519 = ORIENTED_EDGE ( 'NONE', *, *, #33502, .T. ) ;
#25520 = ORIENTED_EDGE ( 'NONE', *, *, #23547, .T. ) ;
#25521 = CARTESIAN_POINT ( 'NONE',  ( 5.221828392167460642, 0.000000000000000000, -2.393421119419572918 ) ) ;
#25522 = ORIENTED_EDGE ( 'NONE', *, *, #38891, .F. ) ;
#25523 = DIRECTION ( 'NONE',  ( 0.5364919789714477361, 0.6444004775717706579, 0.5449076811759711036 ) ) ;
#25524 = CARTESIAN_POINT ( 'NONE',  ( -12.99926341332800739, 0.000000000000000000, 2.872583502847308790 ) ) ;
#25525 = VECTOR ( 'NONE', #43050, 999.9999999999998863 ) ;
#25526 = VECTOR ( 'NONE', #18138, 999.9999999999998863 ) ;
#25527 = ORIENTED_EDGE ( 'NONE', *, *, #41292, .T. ) ;
#25528 = VERTEX_POINT ( 'NONE', #11577 ) ;
#25529 = EDGE_CURVE ( 'NONE', #35066, #28129, #51318, .T. ) ;
#25530 = VECTOR ( 'NONE', #12096, 1000.000000000000227 ) ;
#25531 = CARTESIAN_POINT ( 'NONE',  ( 5.912796793901484271, -6.204513306124835204, 2.260536671351836002 ) ) ;
#25532 = DIRECTION ( 'NONE',  ( 0.005002170337468016433, -0.7660444431189770143, -0.6427681459581293666 ) ) ;
#25533 = ORIENTED_EDGE ( 'NONE', *, *, #11938, .T. ) ;
#25534 = ADVANCED_FACE ( 'NONE', ( #7582 ), #2736, .F. ) ;
#25535 = DIRECTION ( 'NONE',  ( 0.005961354470445682716, -0.6427876096865404731, -0.7660212471507180654 ) ) ;
#25536 = DIRECTION ( 'NONE',  ( 0.5449076811759707706, 0.6444004775717708799, -0.5364919789714476250 ) ) ;
#25537 = ORIENTED_EDGE ( 'NONE', *, *, #34115, .F. ) ;
#25538 = FACE_OUTER_BOUND ( 'NONE', #7919, .T. ) ;
#25539 = VERTEX_POINT ( 'NONE', #3026 ) ;
#25540 = EDGE_CURVE ( 'NONE', #50681, #41476, #47050, .T. ) ;
#25541 = LINE ( 'NONE', #42858, #17335 ) ;
#25542 = ADVANCED_FACE ( 'NONE', ( #16113 ), #7895, .F. ) ;
#25543 = AXIS2_PLACEMENT_3D ( 'NONE', #36733, #15166, #32482 ) ;
#25544 = CARTESIAN_POINT ( 'NONE',  ( -10.86644437236699190, 1.095915999411505082, 2.900801997477032934 ) ) ;
#25545 = ORIENTED_EDGE ( 'NONE', *, *, #10311, .F. ) ;
#25546 = PLANE ( 'NONE',  #54858 ) ;
#25547 = CARTESIAN_POINT ( 'NONE',  ( -15.80432911540621532, 0.000000000000000000, 5.066746251785837707 ) ) ;
#25548 = FACE_OUTER_BOUND ( 'NONE', #20490, .T. ) ;
#25549 = LINE ( 'NONE', #43697, #46424 ) ;
#25550 = ORIENTED_EDGE ( 'NONE', *, *, #2171, .F. ) ;
#25551 = DIRECTION ( 'NONE',  ( -0.5449076811759708816, 0.6444004775717707689, 0.5364919789714475140 ) ) ;
#25552 = CARTESIAN_POINT ( 'NONE',  ( -10.20437627088164589, 0.000000000000000000, 1.986343807644861847 ) ) ;
#25553 = CARTESIAN_POINT ( 'NONE',  ( -9.542064456761055524, 0.000000000000000000, 10.59726798936431180 ) ) ;
#25554 = CARTESIAN_POINT ( 'NONE',  ( -17.57658898651670043, -1.003701604285656579, 5.156521124944394074 ) ) ;
#25555 = DIRECTION ( 'NONE',  ( 0.9321478471874541372, 0.000000000000000000, -0.3620778797217453771 ) ) ;
#25556 = LINE ( 'NONE', #15929, #46981 ) ;
#25557 = DIRECTION ( 'NONE',  ( 0.5364919789714477361, 0.6444004775717706579, 0.5449076811759711036 ) ) ;
#25558 = DIRECTION ( 'NONE',  ( 0.007781995580012663651, 0.000000000000000000, -0.9999697198139515519 ) ) ;
#25559 = ORIENTED_EDGE ( 'NONE', *, *, #42500, .T. ) ;
#25560 = PLANE ( 'NONE',  #10590 ) ;
#25561 = EDGE_LOOP ( 'NONE', ( #10605, #18281, #37316, #21489 ) ) ;
#25562 = DIRECTION ( 'NONE',  ( 0.005002170337468016433, -0.7660444431189770143, -0.6427681459581293666 ) ) ;
#25563 = DIRECTION ( 'NONE',  ( -0.1139275668495183524, 0.9934890585767659488, 4.694855797473114533E-16 ) ) ;
#25564 = VECTOR ( 'NONE', #16287, 1000.000000000000000 ) ;
#25565 = VECTOR ( 'NONE', #49791, 1000.000000000000227 ) ;
#25566 = FACE_OUTER_BOUND ( 'NONE', #9819, .T. ) ;
#25567 = PLANE ( 'NONE',  #43282 ) ;
#25568 = CARTESIAN_POINT ( 'NONE',  ( -50.45472955569960760, 3.742236127018431890, -5.000000000000000000 ) ) ;
#25569 = ORIENTED_EDGE ( 'NONE', *, *, #35117, .F. ) ;
#25570 = VECTOR ( 'NONE', #5390, 1000.000000000000000 ) ;
#25571 = ORIENTED_EDGE ( 'NONE', *, *, #28833, .F. ) ;
#25572 = CARTESIAN_POINT ( 'NONE',  ( -10.94028622754223967, 0.000000000000000000, 11.14038480894692995 ) ) ;
#25573 = CARTESIAN_POINT ( 'NONE',  ( -17.72157301408583763, -5.536956232915663634, 12.65268099554350911 ) ) ;
#25574 = ORIENTED_EDGE ( 'NONE', *, *, #640, .T. ) ;
#25575 = DIRECTION ( 'NONE',  ( 0.000000000000000000, -0.000000000000000000, -1.000000000000000000 ) ) ;
#25576 = EDGE_CURVE ( 'NONE', #23017, #7084, #35620, .T. ) ;
#25577 = ORIENTED_EDGE ( 'NONE', *, *, #20249, .T. ) ;
#25578 = CARTESIAN_POINT ( 'NONE',  ( -10.94028622754223967, 0.000000000000000000, 11.14038480894692995 ) ) ;
#25579 = AXIS2_PLACEMENT_3D ( 'NONE', #49855, #27742, #28014 ) ;
#25580 = ORIENTED_EDGE ( 'NONE', *, *, #27181, .T. ) ;
#25581 = DIRECTION ( 'NONE',  ( 0.000000000000000000, -1.000000000000000000, 0.000000000000000000 ) ) ;
#25582 = EDGE_CURVE ( 'NONE', #54876, #43321, #29150, .T. ) ;
#25583 = ADVANCED_FACE ( 'NONE', ( #46773 ), #16661, .F. ) ;
#25584 = ORIENTED_EDGE ( 'NONE', *, *, #26249, .T. ) ;
#25585 = ORIENTED_EDGE ( 'NONE', *, *, #45164, .F. ) ;
#25586 = ORIENTED_EDGE ( 'NONE', *, *, #49587, .T. ) ;
#25587 = LINE ( 'NONE', #39207, #13898 ) ;
#25588 = FACE_OUTER_BOUND ( 'NONE', #50226, .T. ) ;
#25589 = DIRECTION ( 'NONE',  ( 0.007781995580012663651, -3.146120232559066537E-19, -0.9999697198139514409 ) ) ;
#25590 = PLANE ( 'NONE',  #25759 ) ;
#25591 = EDGE_LOOP ( 'NONE', ( #35050, #16668, #20578, #54715 ) ) ;
#25592 = ORIENTED_EDGE ( 'NONE', *, *, #25697, .T. ) ;
#25593 = AXIS2_PLACEMENT_3D ( 'NONE', #17981, #48642, #13987 ) ;
#25594 = ORIENTED_EDGE ( 'NONE', *, *, #10903, .T. ) ;
#25595 = CARTESIAN_POINT ( 'NONE',  ( -16.79925329029790149, 0.000000000000000000, 13.49544742625427496 ) ) ;
#25596 = LINE ( 'NONE', #21051, #7696 ) ;
#25597 = ORIENTED_EDGE ( 'NONE', *, *, #2751, .T. ) ;
#25598 = VECTOR ( 'NONE', #30776, 1000.000000000000227 ) ;
#25599 = DIRECTION ( 'NONE',  ( 0.000000000000000000, -1.000000000000000000, 0.000000000000000000 ) ) ;
#25600 = ORIENTED_EDGE ( 'NONE', *, *, #36713, .T. ) ;
#25601 = DIRECTION ( 'NONE',  ( 0.000000000000000000, -0.000000000000000000, -1.000000000000000000 ) ) ;
#25602 = CARTESIAN_POINT ( 'NONE',  ( -17.74560456716937296, 0.000000000000000000, 3.774316574337878372 ) ) ;
#25603 = AXIS2_PLACEMENT_3D ( 'NONE', #17861, #18384, #14158 ) ;
#25604 = AXIS2_PLACEMENT_3D ( 'NONE', #13610, #34095, #43179 ) ;
#25605 = ORIENTED_EDGE ( 'NONE', *, *, #35255, .F. ) ;
#25606 = CARTESIAN_POINT ( 'NONE',  ( -15.85727731971092780, -5.536956232915663634, 11.92852523610001647 ) ) ;
#25607 = ORIENTED_EDGE ( 'NONE', *, *, #50078, .F. ) ;
#25608 = EDGE_CURVE ( 'NONE', #54304, #7819, #3874, .T. ) ;
#25609 = AXIS2_PLACEMENT_3D ( 'NONE', #50791, #12485, #17018 ) ;
#25610 = DIRECTION ( 'NONE',  ( -0.5449076811759708816, 0.6444004775717707689, 0.5364919789714475140 ) ) ;
#25611 = CARTESIAN_POINT ( 'NONE',  ( -21.59172106477361908, 2.229229656569007734, 4.997765353639686658 ) ) ;
#25612 = VECTOR ( 'NONE', #23747, 999.9999999999998863 ) ;
#25614 = EDGE_CURVE ( 'NONE', #46401, #16128, #54428, .T. ) ;
#25613 = ORIENTED_EDGE ( 'NONE', *, *, #17522, .T. ) ;
#25615 = LINE ( 'NONE', #42941, #2330 ) ;
#25616 = LINE ( 'NONE', #38116, #13933 ) ;
#25617 = LINE ( 'NONE', #52850, #11047 ) ;
#25618 = EDGE_CURVE ( 'NONE', #38527, #23133, #45936, .T. ) ;
#25619 = VERTEX_POINT ( 'NONE', #32856 ) ;
#25620 = PLANE ( 'NONE',  #47337 ) ;
#25621 = ADVANCED_FACE ( 'NONE', ( #50174 ), #7045, .F. ) ;
#25622 = LINE ( 'NONE', #52326, #51216 ) ;
#25623 = STYLED_ITEM ( 'NONE', ( #5509 ), #2589 ) ;
#25624 = DIRECTION ( 'NONE',  ( 0.007781995580012663651, 0.000000000000000000, -0.9999697198139515519 ) ) ;
#25625 = DIRECTION ( 'NONE',  ( -0.5364919789714478471, 0.6444004775717705469, -0.5449076811759709926 ) ) ;
#25626 = CARTESIAN_POINT ( 'NONE',  ( -11.72846197273706537, -3.432230869623159819, 6.870540248819963836 ) ) ;
#25627 = LINE ( 'NONE', #55177, #16770 ) ;
#25628 = ORIENTED_EDGE ( 'NONE', *, *, #54297, .F. ) ;
#25629 = DIRECTION ( 'NONE',  ( 0.007781995580012663651, 0.000000000000000000, -0.9999697198139515519 ) ) ;
#25630 = CARTESIAN_POINT ( 'NONE',  ( 2.072287782118878319, 0.000000000000000000, -2.950529333540147015 ) ) ;
#25631 = DIRECTION ( 'NONE',  ( -0.005002170337468016433, -0.7660444431189770143, 0.6427681459581293666 ) ) ;
#25632 = EDGE_LOOP ( 'NONE', ( #47, #34599, #16109, #9951 ) ) ;
#25633 = LINE ( 'NONE', #35027, #19324 ) ;
#25634 = CARTESIAN_POINT ( 'NONE',  ( 2.072287782118878319, 0.000000000000000000, -2.950529333540147015 ) ) ;
#25635 = EDGE_LOOP ( 'NONE', ( #6814, #30191, #4844, #54849 ) ) ;
#25636 = CYLINDRICAL_SURFACE ( 'NONE', #8071, 3.000000000000001332 ) ;
#25637 = DIRECTION ( 'NONE',  ( 0.007781995580012663651, -3.146120232559066537E-19, -0.9999697198139514409 ) ) ;
#25638 = VECTOR ( 'NONE', #51436, 1000.000000000000227 ) ;
#25639 = EDGE_CURVE ( 'NONE', #46062, #25455, #37385, .T. ) ;
#25640 = CARTESIAN_POINT ( 'NONE',  ( -16.33317936670417225, 0.000000000000000000, 13.31440848639340224 ) ) ;
#25641 = CARTESIAN_POINT ( 'NONE',  ( -65.68698218762608576, 2.000000000000004441, 3.192571262220380124 ) ) ;
#25642 = ORIENTED_EDGE ( 'NONE', *, *, #19738, .T. ) ;
#25643 = ORIENTED_EDGE ( 'NONE', *, *, #41587, .F. ) ;
#25644 = FACE_OUTER_BOUND ( 'NONE', #49140, .T. ) ;
#25645 = PLANE ( 'NONE',  #17741 ) ;
#25646 = AXIS2_PLACEMENT_3D ( 'NONE', #32991, #1506, #50303 ) ;
#25647 = CARTESIAN_POINT ( 'NONE',  ( -17.16584333050165867, 0.2864062442990034651, 4.019159061553319034 ) ) ;
#25648 = EDGE_CURVE ( 'NONE', #6528, #40301, #50477, .T. ) ;
#25649 = VECTOR ( 'NONE', #27703, 1000.000000000000227 ) ;
#25650 = CARTESIAN_POINT ( 'NONE',  ( -11.79385045274640653, 0.000000000000000000, 1.404636026004276284 ) ) ;
#25651 = VECTOR ( 'NONE', #43105, 1000.000000000000227 ) ;
#25652 = LINE ( 'NONE', #43533, #47331 ) ;
#25653 = ADVANCED_FACE ( 'NONE', ( #4463 ), #13534, .F. ) ;
#25654 = LINE ( 'NONE', #11755, #50293 ) ;
#25655 = VERTEX_POINT ( 'NONE', #753 ) ;
#25656 = CARTESIAN_POINT ( 'NONE',  ( -19.83058694132466115, 4.495856970884009485, 11.96266175778294816 ) ) ;
#25657 = EDGE_CURVE ( 'NONE', #41831, #42740, #17501, .T. ) ;
#25658 = EDGE_CURVE ( 'NONE', #53603, #7239, #52438, .T. ) ;
#25659 = VECTOR ( 'NONE', #31953, 999.9999999999998863 ) ;
#25660 = CARTESIAN_POINT ( 'NONE',  ( -16.53317331066696383, 0.000000000000000000, 13.31285208727739899 ) ) ;
#25661 = VECTOR ( 'NONE', #28425, 1000.000000000000227 ) ;
#25662 = ORIENTED_EDGE ( 'NONE', *, *, #17021, .T. ) ;
#25663 = CARTESIAN_POINT ( 'NONE',  ( -21.47263955680318404, 0.000000000000000000, 5.022634149262071190 ) ) ;
#25664 = LINE ( 'NONE', #56063, #9587 ) ;
#25665 = DIRECTION ( 'NONE',  ( 0.005961354470445682716, -0.6427876096865404731, -0.7660212471507180654 ) ) ;
#25666 = ORIENTED_EDGE ( 'NONE', *, *, #50126, .F. ) ;
#25667 = PRODUCT_DEFINITION ( 'UNKNOWN', '', #28076, #42725 ) ;
#25668 = DIRECTION ( 'NONE',  ( 0.9999697198139515519, 0.000000000000000000, 0.007781995580013368816 ) ) ;
#25669 = VECTOR ( 'NONE', #32878, 1000.000000000000227 ) ;
#25670 = ORIENTED_EDGE ( 'NONE', *, *, #35106, .T. ) ;
#25671 = AXIS2_PLACEMENT_3D ( 'NONE', #26304, #17500, #8151 ) ;
#25672 = EDGE_CURVE ( 'NONE', #36758, #23095, #34837, .T. ) ;
#25673 = ORIENTED_EDGE ( 'NONE', *, *, #19176, .F. ) ;
#25674 = VERTEX_POINT ( 'NONE', #8735 ) ;
#25675 = VERTEX_POINT ( 'NONE', #56135 ) ;
#25676 = CARTESIAN_POINT ( 'NONE',  ( -21.47419595591918906, 0.000000000000000000, 5.222628093224860102 ) ) ;
#25677 = ORIENTED_EDGE ( 'NONE', *, *, #9618, .F. ) ;
#25678 = AXIS2_PLACEMENT_3D ( 'NONE', #6100, #1787, #36183 ) ;
#25679 = CARTESIAN_POINT ( 'NONE',  ( -13.72345201801339165, 23.00298632150112255, -3.759965536548706133 ) ) ;
#25680 = EDGE_LOOP ( 'NONE', ( #37878, #53814, #39047, #36632 ) ) ;
#25681 = PLANE ( 'NONE',  #11363 ) ;
#25682 = ORIENTED_EDGE ( 'NONE', *, *, #2315, .T. ) ;
#25683 = PLANE ( 'NONE',  #26628 ) ;
#25684 = AXIS2_PLACEMENT_3D ( 'NONE', #34395, #52282, #25575 ) ;
#25685 = ORIENTED_EDGE ( 'NONE', *, *, #26188, .F. ) ;
#25686 = CARTESIAN_POINT ( 'NONE',  ( -33.59211796935609584, 0.000000000000000000, 9.929640529607549837 ) ) ;
#25687 = CARTESIAN_POINT ( 'NONE',  ( -66.74342152241241877, -11.36145478494482042, -7.448289400635804469 ) ) ;
#25688 = DIRECTION ( 'NONE',  ( -0.6427681459581293666, -0.7660444431189770143, -0.005002170337467561935 ) ) ;
#25689 = CARTESIAN_POINT ( 'NONE',  ( -15.93671887550372013, -0.1191753592594204797, 9.228371760044637995 ) ) ;
#25690 = VECTOR ( 'NONE', #3397, 1000.000000000000000 ) ;
#25691 = FACE_OUTER_BOUND ( 'NONE', #18002, .T. ) ;
#25692 = ORIENTED_EDGE ( 'NONE', *, *, #12877, .T. ) ;
#25693 = AXIS2_PLACEMENT_3D ( 'NONE', #27293, #633, #35536 ) ;
#25694 = AXIS2_PLACEMENT_3D ( 'NONE', #35233, #43194, #581 ) ;
#25695 = ORIENTED_EDGE ( 'NONE', *, *, #5405, .T. ) ;
#25696 = CARTESIAN_POINT ( 'NONE',  ( -8.875996589204540044, 0.000000000000000000, 10.41778544861944233 ) ) ;
#25697 = EDGE_CURVE ( 'NONE', #26758, #15321, #17224, .T. ) ;
#25698 = DIRECTION ( 'NONE',  ( -0.7660212471507179544, -0.6427876096865405842, -0.005961354470445141482 ) ) ;
#25699 = LINE ( 'NONE', #38189, #33328 ) ;
#25700 = VECTOR ( 'NONE', #29219, 999.9999999999998863 ) ;
#25701 = VECTOR ( 'NONE', #13311, 1000.000000000000000 ) ;
#25702 = DIRECTION ( 'NONE',  ( 0.5364919789714477361, 0.6444004775717706579, 0.5449076811759711036 ) ) ;
#25703 = CARTESIAN_POINT ( 'NONE',  ( -13.22668023795434067, 0.000000000000000000, 6.394808377013974976 ) ) ;
#25704 = CARTESIAN_POINT ( 'NONE',  ( -18.66354898467281132, 0.000000000000000000, 14.21960318569776582 ) ) ;
#25705 = EDGE_LOOP ( 'NONE', ( #52805, #36626, #51445, #56194 ) ) ;
#25706 = CARTESIAN_POINT ( 'NONE',  ( -22.15388463660123719, -4.241740624735662379, 5.351308525247191916 ) ) ;
#25707 = DIRECTION ( 'NONE',  ( 0.7660212471507180654, -0.6427876096865404731, 0.005961354470445141482 ) ) ;
#25708 = EDGE_LOOP ( 'NONE', ( #50280, #34062, #6423, #6818 ) ) ;
#25709 = EDGE_CURVE ( 'NONE', #9950, #33621, #21770, .T. ) ;
#25710 = DIRECTION ( 'NONE',  ( 0.9999697198139515519, 0.000000000000000000, 0.007781995580013368816 ) ) ;
#25711 = LINE ( 'NONE', #423, #41464 ) ;
#25712 = LINE ( 'NONE', #20880, #26840 ) ;
#25713 = EDGE_CURVE ( 'NONE', #53889, #6987, #43073, .T. ) ;
#25714 = EDGE_CURVE ( 'NONE', #20361, #52593, #22352, .T. ) ;
#25715 = DIRECTION ( 'NONE',  ( -0.5364919789714478471, 0.6444004775717705469, -0.5449076811759709926 ) ) ;
#25716 = ORIENTED_EDGE ( 'NONE', *, *, #49039, .T. ) ;
#25717 = VECTOR ( 'NONE', #48878, 1000.000000000000114 ) ;
#25718 = ORIENTED_EDGE ( 'NONE', *, *, #2580, .F. ) ;
#25719 = DIRECTION ( 'NONE',  ( 0.000000000000000000, -0.000000000000000000, -1.000000000000000000 ) ) ;
#25720 = DIRECTION ( 'NONE',  ( -0.5449076811759708816, 0.6444004775717707689, 0.5364919789714475140 ) ) ;
#25721 = DIRECTION ( 'NONE',  ( 0.007781995580012662783, 0.000000000000000000, -0.9999697198139514409 ) ) ;
#25722 = EDGE_CURVE ( 'NONE', #11534, #55481, #39674, .T. ) ;
#25723 = AXIS2_PLACEMENT_3D ( 'NONE', #27503, #44532, #6484 ) ;
#25724 = ADVANCED_FACE ( 'NONE', ( #16966 ), #18070, .F. ) ;
#25725 = FACE_OUTER_BOUND ( 'NONE', #52654, .T. ) ;
#25726 = ADVANCED_FACE ( 'NONE', ( #30006 ), #9003, .F. ) ;
#25727 = CARTESIAN_POINT ( 'NONE',  ( -16.89925026227929195, -0.1191753592594197858, 13.49466922669627422 ) ) ;
#25728 = AXIS2_PLACEMENT_3D ( 'NONE', #16739, #7961, #32934 ) ;
#25729 = LINE ( 'NONE', #51295, #33713 ) ;
#25730 = DIRECTION ( 'NONE',  ( 0.005961354470445682716, -0.6427876096865404731, -0.7660212471507180654 ) ) ;
#25731 = EDGE_CURVE ( 'NONE', #35444, #32268, #47315, .T. ) ;
#25732 = VERTEX_POINT ( 'NONE', #51594 ) ;
#25733 = LINE ( 'NONE', #12098, #12355 ) ;
#25734 = CARTESIAN_POINT ( 'NONE',  ( -27.99845268667336384, -0.1191753592594197858, 7.657176279295684118 ) ) ;
#25735 = VECTOR ( 'NONE', #33368, 1000.000000000000227 ) ;
#25736 = PLANE ( 'NONE',  #55563 ) ;
#25737 = ORIENTED_EDGE ( 'NONE', *, *, #7978, .F. ) ;
#25738 = CARTESIAN_POINT ( 'NONE',  ( -15.40103151951671734, 0.000000000000000000, 12.95233060667165681 ) ) ;
#25739 = VECTOR ( 'NONE', #824, 1000.000000000000227 ) ;
#25740 = EDGE_CURVE ( 'NONE', #33706, #43208, #23883, .T. ) ;
#25741 = ORIENTED_EDGE ( 'NONE', *, *, #21286, .T. ) ;
#25742 = ORIENTED_EDGE ( 'NONE', *, *, #35725, .F. ) ;
#25743 = ADVANCED_FACE ( 'NONE', ( #4186 ), #25752, .F. ) ;
#25744 = VECTOR ( 'NONE', #34721, 999.9999999999998863 ) ;
#25745 = VERTEX_POINT ( 'NONE', #26054 ) ;
#25746 = ORIENTED_EDGE ( 'NONE', *, *, #30329, .T. ) ;
#25747 = VECTOR ( 'NONE', #27125, 1000.000000000000114 ) ;
#25748 = ORIENTED_EDGE ( 'NONE', *, *, #41514, .T. ) ;
#25749 = ORIENTED_EDGE ( 'NONE', *, *, #44720, .F. ) ;
#25750 = LINE ( 'NONE', #17222, #26009 ) ;
#25751 = CARTESIAN_POINT ( 'NONE',  ( -12.23851102634202448, -0.1191753592594197858, 11.68427982808754884 ) ) ;
#25752 = PLANE ( 'NONE',  #28568 ) ;
#25753 = ORIENTED_EDGE ( 'NONE', *, *, #2591, .F. ) ;
#25754 = CARTESIAN_POINT ( 'NONE',  ( -14.15020592462595062, 0.000000000000000000, 5.648957146962426457 ) ) ;
#25755 = ORIENTED_EDGE ( 'NONE', *, *, #9896, .F. ) ;
#25756 = DIRECTION ( 'NONE',  ( 0.005961354470445682716, -0.6427876096865404731, -0.7660212471507180654 ) ) ;
#25757 = EDGE_LOOP ( 'NONE', ( #10535, #52214, #30176, #25269 ) ) ;
#25758 = FACE_OUTER_BOUND ( 'NONE', #26108, .T. ) ;
#25759 = AXIS2_PLACEMENT_3D ( 'NONE', #4024, #21348, #8569 ) ;
#25760 = PLANE ( 'NONE',  #42806 ) ;
#25761 = DIRECTION ( 'NONE',  ( -0.5449076811759708816, 0.6444004775717707689, 0.5364919789714475140 ) ) ;
#25762 = EDGE_LOOP ( 'NONE', ( #36495, #41237, #35616, #24459 ) ) ;
#25763 = PLANE ( 'NONE',  #27411 ) ;
#25764 = VECTOR ( 'NONE', #19960, 999.9999999999998863 ) ;
#25765 = ORIENTED_EDGE ( 'NONE', *, *, #49458, .F. ) ;
#25766 = CARTESIAN_POINT ( 'NONE',  ( -18.34187781110085069, 0.000000000000000000, 6.893658810118608038 ) ) ;
#25767 = EDGE_CURVE ( 'NONE', #17866, #8893, #43367, .T. ) ;
#25769 = AXIS2_PLACEMENT_3D ( 'NONE', #49296, #43909, #36510 ) ;
#25768 = DIRECTION ( 'NONE',  ( -0.005002170337468016433, -0.7660444431189770143, 0.6427681459581293666 ) ) ;
#25770 = FACE_OUTER_BOUND ( 'NONE', #2065, .T. ) ;
#25771 = DIRECTION ( 'NONE',  ( 0.000000000000000000, -0.000000000000000000, -1.000000000000000000 ) ) ;
#25772 = FACE_OUTER_BOUND ( 'NONE', #14791, .T. ) ;
#25773 = FACE_OUTER_BOUND ( 'NONE', #34775, .T. ) ;
#25774 = FACE_OUTER_BOUND ( 'NONE', #10460, .T. ) ;
#25775 = AXIS2_PLACEMENT_3D ( 'NONE', #2034, #19089, #15658 ) ;
#25776 = CARTESIAN_POINT ( 'NONE',  ( -67.14101802347384762, -8.387388012353506284, -2.442027903730112026 ) ) ;
#25777 = ORIENTED_EDGE ( 'NONE', *, *, #9049, .F. ) ;
#25778 = CARTESIAN_POINT ( 'NONE',  ( -16.27471411925786882, 0.000000000000000000, 5.801749746533357843 ) ) ;
#25779 = EDGE_LOOP ( 'NONE', ( #40008, #4117, #26479, #41478, #39027 ) ) ;
#25780 = EDGE_CURVE ( 'NONE', #51442, #47161, #161, .T. ) ;
#25781 = ADVANCED_FACE ( 'NONE', ( #33006 ), #31702, .F. ) ;
#25782 = VECTOR ( 'NONE', #43991, 999.9999999999998863 ) ;
#25783 = FACE_OUTER_BOUND ( 'NONE', #1907, .T. ) ;
#25784 = LINE ( 'NONE', #35421, #26928 ) ;
#25785 = FACE_OUTER_BOUND ( 'NONE', #39082, .T. ) ;
#25786 = CARTESIAN_POINT ( 'NONE',  ( -12.23851102634202448, -0.1191753592594197858, 11.68427982808754884 ) ) ;
#25787 = CARTESIAN_POINT ( 'NONE',  ( -16.81267852042391198, -0.1191753592594197858, 3.312241722634738039 ) ) ;
#25788 = EDGE_CURVE ( 'NONE', #3308, #32995, #14647, .T. ) ;
#25789 = DIRECTION ( 'NONE',  ( 0.000000000000000000, -0.000000000000000000, -1.000000000000000000 ) ) ;
#25790 = AXIS2_PLACEMENT_3D ( 'NONE', #11814, #42749, #38503 ) ;
#25791 = DIRECTION ( 'NONE',  ( 0.007781995580012663651, 0.000000000000000000, -0.9999697198139515519 ) ) ;
#25792 = VECTOR ( 'NONE', #26279, 1000.000000000000227 ) ;
#25793 = APPLICATION_PROTOCOL_DEFINITION ( 'draft international standard', 'automotive_design', 1998, #5743 ) ;
#25794 = ORIENTED_EDGE ( 'NONE', *, *, #31764, .T. ) ;
#25795 = CARTESIAN_POINT ( 'NONE',  ( -28.01304021813471934, 14.75288872755216119, 4.717228875401151988 ) ) ;
#25796 = DIRECTION ( 'NONE',  ( -0.5364919789714478471, 0.6444004775717705469, -0.5449076811759709926 ) ) ;
#25797 = DIRECTION ( 'NONE',  ( 0.6427681459581294776, -0.7660444431189769032, 0.005002170337467562802 ) ) ;
#25798 = CARTESIAN_POINT ( 'NONE',  ( -18.42254072940788134, 0.1245042932765029059, 3.833899844102495624 ) ) ;
#25799 = ADVANCED_FACE ( 'NONE', ( #11708 ), #10108, .F. ) ;
#25800 = LINE ( 'NONE', #43127, #18524 ) ;
#25801 = DIRECTION ( 'NONE',  ( 0.000000000000000000, -0.000000000000000000, -1.000000000000000000 ) ) ;
#25802 = DIRECTION ( 'NONE',  ( 0.9999697198139515519, 0.000000000000000000, 0.007781995580013368816 ) ) ;
#25803 = ORIENTED_EDGE ( 'NONE', *, *, #9910, .T. ) ;
#25804 = EDGE_CURVE ( 'NONE', #39023, #20767, #10400, .T. ) ;
#25805 = VECTOR ( 'NONE', #1982, 1000.000000000000227 ) ;
#25806 = DIRECTION ( 'NONE',  ( -0.005961354470445682716, -0.6427876096865404731, 0.7660212471507180654 ) ) ;
#25807 = FACE_OUTER_BOUND ( 'NONE', #9228, .T. ) ;
#25808 = VERTEX_POINT ( 'NONE', #15978 ) ;
#25809 = VECTOR ( 'NONE', #21058, 999.9999999999998863 ) ;
#25810 = ADVANCED_FACE ( 'NONE', ( #36501 ), #53820, .F. ) ;
#25811 = EDGE_LOOP ( 'NONE', ( #12426, #36420, #54386, #51243 ) ) ;
#25812 = LINE ( 'NONE', #13849, #49201 ) ;
#25813 = VECTOR ( 'NONE', #54516, 1000.000000000000227 ) ;
#25814 = ADVANCED_FACE ( 'NONE', ( #29024 ), #50324, .F. ) ;
#25815 = ORIENTED_EDGE ( 'NONE', *, *, #30628, .T. ) ;
#25816 = ORIENTED_EDGE ( 'NONE', *, *, #48870, .F. ) ;
#25817 = VERTEX_POINT ( 'NONE', #48749 ) ;
#25818 = VECTOR ( 'NONE', #34861, 1000.000000000000227 ) ;
#25819 = ORIENTED_EDGE ( 'NONE', *, *, #2104, .F. ) ;
#25820 = CARTESIAN_POINT ( 'NONE',  ( -13.07066190154808361, 0.000000000000000000, 12.04713590736729678 ) ) ;
#25821 = VECTOR ( 'NONE', #10995, 999.9999999999998863 ) ;
#25822 = ORIENTED_EDGE ( 'NONE', *, *, #3561, .F. ) ;
#25823 = CARTESIAN_POINT ( 'NONE',  ( -13.66389425413188086, 0.000000000000000000, 2.867411191963296080 ) ) ;
#25824 = LINE ( 'NONE', #30903, #45742 ) ;
#25825 = VECTOR ( 'NONE', #3209, 999.9999999999998863 ) ;
#25826 = ORIENTED_EDGE ( 'NONE', *, *, #6616, .T. ) ;
#25827 = ORIENTED_EDGE ( 'NONE', *, *, #42096, .F. ) ;
#25828 = VECTOR ( 'NONE', #31872, 999.9999999999998863 ) ;
#25829 = AXIS2_PLACEMENT_3D ( 'NONE', #12171, #7344, #37756 ) ;
#25830 = CARTESIAN_POINT ( 'NONE',  ( -17.36532418587302473, -0.1191753592594177458, 13.67570816655714516 ) ) ;
#25831 = VERTEX_POINT ( 'NONE', #11441 ) ;
#25832 = CARTESIAN_POINT ( 'NONE',  ( -11.87243407472968926, 0.000000000000000000, 11.50246268866867361 ) ) ;
#25833 = ORIENTED_EDGE ( 'NONE', *, *, #12242, .T. ) ;
#25834 = DIRECTION ( 'NONE',  ( 0.6427681459581294776, -0.7660444431189769032, 0.005002170337467562802 ) ) ;
#25835 = EDGE_CURVE ( 'NONE', #4032, #8206, #23185, .T. ) ;
#25836 = EDGE_LOOP ( 'NONE', ( #5065, #26382, #30533, #4255 ) ) ;
#25837 = DIRECTION ( 'NONE',  ( 0.007781995580012662783, 0.000000000000000000, -0.9999697198139514409 ) ) ;
#25838 = EDGE_CURVE ( 'NONE', #83, #27011, #46068, .T. ) ;
#25839 = AXIS2_PLACEMENT_3D ( 'NONE', #37165, #41691, #6792 ) ;
#25840 = CARTESIAN_POINT ( 'NONE',  ( -16.50360637555614218, -4.727446477803164626, 3.141052004737669545 ) ) ;
#25841 = VERTEX_POINT ( 'NONE', #2879 ) ;
#25842 = PLANE ( 'NONE',  #48502 ) ;
#25843 = DIRECTION ( 'NONE',  ( 0.7660212471507180654, -0.6427876096865404731, 0.005961354470445141482 ) ) ;
#25845 = VECTOR ( 'NONE', #9852, 1000.000000000000227 ) ;
#25844 = DIRECTION ( 'NONE',  ( 0.5364919789714477361, 0.6444004775717706579, 0.5449076811759711036 ) ) ;
#25846 = DIRECTION ( 'NONE',  ( -0.9999697198139514409, -0.000000000000000000, -0.007781995580013368816 ) ) ;
#25847 = ORIENTED_EDGE ( 'NONE', *, *, #28402, .T. ) ;
#25848 = VECTOR ( 'NONE', #40857, 999.9999999999998863 ) ;
#25849 = ADVANCED_FACE ( 'NONE', ( #1600 ), #20210, .F. ) ;
#25850 = EDGE_CURVE ( 'NONE', #53959, #30417, #36241, .T. ) ;
#25851 = EDGE_CURVE ( 'NONE', #24469, #35938, #22619, .T. ) ;
#25852 = FACE_OUTER_BOUND ( 'NONE', #1250, .T. ) ;
#25853 = CARTESIAN_POINT ( 'NONE',  ( -19.60912206198628027, -0.1191753592594197858, 4.398475361799976113 ) ) ;
#25854 = CARTESIAN_POINT ( 'NONE',  ( -22.40634380310664397, 0.000000000000000000, 5.584705972946605534 ) ) ;
#25855 = CARTESIAN_POINT ( 'NONE',  ( 2.072287782118878319, 0.000000000000000000, -2.950529333540147015 ) ) ;
#25856 = AXIS2_PLACEMENT_3D ( 'NONE', #13606, #26971, #52512 ) ;
#25857 = DIRECTION ( 'NONE',  ( -0.7660212471507179544, -0.6427876096865405842, -0.005961354470445141482 ) ) ;
#25858 = EDGE_CURVE ( 'NONE', #47896, #43283, #44461, .T. ) ;
#25859 = DIRECTION ( 'NONE',  ( -0.6427681459581293666, -0.7660444431189770143, -0.005002170337467561935 ) ) ;
#25860 = DIRECTION ( 'NONE',  ( -0.5364919789714478471, 0.6444004775717705469, -0.5449076811759709926 ) ) ;
#25862 = AXIS2_PLACEMENT_3D ( 'NONE', #9029, #52468, #504 ) ;
#25861 = DIRECTION ( 'NONE',  ( 0.005961354470445682716, -0.6427876096865404731, -0.7660212471507180654 ) ) ;
#25863 = CARTESIAN_POINT ( 'NONE',  ( -8.409922665610809034, 0.000000000000000000, 10.23674650875856962 ) ) ;
#25864 = EDGE_LOOP ( 'NONE', ( #37689, #34969, #8889, #2797 ) ) ;
#25865 =( NAMED_UNIT ( * ) PLANE_ANGLE_UNIT ( ) SI_UNIT ( $, .RADIAN. ) );
#25867 = LINE ( 'NONE', #4296, #17836 ) ;
#25866 = VECTOR ( 'NONE', #30944, 1000.000000000000114 ) ;
#25868 = ORIENTED_EDGE ( 'NONE', *, *, #25478, .F. ) ;
#25869 = CARTESIAN_POINT ( 'NONE',  ( -11.43033398677498091, -0.3560938001956562293, 1.706272219544479718 ) ) ;
#25870 = LINE ( 'NONE', #30695, #35482 ) ;
#25871 = VECTOR ( 'NONE', #9734, 1000.000000000000000 ) ;
#25872 = CARTESIAN_POINT ( 'NONE',  ( -17.74560456716937296, 0.000000000000000000, 3.774316574337878372 ) ) ;
#25873 = FACE_OUTER_BOUND ( 'NONE', #12347, .T. ) ;
#25874 = EDGE_CURVE ( 'NONE', #12052, #23249, #35676, .T. ) ;
#25875 = CARTESIAN_POINT ( 'NONE',  ( -26.13337879274045505, 0.000000000000000000, 6.833023547870798353 ) ) ;
#25876 = EDGE_LOOP ( 'NONE', ( #15664, #45368, #17087, #22137 ) ) ;
#25877 = AXIS2_PLACEMENT_3D ( 'NONE', #52813, #9107, #52284 ) ;
#25878 = EDGE_CURVE ( 'NONE', #53765, #51817, #45051, .T. ) ;
#25879 = AXIS2_PLACEMENT_3D ( 'NONE', #11539, #20312, #20621 ) ;
#25880 = ORIENTED_EDGE ( 'NONE', *, *, #3393, .F. ) ;
#25881 = EDGE_CURVE ( 'NONE', #33602, #19374, #1298, .T. ) ;
#25882 = PLANE ( 'NONE',  #44981 ) ;
#25883 = CARTESIAN_POINT ( 'NONE',  ( -14.17572954220636205, -0.8417996532631565332, 3.569803139150924398 ) ) ;
#25884 = VERTEX_POINT ( 'NONE', #22883 ) ;
#25885 = DIRECTION ( 'NONE',  ( 0.000000000000000000, -0.000000000000000000, -1.000000000000000000 ) ) ;
#25886 = EDGE_CURVE ( 'NONE', #53080, #44261, #40207, .T. ) ;
#25887 = EDGE_LOOP ( 'NONE', ( #13546, #8478, #54955, #13110 ) ) ;
#25888 = PLANE ( 'NONE',  #14082 ) ;
#25889 = ORIENTED_EDGE ( 'NONE', *, *, #16958, .T. ) ;
#25890 = CARTESIAN_POINT ( 'NONE',  ( -17.74482636761137044, -0.1191753592594197858, 3.674319602356483916 ) ) ;
#25891 = EDGE_CURVE ( 'NONE', #34091, #17338, #37845, .T. ) ;
#25892 = AXIS2_PLACEMENT_3D ( 'NONE', #49815, #41006, #10913 ) ;
#25893 = ORIENTED_EDGE ( 'NONE', *, *, #14445, .F. ) ;
#25894 = VERTEX_POINT ( 'NONE', #12561 ) ;
#25895 = ORIENTED_EDGE ( 'NONE', *, *, #5132, .T. ) ;
#25896 = VECTOR ( 'NONE', #34122, 999.9999999999998863 ) ;
#25897 = DIRECTION ( 'NONE',  ( -0.8531650599175529814, -0.4028455766673920135, 0.3313982828793697877 ) ) ;
#25898 = PLANE ( 'NONE',  #26896 ) ;
#25899 = VECTOR ( 'NONE', #2151, 1000.000000000000000 ) ;
#25900 = CARTESIAN_POINT ( 'NONE',  ( -12.13851405436063047, 0.000000000000000000, 11.68505802764555135 ) ) ;
#25901 = LINE ( 'NONE', #33838, #42985 ) ;
#25902 = ORIENTED_EDGE ( 'NONE', *, *, #35397, .T. ) ;
#25903 = VECTOR ( 'NONE', #36893, 999.9999999999998863 ) ;
#25904 = ORIENTED_EDGE ( 'NONE', *, *, #11679, .T. ) ;
#25905 = VERTEX_POINT ( 'NONE', #51465 ) ;
#25906 = VECTOR ( 'NONE', #11073, 1000.000000000000000 ) ;
#25907 = AXIS2_PLACEMENT_3D ( 'NONE', #31895, #30014, #10038 ) ;
#25908 = DIRECTION ( 'NONE',  ( -0.9999697198139514409, -0.000000000000000000, -0.007781995580013368816 ) ) ;
#25909 = EDGE_LOOP ( 'NONE', ( #44631, #12897, #31130, #44108 ) ) ;
#25910 = FACE_OUTER_BOUND ( 'NONE', #30235, .T. ) ;
#25911 = EDGE_LOOP ( 'NONE', ( #37581, #35067, #6965, #7526 ) ) ;
#25912 = DIRECTION ( 'NONE',  ( 0.6427681459581294776, -0.7660444431189769032, 0.005002170337467562802 ) ) ;
#25913 = DIRECTION ( 'NONE',  ( 0.000000000000000000, -1.000000000000000000, 0.000000000000000000 ) ) ;
#25914 = AXIS2_PLACEMENT_3D ( 'NONE', #22647, #48785, #35713 ) ;
#25915 = EDGE_LOOP ( 'NONE', ( #32762, #40571, #4665, #39083 ) ) ;
#25916 = VECTOR ( 'NONE', #8150, 1000.000000000000114 ) ;
#25917 = DIRECTION ( 'NONE',  ( 0.007781995580012662783, 0.000000000000000000, -0.9999697198139514409 ) ) ;
#25918 = VECTOR ( 'NONE', #51059, 999.9999999999998863 ) ;
#25919 = EDGE_LOOP ( 'NONE', ( #35364, #53875, #46565, #50170 ) ) ;
#25920 = AXIS2_PLACEMENT_3D ( 'NONE', #23988, #19737, #53529 ) ;
#25921 = CARTESIAN_POINT ( 'NONE',  ( -9.808144436391993182, 0.000000000000000000, 10.77986332834118777 ) ) ;
#25922 = AXIS2_PLACEMENT_3D ( 'NONE', #23609, #18221, #1479 ) ;
#25923 = ORIENTED_EDGE ( 'NONE', *, *, #11979, .F. ) ;
#25924 = CARTESIAN_POINT ( 'NONE',  ( -20.54049170961573267, 0.000000000000000000, 4.660556269540326646 ) ) ;
#25925 = CARTESIAN_POINT ( 'NONE',  ( -15.07504926568683423, 0.000000000000000000, 5.072421676205853380 ) ) ;
#25926 = CARTESIAN_POINT ( 'NONE',  ( -16.79925329029790149, 0.000000000000000000, 13.49544742625427496 ) ) ;
#25927 = ORIENTED_EDGE ( 'NONE', *, *, #52591, .T. ) ;
#25928 = EDGE_CURVE ( 'NONE', #49012, #17790, #51163, .T. ) ;
#25929 = CARTESIAN_POINT ( 'NONE',  ( -26.13415699229845757, -0.1191753592594197858, 6.933020519852192365 ) ) ;
#25930 = CARTESIAN_POINT ( 'NONE',  ( -27.06552663992790997, 0.000000000000000000, 7.195101427592543786 ) ) ;
#25931 = FACE_OUTER_BOUND ( 'NONE', #53419, .T. ) ;
#25932 = LINE ( 'NONE', #17118, #27731 ) ;
#25933 = EDGE_CURVE ( 'NONE', #55170, #47218, #42637, .T. ) ;
#25934 = LINE ( 'NONE', #35018, #31247 ) ;
#25935 = DIRECTION ( 'NONE',  ( 0.000000000000000000, -1.000000000000000000, 0.000000000000000000 ) ) ;
#25936 = AXIS2_PLACEMENT_3D ( 'NONE', #34392, #30421, #51973 ) ;
#25937 = FACE_OUTER_BOUND ( 'NONE', #55842, .T. ) ;
#25938 = VERTEX_POINT ( 'NONE', #8283 ) ;
#25939 = DIRECTION ( 'NONE',  ( 0.000000000000000000, -0.000000000000000000, -1.000000000000000000 ) ) ;
#25940 = VECTOR ( 'NONE', #33222, 1000.000000000000227 ) ;
#25941 = CARTESIAN_POINT ( 'NONE',  ( -21.93567689722629765, 19.99370688441071309, 4.657440554554202805 ) ) ;
#25942 = CARTESIAN_POINT ( 'NONE',  ( -21.37767238905108513, -3.270328918600657886, 10.35291257913092977 ) ) ;
#25943 = ORIENTED_EDGE ( 'NONE', *, *, #36885, .T. ) ;
#25944 = CARTESIAN_POINT ( 'NONE',  ( -27.13182931993292257, 16.99370688441070953, -4.657437592157546824 ) ) ;
#25945 = CARTESIAN_POINT ( 'NONE',  ( -18.19747506107908563, 0.000000000000000000, 14.03856424583689311 ) ) ;
#25946 = VECTOR ( 'NONE', #54591, 999.9999999999998863 ) ;
#25947 = ORIENTED_EDGE ( 'NONE', *, *, #41429, .T. ) ;
#25948 = DIRECTION ( 'NONE',  ( 0.6427681459581294776, -0.7660444431189769032, 0.005002170337467562802 ) ) ;
#25949 = AXIS2_PLACEMENT_3D ( 'NONE', #36673, #2832, #45449 ) ;
#25950 = DIRECTION ( 'NONE',  ( 0.5364919789714477361, 0.6444004775717706579, 0.5449076811759711036 ) ) ;
#25951 = CARTESIAN_POINT ( 'NONE',  ( -65.40680149495634055, 2.000000000000022204, -1.598589950280139727 ) ) ;
#25952 = ORIENTED_EDGE ( 'NONE', *, *, #8217, .T. ) ;
#25953 = AXIS2_PLACEMENT_3D ( 'NONE', #41955, #12464, #20092 ) ;
#25954 = VECTOR ( 'NONE', #26818, 1000.000000000000227 ) ;
#25955 = ORIENTED_EDGE ( 'NONE', *, *, #20818, .T. ) ;
#25956 = CARTESIAN_POINT ( 'NONE',  ( -67.79130742519731712, -0.6009124436974506711, 4.273291358077424107 ) ) ;
#25957 = CARTESIAN_POINT ( 'NONE',  ( -20.79160881769003666, -2.622721114510659479, 4.873809532974441971 ) ) ;
#25958 = CARTESIAN_POINT ( 'NONE',  ( -11.88054826722768276, 25.79903810567671130, 3.000000000000000888 ) ) ;
#25959 = VECTOR ( 'NONE', #13763, 1000.000000000000227 ) ;
#25960 = DIRECTION ( 'NONE',  ( 0.005002170337468016433, -0.7660444431189770143, -0.6427681459581293666 ) ) ;
#25962 = LINE ( 'NONE', #39002, #33750 ) ;
#25961 = VECTOR ( 'NONE', #26901, 1000.000000000000227 ) ;
#25963 = DIRECTION ( 'NONE',  ( 0.000000000000000000, -1.000000000000000000, 0.000000000000000000 ) ) ;
#25964 = ORIENTED_EDGE ( 'NONE', *, *, #19561, .T. ) ;
#25965 = LINE ( 'NONE', #55467, #51001 ) ;
#25966 = EDGE_CURVE ( 'NONE', #21242, #47865, #16512, .T. ) ;
#25967 = VECTOR ( 'NONE', #11697, 999.9999999999998863 ) ;
#25968 = VECTOR ( 'NONE', #33958, 1000.000000000000227 ) ;
#25969 = CARTESIAN_POINT ( 'NONE',  ( -17.67724697029697367, 0.000000000000000000, 6.898831121002622524 ) ) ;
#25970 = ORIENTED_EDGE ( 'NONE', *, *, #18873, .T. ) ;
#25971 = ADVANCED_FACE ( 'NONE', ( #3182 ), #42379, .F. ) ;
#25972 = DIRECTION ( 'NONE',  ( -0.005961354470445682716, -0.6427876096865404731, 0.7660212471507180654 ) ) ;
#25973 = LINE ( 'NONE', #29080, #1422 ) ;
#25974 = FACE_OUTER_BOUND ( 'NONE', #4711, .T. ) ;
#25975 = ORIENTED_EDGE ( 'NONE', *, *, #5406, .F. ) ;
#25976 = FACE_OUTER_BOUND ( 'NONE', #34737, .T. ) ;
#25977 = EDGE_CURVE ( 'NONE', #54798, #7497, #25596, .T. ) ;
#25978 = ORIENTED_EDGE ( 'NONE', *, *, #15289, .T. ) ;
#25979 = VECTOR ( 'NONE', #24892, 999.9999999999998863 ) ;
#25980 = EDGE_LOOP ( 'NONE', ( #16000, #12627, #52140, #38381 ) ) ;
#25981 = ORIENTED_EDGE ( 'NONE', *, *, #38789, .F. ) ;
#25982 = ORIENTED_EDGE ( 'NONE', *, *, #2687, .T. ) ;
#25983 = DIRECTION ( 'NONE',  ( 0.5364919789714477361, 0.6444004775717706579, 0.5449076811759711036 ) ) ;
#25984 = VECTOR ( 'NONE', #9088, 1000.000000000000114 ) ;
#25985 = ORIENTED_EDGE ( 'NONE', *, *, #17742, .T. ) ;
#25986 = CARTESIAN_POINT ( 'NONE',  ( -12.77353955513438599, 0.000000000000000000, 7.875663101813041855 ) ) ;
#25987 = VERTEX_POINT ( 'NONE', #34412 ) ;
#25988 = DIRECTION ( 'NONE',  ( -0.9999697198139514409, -0.000000000000000000, -0.007781995580013368816 ) ) ;
#25989 = VECTOR ( 'NONE', #36284, 1000.000000000000227 ) ;
#25990 = EDGE_LOOP ( 'NONE', ( #52988, #8147, #52486, #50031 ) ) ;
#25991 = LINE ( 'NONE', #96, #9398 ) ;
#25992 = ORIENTED_EDGE ( 'NONE', *, *, #16073, .T. ) ;
#25993 = VECTOR ( 'NONE', #44840, 999.9999999999998863 ) ;
#25994 = LINE ( 'NONE', #8666, #27499 ) ;
#25995 = CARTESIAN_POINT ( 'NONE',  ( 2.072287782118878319, 0.000000000000000000, -2.950529333540147015 ) ) ;
#25996 = LINE ( 'NONE', #9207, #22254 ) ;
#25997 = CARTESIAN_POINT ( 'NONE',  ( -19.79569077582305070, 0.000000000000000000, 14.58012466630350445 ) ) ;
#25998 = EDGE_CURVE ( 'NONE', #41698, #15410, #43236, .T. ) ;
#25999 = LINE ( 'NONE', #39315, #33764 ) ;
#26000 = ORIENTED_EDGE ( 'NONE', *, *, #518, .F. ) ;
#26001 = AXIS2_PLACEMENT_3D ( 'NONE', #20013, #7250, #38180 ) ;
#26002 = ADVANCED_FACE ( 'NONE', ( #20517 ), #4332, .F. ) ;
#26003 = EDGE_LOOP ( 'NONE', ( #33827, #28522, #25947, #16273 ) ) ;
#26004 = AXIS2_PLACEMENT_3D ( 'NONE', #51255, #8368, #12376 ) ;
#26005 = LINE ( 'NONE', #12648, #30373 ) ;
#26006 = FACE_OUTER_BOUND ( 'NONE', #12615, .T. ) ;
#26007 = EDGE_CURVE ( 'NONE', #44683, #46842, #11965, .T. ) ;
#26008 = ADVANCED_FACE ( 'NONE', ( #25333 ), #17098, .F. ) ;
#26009 = VECTOR ( 'NONE', #9000, 1000.000000000000227 ) ;
#26010 = CARTESIAN_POINT ( 'NONE',  ( -31.72626587586518099, 0.000000000000000000, 9.005490826201270949 ) ) ;
#26011 = AXIS2_PLACEMENT_3D ( 'NONE', #43278, #17693, #21936 ) ;
#26012 = DIRECTION ( 'NONE',  ( 0.007781995580012663651, -3.146120232559066537E-19, -0.9999697198139514409 ) ) ;
#26013 = CARTESIAN_POINT ( 'NONE',  ( -9.808144436391993182, 0.000000000000000000, 10.77986332834118777 ) ) ;
#26014 = DIRECTION ( 'NONE',  ( 0.5449076811759707706, 0.6444004775717708799, -0.5364919789714476250 ) ) ;
#26015 = ORIENTED_EDGE ( 'NONE', *, *, #37193, .F. ) ;
#26016 = DIRECTION ( 'NONE',  ( 0.007781995580012662783, 0.000000000000000000, -0.9999697198139514409 ) ) ;
#26017 = FACE_OUTER_BOUND ( 'NONE', #6813, .T. ) ;
#26018 = ORIENTED_EDGE ( 'NONE', *, *, #9197, .T. ) ;
#26019 = PLANE ( 'NONE',  #56066 ) ;
#26020 = DIRECTION ( 'NONE',  ( 0.000000000000000000, -1.000000000000000000, 0.000000000000000000 ) ) ;
#26021 = CARTESIAN_POINT ( 'NONE',  ( -23.23471500290295921, 19.24370688441070953, 4.480778704491060971 ) ) ;
#26022 = DIRECTION ( 'NONE',  ( 0.9999697198139515519, 0.000000000000000000, 0.007781995580013368816 ) ) ;
#26023 = AXIS2_PLACEMENT_3D ( 'NONE', #3979, #4286, #16762 ) ;
#26024 = ADVANCED_FACE ( 'NONE', ( #38384 ), #29305, .F. ) ;
#26025 = ORIENTED_EDGE ( 'NONE', *, *, #49948, .F. ) ;
#26026 = ORIENTED_EDGE ( 'NONE', *, *, #6200, .F. ) ;
#26027 = CARTESIAN_POINT ( 'NONE',  ( -31.72704407542318350, -0.1191753592594197858, 9.105487798182664960 ) ) ;
#26028 = LINE ( 'NONE', #31404, #12256 ) ;
#26029 = DIRECTION ( 'NONE',  ( 0.9999697198139515519, 0.000000000000000000, 0.007781995580013368816 ) ) ;
#26030 = DIRECTION ( 'NONE',  ( 0.005961354470445682716, -0.6427876096865404731, -0.7660212471507180654 ) ) ;
#26031 = AXIS2_PLACEMENT_3D ( 'NONE', #15730, #46381, #11500 ) ;
#26032 = DIRECTION ( 'NONE',  ( 0.7660212471507180654, -0.6427876096865404731, 0.005961354470445141482 ) ) ;
#26033 = CARTESIAN_POINT ( 'NONE',  ( -19.14237710917700142, -3.432230869623161595, 4.207364329806451586 ) ) ;
#26034 = CARTESIAN_POINT ( 'NONE',  ( -23.33693525117809386, 0.000000000000000000, 5.746789908705562944 ) ) ;
#26035 = ORIENTED_EDGE ( 'NONE', *, *, #2032, .F. ) ;
#26037 = VECTOR ( 'NONE', #22996, 1000.000000000000227 ) ;
#26036 = FACE_OUTER_BOUND ( 'NONE', #37117, .T. ) ;
#26038 = CARTESIAN_POINT ( 'NONE',  ( -15.00929495654107448, 2.714935509636508204, 2.425430953408422408 ) ) ;
#26039 = ORIENTED_EDGE ( 'NONE', *, *, #3306, .T. ) ;
#26040 = DIRECTION ( 'NONE',  ( 0.000000000000000000, -1.000000000000000000, 0.000000000000000000 ) ) ;
#26041 = ORIENTED_EDGE ( 'NONE', *, *, #18334, .T. ) ;
#26042 = CARTESIAN_POINT ( 'NONE',  ( -18.66354898467281132, 0.000000000000000000, 14.21960318569776582 ) ) ;
#26043 = ORIENTED_EDGE ( 'NONE', *, *, #42389, .F. ) ;
#26044 = AXIS2_PLACEMENT_3D ( 'NONE', #2897, #37862, #30921 ) ;
#26045 = EDGE_CURVE ( 'NONE', #39606, #24516, #46619, .T. ) ;
#26046 = VERTEX_POINT ( 'NONE', #3470 ) ;
#26047 = ORIENTED_EDGE ( 'NONE', *, *, #19061, .F. ) ;
#26048 = VECTOR ( 'NONE', #32152, 1000.000000000000227 ) ;
#26049 = VERTEX_POINT ( 'NONE', #38956 ) ;
#26050 = ORIENTED_EDGE ( 'NONE', *, *, #2101, .F. ) ;
#26051 = VERTEX_POINT ( 'NONE', #34677 ) ;
#26052 = DIRECTION ( 'NONE',  ( 0.000000000000000000, -0.000000000000000000, -1.000000000000000000 ) ) ;
#26053 = PLANE ( 'NONE',  #55574 ) ;
#26054 = CARTESIAN_POINT ( 'NONE',  ( -10.87032476607480547, 0.000000000000000000, 2.150487256055822805 ) ) ;
#26055 = EDGE_CURVE ( 'NONE', #21341, #1854, #52002, .T. ) ;
#26056 = VERTEX_POINT ( 'NONE', #13113 ) ;
#26057 = DIRECTION ( 'NONE',  ( 0.000000000000000000, -1.000000000000000000, 0.000000000000000000 ) ) ;
#26058 = ORIENTED_EDGE ( 'NONE', *, *, #50328, .F. ) ;
#26059 = EDGE_CURVE ( 'NONE', #38090, #54919, #16241, .T. ) ;
#26060 = ORIENTED_EDGE ( 'NONE', *, *, #5423, .T. ) ;
#26061 = EDGE_CURVE ( 'NONE', #47842, #31761, #38100, .T. ) ;
#26062 = DIRECTION ( 'NONE',  ( -0.7660212471507179544, -0.6427876096865405842, -0.005961354470445141482 ) ) ;
#26063 = LINE ( 'NONE', #43374, #25059 ) ;
#26064 = EDGE_CURVE ( 'NONE', #29013, #52907, #12275, .T. ) ;
#26065 = ORIENTED_EDGE ( 'NONE', *, *, #48019, .T. ) ;
#26066 = LINE ( 'NONE', #51866, #42802 ) ;
#26067 = EDGE_LOOP ( 'NONE', ( #11514, #23647, #34146, #34402 ) ) ;
#26068 = DIRECTION ( 'NONE',  ( -0.6427681459581293666, -0.7660444431189770143, -0.005002170337467561935 ) ) ;
#26069 = EDGE_CURVE ( 'NONE', #36809, #27546, #14254, .T. ) ;
#26070 = DIRECTION ( 'NONE',  ( 0.007781995580012663651, 0.000000000000000000, -0.9999697198139515519 ) ) ;
#26071 = EDGE_CURVE ( 'NONE', #49012, #17246, #35265, .T. ) ;
#26072 = LINE ( 'NONE', #21528, #22397 ) ;
#26073 = VECTOR ( 'NONE', #981, 1000.000000000000227 ) ;
#26074 = DIRECTION ( 'NONE',  ( 0.007781995580012662783, 0.000000000000000000, -0.9999697198139514409 ) ) ;
#26075 = CARTESIAN_POINT ( 'NONE',  ( -25.20278734466900517, 0.000000000000000000, 6.670939612111840944 ) ) ;
#26076 = CARTESIAN_POINT ( 'NONE',  ( -11.17708129266966743, 0.000000000000000000, 7.559931525015129772 ) ) ;
#26077 = LINE ( 'NONE', #44230, #50235 ) ;
#26078 = DIRECTION ( 'NONE',  ( 0.007781995580012663651, 0.000000000000000000, -0.9999697198139515519 ) ) ;
#26079 = ORIENTED_EDGE ( 'NONE', *, *, #40433, .T. ) ;
#26080 = CARTESIAN_POINT ( 'NONE',  ( -56.26447305843585411, 6.756484714774108724, -2.135113782577493513 ) ) ;
#26081 = APPLICATION_CONTEXT ( 'automotive_design' ) ;
#26082 = EDGE_CURVE ( 'NONE', #10688, #4495, #13942, .T. ) ;
#26083 = VECTOR ( 'NONE', #29402, 999.9999999999998863 ) ;
#26084 = CARTESIAN_POINT ( 'NONE',  ( -10.28842178966973897, 0.000000000000000000, 0.8776935365639153552 ) ) ;
#26085 = FACE_OUTER_BOUND ( 'NONE', #40831, .T. ) ;
#26086 = CARTESIAN_POINT ( 'NONE',  ( -19.80914291367107438, 1.743523803501506819, 7.437284542042184476 ) ) ;
#26087 = CARTESIAN_POINT ( 'NONE',  ( -28.37605857990474334, 14.54329997866345714, -4.729543700631310799 ) ) ;
#26088 = CARTESIAN_POINT ( 'NONE',  ( -15.45196360412565895, -0.1191753592594177180, 6.646819749008290756 ) ) ;
#26089 = PLANE ( 'NONE',  #13234 ) ;
#26090 = EDGE_CURVE ( 'NONE', #54495, #38297, #44590, .T. ) ;
#26091 = CARTESIAN_POINT ( 'NONE',  ( -14.00280974873554030, 0.000000000000000000, 12.40921378708904044 ) ) ;
#26092 = VERTEX_POINT ( 'NONE', #44328 ) ;
#26093 = CARTESIAN_POINT ( 'NONE',  ( 2.072287782118878319, 0.000000000000000000, -2.950529333540147015 ) ) ;
#26094 = PLANE ( 'NONE',  #52142 ) ;
#26095 = DIRECTION ( 'NONE',  ( -0.9999697198139514409, -0.000000000000000000, -0.007781995580013368816 ) ) ;
#26096 = DIRECTION ( 'NONE',  ( -0.9999697198139514409, -0.000000000000000000, -0.007781995580013368816 ) ) ;
#26097 = DIRECTION ( 'NONE',  ( -0.7660212471507179544, -0.6427876096865405842, -0.005961354470445141482 ) ) ;
#26098 = LINE ( 'NONE', #16712, #532 ) ;
#26099 = LINE ( 'NONE', #21556, #5672 ) ;
#26100 = CARTESIAN_POINT ( 'NONE',  ( -15.60102546347950536, 0.000000000000000000, 12.95077420755565356 ) ) ;
#26101 = CARTESIAN_POINT ( 'NONE',  ( -66.84292213857837339, -9.493652800274178460, 1.352000712394443305 ) ) ;
#26102 = ORIENTED_EDGE ( 'NONE', *, *, #45867, .T. ) ;
#26103 = LINE ( 'NONE', #43409, #16524 ) ;
#26104 = ORIENTED_EDGE ( 'NONE', *, *, #52371, .T. ) ;
#26105 = EDGE_CURVE ( 'NONE', #45704, #3681, #9970, .T. ) ;
#26106 = AXIS2_PLACEMENT_3D ( 'NONE', #47815, #46967, #22241 ) ;
#26107 = EDGE_LOOP ( 'NONE', ( #11841, #8885, #11145 ) ) ;
#26108 = EDGE_LOOP ( 'NONE', ( #41535, #37072, #7182, #23591 ) ) ;
#26109 = ORIENTED_EDGE ( 'NONE', *, *, #1552, .T. ) ;
#26110 = ORIENTED_EDGE ( 'NONE', *, *, #45445, .T. ) ;
#26111 = CARTESIAN_POINT ( 'NONE',  ( -17.61711527485669038, 1.905425754524005200, 6.851535249505179337 ) ) ;
#26112 = CARTESIAN_POINT ( 'NONE',  ( -15.40103151951671734, 0.000000000000000000, 12.95233060667165681 ) ) ;
#26113 = VECTOR ( 'NONE', #338, 999.9999999999998863 ) ;
#26114 = ORIENTED_EDGE ( 'NONE', *, *, #17643, .F. ) ;
#26115 = ADVANCED_FACE ( 'NONE', ( #13656 ), #39797, .F. ) ;
#26116 = CARTESIAN_POINT ( 'NONE',  ( -67.13288019662928718, 3.903127820947823062E-15, -6.325180979151116212 ) ) ;
#26117 = VERTEX_POINT ( 'NONE', #875 ) ;
#26118 = DIRECTION ( 'NONE',  ( -0.5364919789714478471, 0.6444004775717705469, -0.5449076811759709926 ) ) ;
#26119 = DIRECTION ( 'NONE',  ( 0.007781995580012663651, -3.146120232559066537E-19, -0.9999697198139514409 ) ) ;
#26120 = VERTEX_POINT ( 'NONE', #9404 ) ;
#26121 = DIRECTION ( 'NONE',  ( 0.000000000000000000, -0.000000000000000000, -1.000000000000000000 ) ) ;
#26122 = EDGE_LOOP ( 'NONE', ( #43174, #4400, #29215, #31564 ) ) ;
#26123 = CARTESIAN_POINT ( 'NONE',  ( -16.66604408758459144, 0.000000000000000000, 9.692031080521234188 ) ) ;
#26124 = EDGE_CURVE ( 'NONE', #23769, #25116, #31266, .T. ) ;
#26125 = EDGE_CURVE ( 'NONE', #22884, #51007, #39527, .T. ) ;
#26126 = LINE ( 'NONE', #25544, #55366 ) ;
#26127 = ORIENTED_EDGE ( 'NONE', *, *, #35101, .F. ) ;
#26128 = PLANE ( 'NONE',  #53049 ) ;
#26129 = DIRECTION ( 'NONE',  ( 0.007781995580012663651, 0.000000000000000000, -0.9999697198139515519 ) ) ;
#26130 = CARTESIAN_POINT ( 'NONE',  ( -1.086233639165236964, 0.000000000000000000, -2.796443541562362078 ) ) ;
#26131 = LINE ( 'NONE', #47977, #1115 ) ;
#26132 = ORIENTED_EDGE ( 'NONE', *, *, #45705, .T. ) ;
#26133 = EDGE_CURVE ( 'NONE', #10708, #43608, #4455, .T. ) ;
#26134 = CARTESIAN_POINT ( 'NONE',  ( -70.10219403106212610, -1.000000000000000666, -7.503912900124007912 ) ) ;
#26135 = DIRECTION ( 'NONE',  ( -0.5364919789714478471, 0.6444004775717705469, -0.5449076811759709926 ) ) ;
#26136 = CARTESIAN_POINT ( 'NONE',  ( -55.17209868701984732, 6.284443032133044227, 0.3805810627426376991 ) ) ;
#26137 = DIRECTION ( 'NONE',  ( 0.007781995580012663651, 0.000000000000000000, -0.9999697198139515519 ) ) ;
#26138 = FACE_OUTER_BOUND ( 'NONE', #4011, .T. ) ;
#26139 = CARTESIAN_POINT ( 'NONE',  ( -32.47108885958310509, -1.000000000000000000, 15.83124721154520387 ) ) ;
#26140 = LINE ( 'NONE', #39178, #26149 ) ;
#26141 = EDGE_CURVE ( 'NONE', #39352, #9106, #22741, .T. ) ;
#26142 = LINE ( 'NONE', #34946, #32022 ) ;
#26143 = CARTESIAN_POINT ( 'NONE',  ( -23.33849165029409889, 0.000000000000000000, 5.946783852668351855 ) ) ;
#26144 = CARTESIAN_POINT ( 'NONE',  ( -24.27063949748155380, 0.000000000000000000, 6.308861732390097288 ) ) ;
#26145 = ORIENTED_EDGE ( 'NONE', *, *, #47235, .F. ) ;
#26146 = FACE_OUTER_BOUND ( 'NONE', #28252, .T. ) ;
#26147 = CARTESIAN_POINT ( 'NONE',  ( -8.947017916834877127, -0.1191753592594194527, 6.693699176569870346 ) ) ;
#26148 = CARTESIAN_POINT ( 'NONE',  ( -14.53131197095933125, -0.1191753592594181482, 7.761980682317608959 ) ) ;
#26149 = VECTOR ( 'NONE', #17311, 1000.000000000000114 ) ;
#26150 = DIRECTION ( 'NONE',  ( -0.7660212471507179544, -0.6427876096865405842, -0.005961354470445141482 ) ) ;
#26151 = CARTESIAN_POINT ( 'NONE',  ( -14.97870454676872320, -0.1191753592594188005, 5.542506551003013371 ) ) ;
#26152 = CARTESIAN_POINT ( 'NONE',  ( -14.13427925798353435, 0.000000000000000000, 3.602414686710813996 ) ) ;
#26153 = ORIENTED_EDGE ( 'NONE', *, *, #16493, .F. ) ;
#26154 = ORIENTED_EDGE ( 'NONE', *, *, #14012, .F. ) ;
#26155 = FACE_OUTER_BOUND ( 'NONE', #12820, .T. ) ;
#26156 = DIRECTION ( 'NONE',  ( 0.7660212471507180654, -0.6427876096865404731, 0.005961354470445141482 ) ) ;
#26157 = ORIENTED_EDGE ( 'NONE', *, *, #54241, .F. ) ;
#26158 = ADVANCED_FACE ( 'NONE', ( #23032 ), #9122, .F. ) ;
#26159 = CARTESIAN_POINT ( 'NONE',  ( -10.34095773887371372, -0.1191753592594177180, 6.686594778456397492 ) ) ;
#26160 = VERTEX_POINT ( 'NONE', #17944 ) ;
#26161 = DIRECTION ( 'NONE',  ( 0.005002170337468016433, -0.7660444431189770143, -0.6427681459581293666 ) ) ;
#26162 = EDGE_CURVE ( 'NONE', #10075, #50517, #5702, .T. ) ;
#26163 = ORIENTED_EDGE ( 'NONE', *, *, #20758, .F. ) ;
#26164 = PLANE ( 'NONE',  #16602 ) ;
#26165 = VERTEX_POINT ( 'NONE', #53145 ) ;
#26166 = EDGE_LOOP ( 'NONE', ( #37760, #900, #19764, #42643 ) ) ;
#26167 = ORIENTED_EDGE ( 'NONE', *, *, #45596, .F. ) ;
#26168 = EDGE_CURVE ( 'NONE', #10990, #37130, #44049, .T. ) ;
#26169 = CARTESIAN_POINT ( 'NONE',  ( -29.86197018149027116, 0.000000000000000000, 8.281335066757780083 ) ) ;
#26170 = CARTESIAN_POINT ( 'NONE',  ( -24.27063949748155380, 0.000000000000000000, 6.308861732390097288 ) ) ;
#26171 = DIRECTION ( 'NONE',  ( 0.007781995580012663651, 0.000000000000000000, -0.9999697198139515519 ) ) ;
#26172 = EDGE_CURVE ( 'NONE', #50596, #22114, #5172, .T. ) ;
#26173 = EDGE_CURVE ( 'NONE', #28890, #29609, #18481, .T. ) ;
#26174 = ADVANCED_FACE ( 'NONE', ( #26434 ), #35522, .F. ) ;
#26175 = CARTESIAN_POINT ( 'NONE',  ( -18.67775241435682432, 0.000000000000000000, 4.136394454059623804 ) ) ;
#26176 = ORIENTED_EDGE ( 'NONE', *, *, #13357, .F. ) ;
#26177 = ORIENTED_EDGE ( 'NONE', *, *, #24062, .T. ) ;
#26178 = ORIENTED_EDGE ( 'NONE', *, *, #8816, .T. ) ;
#26179 = DIRECTION ( 'NONE',  ( 0.7660212471507180654, -0.6427876096865404731, 0.005961354470445141482 ) ) ;
#26180 = ORIENTED_EDGE ( 'NONE', *, *, #38815, .F. ) ;
#26181 = CARTESIAN_POINT ( 'NONE',  ( -61.52150108290046404, 8.525944197083212828, -3.000000000000000000 ) ) ;
#26182 = ORIENTED_EDGE ( 'NONE', *, *, #9718, .T. ) ;
#26183 = CARTESIAN_POINT ( 'NONE',  ( -18.69499589319012145, 0.4483081953215045656, 3.929399642557045880 ) ) ;
#26184 = DIRECTION ( 'NONE',  ( 0.9999697198139515519, 0.000000000000000000, 0.007781995580013368816 ) ) ;
#26185 = AXIS2_PLACEMENT_3D ( 'NONE', #35853, #5199, #5736 ) ;
#26186 = ORIENTED_EDGE ( 'NONE', *, *, #9859, .T. ) ;
#26187 = DIRECTION ( 'NONE',  ( 0.005002170337468016433, -0.7660444431189770143, -0.6427681459581293666 ) ) ;
#26188 = EDGE_CURVE ( 'NONE', #13435, #593, #43750, .T. ) ;
#26189 = ORIENTED_EDGE ( 'NONE', *, *, #33678, .T. ) ;
#26190 = EDGE_CURVE ( 'NONE', #16343, #31427, #24410, .T. ) ;
#26191 = CARTESIAN_POINT ( 'NONE',  ( -16.26566120875878596, -1.651309408375658538, 5.710146992570346747 ) ) ;
#26192 = EDGE_LOOP ( 'NONE', ( #4737, #13913, #48776, #41796, #45410 ) ) ;
#26193 = PLANE ( 'NONE',  #9619 ) ;
#26194 = CARTESIAN_POINT ( 'NONE',  ( -24.26908309836554878, 0.000000000000000000, 6.108867788427308376 ) ) ;
#26195 = EDGE_CURVE ( 'NONE', #42767, #20663, #19613, .T. ) ;
#26196 = LINE ( 'NONE', #43500, #13772 ) ;
#26197 = EDGE_LOOP ( 'NONE', ( #15889, #23076, #19127, #18171 ) ) ;
#26198 = LINE ( 'NONE', #1928, #29294 ) ;
#26199 = EDGE_CURVE ( 'NONE', #29379, #6398, #11362, .T. ) ;
#26200 = LINE ( 'NONE', #25355, #22823 ) ;
#26201 = LINE ( 'NONE', #4603, #15816 ) ;
#26202 = LINE ( 'NONE', #30474, #10458 ) ;
#26203 = DIRECTION ( 'NONE',  ( 0.000000000000000000, -1.000000000000000000, 0.000000000000000000 ) ) ;
#26204 = LINE ( 'NONE', #39553, #43345 ) ;
#26205 = DIRECTION ( 'NONE',  ( -0.5449076811759708816, 0.6444004775717707689, 0.5364919789714475140 ) ) ;
#26206 = EDGE_LOOP ( 'NONE', ( #49758, #33774, #40504, #32643 ) ) ;
#26207 = CARTESIAN_POINT ( 'NONE',  ( 2.072287782118878319, 0.000000000000000000, -2.950529333540147015 ) ) ;
#26208 = CARTESIAN_POINT ( 'NONE',  ( -26.09471150760941072, 17.54484258725233659, -4.616176205589227699 ) ) ;
#26209 = CARTESIAN_POINT ( 'NONE',  ( -17.19117404452963171, 0.000000000000000000, 4.147963350671305172 ) ) ;
#26210 = ORIENTED_EDGE ( 'NONE', *, *, #42139, .T. ) ;
#26211 = CARTESIAN_POINT ( 'NONE',  ( -13.07066190154808361, 0.000000000000000000, 12.04713590736729678 ) ) ;
#26212 = ORIENTED_EDGE ( 'NONE', *, *, #5333, .T. ) ;
#26213 = LINE ( 'NONE', #34720, #23476 ) ;
#26214 = CARTESIAN_POINT ( 'NONE',  ( -11.60116101491018448, 0.000000000000000000, 2.344805775598597375 ) ) ;
#26215 = CARTESIAN_POINT ( 'NONE',  ( -18.71224913745325935, -1.813211359398156919, 4.091943217255450627 ) ) ;
#26216 = DIRECTION ( 'NONE',  ( -0.9999697198139514409, -0.000000000000000000, -0.007781995580013368816 ) ) ;
#26217 = ORIENTED_EDGE ( 'NONE', *, *, #29372, .T. ) ;
#26218 = ORIENTED_EDGE ( 'NONE', *, *, #38050, .T. ) ;
#26219 = DIRECTION ( 'NONE',  ( -0.9999697198139514409, -0.000000000000000000, -0.007781995580013368816 ) ) ;
#26220 = CARTESIAN_POINT ( 'NONE',  ( -21.82403829489863156, -4.403642575758161648, 5.218019484613594550 ) ) ;
#26221 = CARTESIAN_POINT ( 'NONE',  ( -22.40634380310664397, 0.000000000000000000, 5.584705972946605534 ) ) ;
#26222 = LINE ( 'NONE', #18241, #48375 ) ;
#26223 = CARTESIAN_POINT ( 'NONE',  ( -27.06630483948590893, -0.1191753592594197858, 7.295098399573937797 ) ) ;
#26224 = LINE ( 'NONE', #6324, #34914 ) ;
#26225 = EDGE_LOOP ( 'NONE', ( #30133, #36936, #42071, #44893 ) ) ;
#26226 = DIRECTION ( 'NONE',  ( 0.6427681459581294776, -0.7660444431189769032, 0.005002170337467562802 ) ) ;
#26227 = PLANE ( 'NONE',  #11546 ) ;
#26228 = ORIENTED_EDGE ( 'NONE', *, *, #54229, .F. ) ;
#26229 = DIRECTION ( 'NONE',  ( -0.005961354470445682716, -0.6427876096865404731, 0.7660212471507180654 ) ) ;
#26230 = FACE_OUTER_BOUND ( 'NONE', #36137, .T. ) ;
#26231 = CARTESIAN_POINT ( 'NONE',  ( -18.29747203306047609, -0.1191753592594177458, 14.03778604627889059 ) ) ;
#26232 = ADVANCED_FACE ( 'NONE', ( #32114 ), #28695, .F. ) ;
#26233 = EDGE_CURVE ( 'NONE', #29241, #7820, #11064, .T. ) ;
#26234 = ORIENTED_EDGE ( 'NONE', *, *, #9923, .T. ) ;
#26235 = CARTESIAN_POINT ( 'NONE',  ( 0.000000000000000000, -1.000000000000000000, 0.000000000000000000 ) ) ;
#26236 = ORIENTED_EDGE ( 'NONE', *, *, #31747, .T. ) ;
#26237 = ADVANCED_FACE ( 'NONE', ( #15341 ), #53672, .F. ) ;
#26238 = ORIENTED_EDGE ( 'NONE', *, *, #1732, .F. ) ;
#26239 = ORIENTED_EDGE ( 'NONE', *, *, #26297, .F. ) ;
#26240 = EDGE_LOOP ( 'NONE', ( #55487, #25571, #30845 ) ) ;
#26241 = LINE ( 'NONE', #42705, #15732 ) ;
#26242 = VERTEX_POINT ( 'NONE', #44889 ) ;
#26243 = CARTESIAN_POINT ( 'NONE',  ( -11.43872127411717443, 24.32207623151542464, -3.308936884429647840 ) ) ;
#26244 = ORIENTED_EDGE ( 'NONE', *, *, #13299, .T. ) ;
#26245 = LINE ( 'NONE', #13477, #53084 ) ;
#26246 = ORIENTED_EDGE ( 'NONE', *, *, #28454, .T. ) ;
#26247 = PLANE ( 'NONE',  #4736 ) ;
#26248 = ORIENTED_EDGE ( 'NONE', *, *, #30632, .F. ) ;
#26249 = EDGE_CURVE ( 'NONE', #41786, #49493, #45425, .T. ) ;
#26250 = CARTESIAN_POINT ( 'NONE',  ( -29.86352658060627618, 0.000000000000000000, 8.481329010720569883 ) ) ;
#26251 = DIRECTION ( 'NONE',  ( 0.007781995580012663651, 0.000000000000000000, -0.9999697198139515519 ) ) ;
#26252 = CARTESIAN_POINT ( 'NONE',  ( -23.33771345073609638, -0.1191753592594197858, 5.846786880686956955 ) ) ;
#26253 = ADVANCED_FACE ( 'NONE', ( #36361 ), #19038, .F. ) ;
#26254 = DIRECTION ( 'NONE',  ( -0.5364919789714478471, 0.6444004775717705469, -0.5449076811759709926 ) ) ;
#26255 = CARTESIAN_POINT ( 'NONE',  ( -18.37467513599760949, 0.6102101463440048335, 5.020127754809787568 ) ) ;
#26256 = ORIENTED_EDGE ( 'NONE', *, *, #49108, .T. ) ;
#26258 = ORIENTED_EDGE ( 'NONE', *, *, #44121, .T. ) ;
#26257 = EDGE_CURVE ( 'NONE', #29027, #32158, #31823, .T. ) ;
#26259 = CARTESIAN_POINT ( 'NONE',  ( -13.03662610889668194, 0.000000000000000000, 7.673609645198246731 ) ) ;
#26260 = LINE ( 'NONE', #52392, #8539 ) ;
#26261 = EDGE_CURVE ( 'NONE', #47262, #53298, #1978, .T. ) ;
#26262 = PLANE ( 'NONE',  #3405 ) ;
#26263 = DIRECTION ( 'NONE',  ( -0.7660212471507179544, -0.6427876096865405842, -0.005961354470445141482 ) ) ;
#26264 = DIRECTION ( 'NONE',  ( 0.000000000000000000, -1.000000000000000000, 0.000000000000000000 ) ) ;
#26265 = CARTESIAN_POINT ( 'NONE',  ( -15.96710241509184058, -0.1191753592594218814, 13.13259134697452879 ) ) ;
#26266 = ORIENTED_EDGE ( 'NONE', *, *, #3309, .F. ) ;
#26267 = CARTESIAN_POINT ( 'NONE',  ( -19.56339837965643369, -0.02924509082106617128, 7.278025012417948858 ) ) ;
#26268 = EDGE_CURVE ( 'NONE', #56189, #33548, #46013, .T. ) ;
#26269 = LINE ( 'NONE', #12656, #50310 ) ;
#26270 = EDGE_LOOP ( 'NONE', ( #37459, #51461, #45066, #18067 ) ) ;
#26271 = CARTESIAN_POINT ( 'NONE',  ( -11.20636620717317378, 0.000000000000000000, 11.32298014792380414 ) ) ;
#26272 = CARTESIAN_POINT ( 'NONE',  ( -17.20398791294004326, 0.000000000000000000, 5.794517922997338921 ) ) ;
#26273 = EDGE_CURVE ( 'NONE', #23095, #48219, #49959, .T. ) ;
#26274 = DIRECTION ( 'NONE',  ( -0.005002170337468016433, -0.7660444431189770143, 0.6427681459581293666 ) ) ;
#26275 = DIRECTION ( 'NONE',  ( 0.5449076811759707706, 0.6444004775717708799, -0.5364919789714476250 ) ) ;
#26276 = FACE_OUTER_BOUND ( 'NONE', #56141, .T. ) ;
#26277 = EDGE_LOOP ( 'NONE', ( #22162, #35978, #9907, #17874 ) ) ;
#26278 = ORIENTED_EDGE ( 'NONE', *, *, #52056, .T. ) ;
#26279 = DIRECTION ( 'NONE',  ( -0.9999697198139514409, -0.000000000000000000, -0.007781995580013368816 ) ) ;
#26280 = DIRECTION ( 'NONE',  ( 0.000000000000000000, -1.000000000000000000, 0.000000000000000000 ) ) ;
#26281 = LINE ( 'NONE', #48417, #25180 ) ;
#26282 = CARTESIAN_POINT ( 'NONE',  ( -13.08486533123210194, 0.000000000000000000, 1.963927175729152541 ) ) ;
#26283 = PLANE ( 'NONE',  #41223 ) ;
#26284 = CARTESIAN_POINT ( 'NONE',  ( -13.94269994003180457, 24.60845428227341003, -3.679749630833339946 ) ) ;
#26285 = DIRECTION ( 'NONE',  ( -0.005002170337468016433, -0.7660444431189770143, 0.6427681459581293666 ) ) ;
#26286 = EDGE_LOOP ( 'NONE', ( #13754, #44367, #16365, #38946 ) ) ;
#26287 = CARTESIAN_POINT ( 'NONE',  ( -19.09948665707623405, -1.165603555308156514, 4.263021500068094660 ) ) ;
#26288 = LINE ( 'NONE', #4708, #38713 ) ;
#26289 = ORIENTED_EDGE ( 'NONE', *, *, #5596, .F. ) ;
#26290 = LINE ( 'NONE', #17791, #43726 ) ;
#26291 = ORIENTED_EDGE ( 'NONE', *, *, #40529, .T. ) ;
#26292 = FACE_OUTER_BOUND ( 'NONE', #19032, .T. ) ;
#26293 = DIRECTION ( 'NONE',  ( -0.8531650599175529814, -0.4028455766673920135, 0.3313982828793697877 ) ) ;
#26294 = EDGE_CURVE ( 'NONE', #46009, #30960, #2275, .T. ) ;
#26295 = ORIENTED_EDGE ( 'NONE', *, *, #52184, .F. ) ;
#26296 = EDGE_LOOP ( 'NONE', ( #4007, #20670, #28375, #44209 ) ) ;
#26297 = EDGE_CURVE ( 'NONE', #54363, #35325, #6278, .T. ) ;
#26298 = EDGE_CURVE ( 'NONE', #40212, #19762, #10553, .T. ) ;
#26299 = ORIENTED_EDGE ( 'NONE', *, *, #44338, .T. ) ;
#26300 = ORIENTED_EDGE ( 'NONE', *, *, #37225, .F. ) ;
#26301 = VERTEX_POINT ( 'NONE', #27566 ) ;
#26302 = EDGE_LOOP ( 'NONE', ( #17596, #4516, #31687, #3736 ) ) ;
#26303 = LINE ( 'NONE', #39086, #6070 ) ;
#26304 = CARTESIAN_POINT ( 'NONE',  ( -23.33849165029409889, 0.000000000000000000, 5.946783852668351855 ) ) ;
#26305 = CARTESIAN_POINT ( 'NONE',  ( -8.975993561185934055, -0.1191753592594197858, 10.41700724906143982 ) ) ;
#26306 = ORIENTED_EDGE ( 'NONE', *, *, #26133, .F. ) ;
#26307 = CARTESIAN_POINT ( 'NONE',  ( -20.30408966804592907, -1.489407457353158160, 4.720599178244390792 ) ) ;
#26308 = ORIENTED_EDGE ( 'NONE', *, *, #11973, .T. ) ;
#26309 = ORIENTED_EDGE ( 'NONE', *, *, #46434, .F. ) ;
#26310 = EDGE_CURVE ( 'NONE', #17219, #6448, #27871, .T. ) ;
#26311 = CARTESIAN_POINT ( 'NONE',  ( -15.13495153988577968, 0.000000000000000000, 12.76973526769478084 ) ) ;
#26312 = CARTESIAN_POINT ( 'NONE',  ( -26.13415699229845757, -0.1191753592594197858, 6.933020519852192365 ) ) ;
#26313 = CARTESIAN_POINT ( 'NONE',  ( -15.86710544311044302, 0.000000000000000000, 13.13336954653252953 ) ) ;
#26314 = EDGE_LOOP ( 'NONE', ( #28319, #47658, #33619, #44604 ) ) ;
#26315 = CARTESIAN_POINT ( 'NONE',  ( -16.99924723426068951, 0.000000000000000000, 13.49389102713827171 ) ) ;
#26316 = ORIENTED_EDGE ( 'NONE', *, *, #51856, .T. ) ;
#26317 = LINE ( 'NONE', #43631, #37354 ) ;
#26318 = CARTESIAN_POINT ( 'NONE',  ( -12.80458192191714595, 0.000000000000000000, 11.86454056839041726 ) ) ;
#26319 = EDGE_CURVE ( 'NONE', #33688, #29013, #2554, .T. ) ;
#26320 = VECTOR ( 'NONE', #33661, 1000.000000000000227 ) ;
#26321 = DIRECTION ( 'NONE',  ( 0.6427681459581294776, -0.7660444431189769032, 0.005002170337467562802 ) ) ;
#26322 = LINE ( 'NONE', #5326, #16812 ) ;
#26323 = ADVANCED_FACE ( 'NONE', ( #40896 ), #6009, .F. ) ;
#26324 = CARTESIAN_POINT ( 'NONE',  ( -15.10534619985566351, 0.000000000000000000, 8.965512652746287614 ) ) ;
#26325 = DIRECTION ( 'NONE',  ( -0.5449076811759708816, 0.6444004775717707689, 0.5364919789714475140 ) ) ;
#26326 = CARTESIAN_POINT ( 'NONE',  ( -66.35525671198902842, -11.31694229433773735, 0.4315550088921851768 ) ) ;
#26327 = ORIENTED_EDGE ( 'NONE', *, *, #36561, .T. ) ;
#26328 = FACE_OUTER_BOUND ( 'NONE', #54562, .T. ) ;
#26329 = LINE ( 'NONE', #4755, #18359 ) ;
#26330 = DIRECTION ( 'NONE',  ( 0.007781995580012662783, 0.000000000000000000, -0.9999697198139514409 ) ) ;
#26331 = DIRECTION ( 'NONE',  ( -0.6427681459581293666, -0.7660444431189770143, -0.005002170337467561935 ) ) ;
#26332 = ADVANCED_FACE ( 'NONE', ( #11902 ), #7962, .F. ) ;
#26333 = DIRECTION ( 'NONE',  ( 0.6427681459581294776, -0.7660444431189769032, 0.005002170337467562802 ) ) ;
#26334 = CARTESIAN_POINT ( 'NONE',  ( -26.13337879274045505, 0.000000000000000000, 6.833023547870798353 ) ) ;
#26335 = CARTESIAN_POINT ( 'NONE',  ( -58.57533928340691887, 0.08623575067603483912, 2.999999999999993339 ) ) ;
#26336 = LINE ( 'NONE', #39418, #52933 ) ;
#26337 = ORIENTED_EDGE ( 'NONE', *, *, #455, .T. ) ;
#26338 = LINE ( 'NONE', #43120, #43856 ) ;
#26339 = CARTESIAN_POINT ( 'NONE',  ( 2.072287782118878319, 0.000000000000000000, -2.950529333540147015 ) ) ;
#26340 = DIRECTION ( 'NONE',  ( -0.7660212471507179544, -0.6427876096865405842, -0.005961354470445141482 ) ) ;
#26341 = ADVANCED_FACE ( 'NONE', ( #55095 ), #34076, .F. ) ;
#26342 = CARTESIAN_POINT ( 'NONE',  ( -14.94838282604900748, -0.1191753592594197858, 2.588085963191248506 ) ) ;
#26343 = PLANE ( 'NONE',  #46648 ) ;
#26344 = LINE ( 'NONE', #20703, #51323 ) ;
#26345 = EDGE_CURVE ( 'NONE', #36770, #43426, #42007, .T. ) ;
#26346 = DIRECTION ( 'NONE',  ( 0.000000000000000000, -0.000000000000000000, -1.000000000000000000 ) ) ;
#26347 = CARTESIAN_POINT ( 'NONE',  ( -69.02283434725003985, -9.743503351218873121, 6.962762944060569836 ) ) ;
#26348 = ORIENTED_EDGE ( 'NONE', *, *, #46440, .T. ) ;
#26349 = DIRECTION ( 'NONE',  ( -0.005002170337468016433, -0.7660444431189770143, 0.6427681459581293666 ) ) ;
#26350 = EDGE_CURVE ( 'NONE', #38597, #11166, #29817, .T. ) ;
#26351 = ORIENTED_EDGE ( 'NONE', *, *, #19180, .F. ) ;
#26352 = VECTOR ( 'NONE', #16525, 1000.000000000000227 ) ;
#26353 = EDGE_CURVE ( 'NONE', #25456, #34036, #25271, .T. ) ;
#26354 = EDGE_CURVE ( 'NONE', #40757, #3468, #12499, .T. ) ;
#26355 = VECTOR ( 'NONE', #32824, 999.9999999999998863 ) ;
#26356 = ORIENTED_EDGE ( 'NONE', *, *, #15474, .T. ) ;
#26357 = ORIENTED_EDGE ( 'NONE', *, *, #35772, .T. ) ;
#26358 = ORIENTED_EDGE ( 'NONE', *, *, #27041, .T. ) ;
#26359 = ORIENTED_EDGE ( 'NONE', *, *, #34913, .F. ) ;
#26360 = DIRECTION ( 'NONE',  ( 0.000000000000000000, -0.000000000000000000, -1.000000000000000000 ) ) ;
#26361 = CARTESIAN_POINT ( 'NONE',  ( -15.83782052860693845, 0.000000000000000000, 9.370320923623856046 ) ) ;
#26362 = EDGE_CURVE ( 'NONE', #41698, #4596, #33769, .T. ) ;
#26363 = ORIENTED_EDGE ( 'NONE', *, *, #37593, .F. ) ;
#26364 = ORIENTED_EDGE ( 'NONE', *, *, #15378, .F. ) ;
#26365 = ADVANCED_FACE ( 'NONE', ( #38608 ), #55939, .F. ) ;
#26366 = FACE_OUTER_BOUND ( 'NONE', #41709, .T. ) ;
#26367 =( BOUNDED_CURVE ( )  B_SPLINE_CURVE ( 3, ( #35492, #9948, #53645, #18169 ),
 .UNSPECIFIED., .F., .F. ) 
 B_SPLINE_CURVE_WITH_KNOTS ( ( 4, 4 ),
 ( 2.756736468966273446, 3.141592653589797113 ),
 .UNSPECIFIED. ) 
 CURVE ( )  GEOMETRIC_REPRESENTATION_ITEM ( )  RATIONAL_B_SPLINE_CURVE ( ( 1.000000000000000000, 0.9876951826469675400, 0.9876951826469675400, 1.000000000000000000 ) ) 
 REPRESENTATION_ITEM ( '' )  );
#26368 = VERTEX_POINT ( 'NONE', #7664 ) ;
#26369 = DIRECTION ( 'NONE',  ( -0.005961354470445682716, -0.6427876096865404731, 0.7660212471507180654 ) ) ;
#26370 = CARTESIAN_POINT ( 'NONE',  ( -15.58059336140243190, -5.213152330870663320, 11.28963442256529426 ) ) ;
#26371 = ORIENTED_EDGE ( 'NONE', *, *, #4935, .T. ) ;
#26372 = CARTESIAN_POINT ( 'NONE',  ( -15.07827343091642014, -4.079838673713162223, 9.234555515054644559 ) ) ;
#26373 = VERTEX_POINT ( 'NONE', #38041 ) ;
#26374 = VECTOR ( 'NONE', #37470, 999.9999999999998863 ) ;
#26375 = CARTESIAN_POINT ( 'NONE',  ( -16.81345671998191449, 0.000000000000000000, 3.412238694616132495 ) ) ;
#26376 = CARTESIAN_POINT ( 'NONE',  ( -10.49818613958752600, -0.3560938001956550081, 1.344194339822732953 ) ) ;
#26377 = PLANE ( 'NONE',  #21458 ) ;
#26378 = VERTEX_POINT ( 'NONE', #15898 ) ;
#26379 = CARTESIAN_POINT ( 'NONE',  ( -26.13493519185646008, 0.000000000000000000, 7.033017491833586377 ) ) ;
#26380 = PLANE ( 'NONE',  #46480 ) ;
#26381 = DIRECTION ( 'NONE',  ( 0.6427681459581294776, -0.7660444431189769032, 0.005002170337467562802 ) ) ;
#26382 = ORIENTED_EDGE ( 'NONE', *, *, #54320, .T. ) ;
#26383 = CARTESIAN_POINT ( 'NONE',  ( -15.88053067323646417, -0.1191753592594197858, 2.950163842912994383 ) ) ;
#26384 = ORIENTED_EDGE ( 'NONE', *, *, #34896, .F. ) ;
#26385 = VECTOR ( 'NONE', #47188, 1000.000000000000114 ) ;
#26386 = CARTESIAN_POINT ( 'NONE',  ( -16.33317936670417225, 0.000000000000000000, 13.31440848639340224 ) ) ;
#26387 = DIRECTION ( 'NONE',  ( 0.6427681459581294776, -0.7660444431189769032, 0.005002170337467562802 ) ) ;
#26388 = CARTESIAN_POINT ( 'NONE',  ( -11.81839927990466954, 0.000000000000000000, 4.559107596029180698 ) ) ;
#26389 = LINE ( 'NONE', #30395, #36858 ) ;
#26390 = EDGE_CURVE ( 'NONE', #51781, #12809, #33243, .T. ) ;
#26391 = CARTESIAN_POINT ( 'NONE',  ( -16.53317331066696383, 0.000000000000000000, 13.31285208727739899 ) ) ;
#26392 = CARTESIAN_POINT ( 'NONE',  ( 1.086233639165236964, 0.000000000000000000, 2.796443541562362078 ) ) ;
#26393 = DIRECTION ( 'NONE',  ( 0.000000000000000000, 1.000000000000000000, 0.000000000000000000 ) ) ;
#26394 = VECTOR ( 'NONE', #27534, 999.9999999999998863 ) ;
#26395 = FACE_OUTER_BOUND ( 'NONE', #77, .T. ) ;
#26396 =( LENGTH_UNIT ( ) NAMED_UNIT ( * ) SI_UNIT ( .MILLI., .METRE. ) );
#26397 = CARTESIAN_POINT ( 'NONE',  ( -22.40478740399063895, 0.000000000000000000, 5.384712028983816623 ) ) ;
#26398 = ORIENTED_EDGE ( 'NONE', *, *, #47031, .T. ) ;
#26399 = LINE ( 'NONE', #3700, #46559 ) ;
#26400 = CARTESIAN_POINT ( 'NONE',  ( -18.78639633340495152, 0.000000000000000000, 4.304874975546248983 ) ) ;
#26401 = DIRECTION ( 'NONE',  ( 0.000000000000000000, -0.000000000000000000, -1.000000000000000000 ) ) ;
#26402 = ADVANCED_FACE ( 'NONE', ( #11650 ), #37780, .F. ) ;
#26403 = CARTESIAN_POINT ( 'NONE',  ( -18.72385110809067399, 3.200641362704007786, 9.407098503644062859 ) ) ;
#26404 = EDGE_CURVE ( 'NONE', #29543, #13781, #29538, .T. ) ;
#26405 = LINE ( 'NONE', #51689, #19668 ) ;
#26406 = EDGE_CURVE ( 'NONE', #47842, #30584, #24988, .T. ) ;
#26407 = DIRECTION ( 'NONE',  ( -0.7660212471507179544, -0.6427876096865405842, -0.005961354470445141482 ) ) ;
#26408 = ORIENTED_EDGE ( 'NONE', *, *, #43551, .F. ) ;
#26409 = ORIENTED_EDGE ( 'NONE', *, *, #33559, .F. ) ;
#26410 = DIRECTION ( 'NONE',  ( -0.7660212471507179544, -0.6427876096865405842, -0.005961354470445141482 ) ) ;
#26411 = CARTESIAN_POINT ( 'NONE',  ( -26.13415699229845757, -0.1191753592594197858, 6.933020519852192365 ) ) ;
#26412 = ORIENTED_EDGE ( 'NONE', *, *, #12613, .T. ) ;
#26413 = LINE ( 'NONE', #38937, #8458 ) ;
#26414 = VECTOR ( 'NONE', #41151, 999.9999999999998863 ) ;
#26415 = VECTOR ( 'NONE', #15909, 1000.000000000000227 ) ;
#26416 = ORIENTED_EDGE ( 'NONE', *, *, #34388, .F. ) ;
#26417 = ADVANCED_FACE ( 'NONE', ( #20727 ), #55350, .F. ) ;
#26418 = CARTESIAN_POINT ( 'NONE',  ( -21.18998281933104622, 5.629170628041515023, 4.733240658386350219 ) ) ;
#26419 = ORIENTED_EDGE ( 'NONE', *, *, #3841, .T. ) ;
#26420 = PLANE ( 'NONE',  #45621 ) ;
#26421 = ADVANCED_FACE ( 'NONE', ( #38308 ), #15512, .F. ) ;
#26422 = EDGE_LOOP ( 'NONE', ( #49407, #52372, #43781, #33853 ) ) ;
#26423 = ORIENTED_EDGE ( 'NONE', *, *, #52554, .T. ) ;
#26424 = ORIENTED_EDGE ( 'NONE', *, *, #24062, .F. ) ;
#26425 = DIRECTION ( 'NONE',  ( 0.7660212471507180654, -0.6427876096865404731, 0.005961354470445141482 ) ) ;
#26426 = CARTESIAN_POINT ( 'NONE',  ( -16.99924723426068951, 0.000000000000000000, 13.49389102713827171 ) ) ;
#26427 = CARTESIAN_POINT ( 'NONE',  ( -13.50281940485377064, 0.000000000000000000, 7.869987677393025294 ) ) ;
#26428 = ADVANCED_FACE ( 'NONE', ( #32837 ), #27775, .F. ) ;
#26429 = LINE ( 'NONE', #872, #21123 ) ;
#26430 = ORIENTED_EDGE ( 'NONE', *, *, #32786, .F. ) ;
#26431 = ORIENTED_EDGE ( 'NONE', *, *, #54894, .T. ) ;
#26432 = AXIS2_PLACEMENT_3D ( 'NONE', #15600, #42010, #2814 ) ;
#26433 = EDGE_CURVE ( 'NONE', #51326, #16268, #16097, .T. ) ;
#26434 = FACE_OUTER_BOUND ( 'NONE', #29534, .T. ) ;
#26435 = VERTEX_POINT ( 'NONE', #28879 ) ;
#26436 = CARTESIAN_POINT ( 'NONE',  ( -20.54049170961573267, 0.000000000000000000, 4.660556269540326646 ) ) ;
#26437 = ORIENTED_EDGE ( 'NONE', *, *, #43942, .F. ) ;
#26438 = CARTESIAN_POINT ( 'NONE',  ( -13.01650773435970443, 0.000000000000000000, 5.088441722393895361 ) ) ;
#26439 = DIRECTION ( 'NONE',  ( 0.007781995580012663651, -3.146120232559066537E-19, -0.9999697198139514409 ) ) ;
#26440 = VERTEX_POINT ( 'NONE', #45345 ) ;
#26441 = PLANE ( 'NONE',  #5075 ) ;
#26442 = ORIENTED_EDGE ( 'NONE', *, *, #36479, .T. ) ;
#26443 = FACE_OUTER_BOUND ( 'NONE', #28013, .T. ) ;
#26444 = ORIENTED_EDGE ( 'NONE', *, *, #28812, .T. ) ;
#26445 = CARTESIAN_POINT ( 'NONE',  ( -21.27912796733415135, -3.756034771668161909, 5.027019887704494039 ) ) ;
#26446 = CARTESIAN_POINT ( 'NONE',  ( -11.17233041452177211, 0.000000000000000000, 6.949453885754755866 ) ) ;
#26447 = DIRECTION ( 'NONE',  ( -0.5364919789714478471, 0.6444004775717705469, -0.5449076811759709926 ) ) ;
#26448 = EDGE_LOOP ( 'NONE', ( #5358, #762, #32330, #32922 ) ) ;
#26450 = CARTESIAN_POINT ( 'NONE',  ( 2.072287782118878319, 0.000000000000000000, -2.950529333540147015 ) ) ;
#26449 = CIRCLE ( 'NONE', #50930, 2.125000000000000000 ) ;
#26451 = VECTOR ( 'NONE', #38969, 1000.000000000000227 ) ;
#26452 = CARTESIAN_POINT ( 'NONE',  ( -12.09010799418281579, 0.000000000000000000, 5.464983249187678638 ) ) ;
#26453 = DIRECTION ( 'NONE',  ( -0.9999697198139514409, -0.000000000000000000, -0.007781995580013368816 ) ) ;
#26454 = EDGE_CURVE ( 'NONE', #30915, #9089, #7030, .T. ) ;
#26455 = DIRECTION ( 'NONE',  ( 0.005961354470445682716, -0.6427876096865404731, -0.7660212471507180654 ) ) ;
#26456 = DIRECTION ( 'NONE',  ( -0.005961354470445682716, -0.6427876096865404731, 0.7660212471507180654 ) ) ;
#26457 = LINE ( 'NONE', #644, #10721 ) ;
#26458 = EDGE_CURVE ( 'NONE', #21645, #28247, #37113, .T. ) ;
#26459 = SURFACE_STYLE_USAGE ( .BOTH. , #21922 ) ;
#26460 = VECTOR ( 'NONE', #47592, 999.9999999999998863 ) ;
#26461 = ORIENTED_EDGE ( 'NONE', *, *, #17019, .F. ) ;
#26462 = DIRECTION ( 'NONE',  ( 0.005002170337468016433, -0.7660444431189770143, -0.6427681459581293666 ) ) ;
#26463 = LINE ( 'NONE', #38723, #51288 ) ;
#26464 = CARTESIAN_POINT ( 'NONE',  ( -13.73672976910459909, 0.000000000000000000, 12.22661844811216270 ) ) ;
#26465 = ORIENTED_EDGE ( 'NONE', *, *, #12982, .F. ) ;
#26466 = LINE ( 'NONE', #4067, #24758 ) ;
#26467 = PLANE ( 'NONE',  #30896 ) ;
#26468 = ORIENTED_EDGE ( 'NONE', *, *, #30967, .F. ) ;
#26469 = ADVANCED_FACE ( 'NONE', ( #7280 ), #19792, .F. ) ;
#26470 = ADVANCED_FACE ( 'NONE', ( #54164 ), #2720, .F. ) ;
#26471 = EDGE_CURVE ( 'NONE', #42993, #29692, #45618, .T. ) ;
#26472 = LINE ( 'NONE', #17384, #13501 ) ;
#26473 = DIRECTION ( 'NONE',  ( 0.9999697198139515519, 0.000000000000000000, 0.007781995580013368816 ) ) ;
#26474 = AXIS2_PLACEMENT_3D ( 'NONE', #25217, #3888, #20923 ) ;
#26475 = DIRECTION ( 'NONE',  ( 0.7660212471507180654, -0.6427876096865404731, 0.005961354470445141482 ) ) ;
#26476 = VECTOR ( 'NONE', #12441, 1000.000000000000227 ) ;
#26477 = ADVANCED_FACE ( 'NONE', ( #54412 ), #3008, .F. ) ;
#26478 = CARTESIAN_POINT ( 'NONE',  ( -18.22541471764576215, -0.1191753592594165800, 4.778575762111413994 ) ) ;
#26479 = ORIENTED_EDGE ( 'NONE', *, *, #55113, .T. ) ;
#26480 = EDGE_LOOP ( 'NONE', ( #17128, #31180, #44337, #15184 ) ) ;
#26481 = DIRECTION ( 'NONE',  ( 0.007781995580012663651, 0.000000000000000000, -0.9999697198139515519 ) ) ;
#26482 = DIRECTION ( 'NONE',  ( 0.000000000000000000, -0.000000000000000000, -1.000000000000000000 ) ) ;
#26483 = FACE_OUTER_BOUND ( 'NONE', #55775, .T. ) ;
#26484 = DIRECTION ( 'NONE',  ( 0.5449076811759707706, 0.6444004775717708799, -0.5364919789714476250 ) ) ;
#26485 = DIRECTION ( 'NONE',  ( 0.5364919789714477361, 0.6444004775717706579, 0.5449076811759711036 ) ) ;
#26486 = ADVANCED_FACE ( 'NONE', ( #20337 ), #6457, .F. ) ;
#26487 = CARTESIAN_POINT ( 'NONE',  ( -18.67775241435682432, 0.000000000000000000, 4.136394454059623804 ) ) ;
#26488 = ORIENTED_EDGE ( 'NONE', *, *, #50187, .F. ) ;
#26489 = DIRECTION ( 'NONE',  ( 0.9999697198139515519, 0.000000000000000000, 0.007781995580013368816 ) ) ;
#26490 = EDGE_CURVE ( 'NONE', #47842, #18253, #37371, .T. ) ;
#26491 = LINE ( 'NONE', #34462, #2461 ) ;
#26492 = ORIENTED_EDGE ( 'NONE', *, *, #26071, .F. ) ;
#26493 = EDGE_CURVE ( 'NONE', #9089, #46401, #41085, .T. ) ;
#26494 = CARTESIAN_POINT ( 'NONE',  ( -13.70716283399377922, -4.727446477803165514, 2.054818365572432803 ) ) ;
#26495 = CIRCLE ( 'NONE', #52794, 6.000000000000002665 ) ;
#26496 = PLANE ( 'NONE',  #47682 ) ;
#26497 = PLANE ( 'NONE',  #39314 ) ;
#26498 = ORIENTED_EDGE ( 'NONE', *, *, #53692, .F. ) ;
#26499 = AXIS2_PLACEMENT_3D ( 'NONE', #32517, #28233, #50662 ) ;
#26500 = EDGE_CURVE ( 'NONE', #18417, #26092, #37678, .T. ) ;
#26501 = VECTOR ( 'NONE', #37488, 999.9999999999998863 ) ;
#26502 = DIRECTION ( 'NONE',  ( -0.7660212471507179544, -0.6427876096865405842, -0.005961354470445141482 ) ) ;
#26503 = ORIENTED_EDGE ( 'NONE', *, *, #50355, .F. ) ;
#26504 = ORIENTED_EDGE ( 'NONE', *, *, #18114, .F. ) ;
#26505 = VECTOR ( 'NONE', #16645, 999.9999999999998863 ) ;
#26506 = EDGE_LOOP ( 'NONE', ( #23524, #49010, #15590, #33295 ) ) ;
#26507 = AXIS2_PLACEMENT_3D ( 'NONE', #15102, #29250, #32428 ) ;
#26508 = ORIENTED_EDGE ( 'NONE', *, *, #13316, .T. ) ;
#26509 = DIRECTION ( 'NONE',  ( -0.9999697198139514409, -0.000000000000000000, -0.007781995580013368816 ) ) ;
#26510 = ORIENTED_EDGE ( 'NONE', *, *, #53206, .F. ) ;
#26511 = DIRECTION ( 'NONE',  ( -0.7660212471507179544, -0.6427876096865405842, -0.005961354470445141482 ) ) ;
#26512 = ORIENTED_EDGE ( 'NONE', *, *, #50722, .T. ) ;
#26513 = CARTESIAN_POINT ( 'NONE',  ( -14.00280974873554030, 0.000000000000000000, 12.40921378708904044 ) ) ;
#26514 = EDGE_LOOP ( 'NONE', ( #38224, #19025, #45266, #7744 ) ) ;
#26516 = VECTOR ( 'NONE', #21142, 1000.000000000000114 ) ;
#26515 = CARTESIAN_POINT ( 'NONE',  ( -27.06708303904391144, 0.000000000000000000, 7.395095371555332697 ) ) ;
#26517 = VERTEX_POINT ( 'NONE', #36551 ) ;
#26518 = DIRECTION ( 'NONE',  ( 0.005002170337468016433, -0.7660444431189770143, -0.6427681459581293666 ) ) ;
#26519 = DIRECTION ( 'NONE',  ( -0.3620778797217461542, -0.000000000000000000, -0.9321478471874538041 ) ) ;
#26520 = CARTESIAN_POINT ( 'NONE',  ( -9.031591052444445822, -0.1191753592594191058, 3.742128014318059748 ) ) ;
#26521 = DIRECTION ( 'NONE',  ( 0.005002170337468016433, -0.7660444431189770143, -0.6427681459581293666 ) ) ;
#26522 = CARTESIAN_POINT ( 'NONE',  ( -11.67244013076689946, 0.000000000000000000, 11.50401908778467863 ) ) ;
#26523 = VERTEX_POINT ( 'NONE', #14980 ) ;
#26524 = EDGE_CURVE ( 'NONE', #54227, #44519, #28300, .T. ) ;
#26525 = VERTEX_POINT ( 'NONE', #32315 ) ;
#26526 = DIRECTION ( 'NONE',  ( -0.5364919789714478471, 0.6444004775717705469, -0.5449076811759709926 ) ) ;
#26527 = FACE_OUTER_BOUND ( 'NONE', #35602, .T. ) ;
#26528 = EDGE_CURVE ( 'NONE', #19226, #27412, #23501, .T. ) ;
#26529 = VECTOR ( 'NONE', #54461, 1000.000000000000114 ) ;
#26530 = LINE ( 'NONE', #9803, #23361 ) ;
#26531 = DIRECTION ( 'NONE',  ( 0.007781995580012663651, -3.146120232559066537E-19, -0.9999697198139514409 ) ) ;
#26532 = DIRECTION ( 'NONE',  ( 0.000000000000000000, -0.000000000000000000, -1.000000000000000000 ) ) ;
#26533 = CARTESIAN_POINT ( 'NONE',  ( -18.67775241435682432, 0.000000000000000000, 4.136394454059623804 ) ) ;
#26534 = VERTEX_POINT ( 'NONE', #19508 ) ;
#26536 = DIRECTION ( 'NONE',  ( -0.005002170337468016433, -0.7660444431189770143, 0.6427681459581293666 ) ) ;
#26535 = AXIS2_PLACEMENT_3D ( 'NONE', #10606, #44642, #2603 ) ;
#26537 = DIRECTION ( 'NONE',  ( 0.5449076811759707706, 0.6444004775717708799, -0.5364919789714476250 ) ) ;
#26538 = EDGE_LOOP ( 'NONE', ( #56127, #14320, #18064, #49268 ) ) ;
#26539 = EDGE_CURVE ( 'NONE', #33244, #27552, #36855, .T. ) ;
#26540 = EDGE_CURVE ( 'NONE', #45468, #48012, #20642, .T. ) ;
#26541 = EDGE_CURVE ( 'NONE', #36489, #6114, #56118, .T. ) ;
#26542 = VECTOR ( 'NONE', #9893, 999.9999999999998863 ) ;
#26543 = AXIS2_PLACEMENT_3D ( 'NONE', #19832, #15553, #32883 ) ;
#26544 = CARTESIAN_POINT ( 'NONE',  ( -68.70267651662487651, -8.968872329527044940, -6.959823595413025643 ) ) ;
#26545 = CARTESIAN_POINT ( 'NONE',  ( -61.38973930853472183, 7.404220597074748333, 2.999999999999993339 ) ) ;
#26546 = EDGE_CURVE ( 'NONE', #53450, #20294, #55260, .T. ) ;
#26547 = DIRECTION ( 'NONE',  ( 0.9999697198139515519, 0.000000000000000000, 0.007781995580013368816 ) ) ;
#26548 = FACE_OUTER_BOUND ( 'NONE', #47179, .T. ) ;
#26549 = ORIENTED_EDGE ( 'NONE', *, *, #9612, .T. ) ;
#26550 = AXIS2_PLACEMENT_3D ( 'NONE', #48661, #44647, #39847 ) ;
#26551 = VECTOR ( 'NONE', #23804, 1000.000000000000114 ) ;
#26552 = EDGE_LOOP ( 'NONE', ( #7172, #37381, #44512, #44936 ) ) ;
#26553 = DIRECTION ( 'NONE',  ( 0.7660212471507180654, -0.6427876096865404731, 0.005961354470445141482 ) ) ;
#26554 = LINE ( 'NONE', #22018, #10452 ) ;
#26555 = CARTESIAN_POINT ( 'NONE',  ( -56.48844206942440138, 5.522788861961955398, -3.000000000000007105 ) ) ;
#26556 = FACE_OUTER_BOUND ( 'NONE', #45262, .T. ) ;
#26557 = VECTOR ( 'NONE', #13355, 1000.000000000000227 ) ;
#26558 = CARTESIAN_POINT ( 'NONE',  ( 5.618093201498282063, -1.050357395465043364, -2.260480044901387764 ) ) ;
#26560 = AXIS2_PLACEMENT_3D ( 'NONE', #35986, #26884, #19171 ) ;
#26559 = DIRECTION ( 'NONE',  ( 0.000000000000000000, -0.000000000000000000, -1.000000000000000000 ) ) ;
#26561 = CARTESIAN_POINT ( 'NONE',  ( -13.03087800188611567, 0.000000000000000000, 6.934990238682716246 ) ) ;
#26562 = ADVANCED_FACE ( 'NONE', ( #17203 ), #39066, .F. ) ;
#26563 = PLANE ( 'NONE',  #8755 ) ;
#26564 = DIRECTION ( 'NONE',  ( 0.000000000000000000, -1.000000000000000000, 0.000000000000000000 ) ) ;
#26565 = ADVANCED_FACE ( 'NONE', ( #47292 ), #42493, .F. ) ;
#26566 = VERTEX_POINT ( 'NONE', #8401 ) ;
#26567 = CARTESIAN_POINT ( 'NONE',  ( -10.47421230394850866, 0.000000000000000000, 10.95934586908605723 ) ) ;
#26568 = VERTEX_POINT ( 'NONE', #37953 ) ;
#26569 = DIRECTION ( 'NONE',  ( 0.007781995580012663651, 0.000000000000000000, -0.9999697198139515519 ) ) ;
#26570 = AXIS2_PLACEMENT_3D ( 'NONE', #5936, #1656, #48813 ) ;
#26571 = CARTESIAN_POINT ( 'NONE',  ( -15.13495153988577968, 0.000000000000000000, 12.76973526769478084 ) ) ;
#26572 = VERTEX_POINT ( 'NONE', #4161 ) ;
#26573 = EDGE_CURVE ( 'NONE', #37960, #17288, #33972, .T. ) ;
#26574 = AXIS2_PLACEMENT_3D ( 'NONE', #25875, #55977, #43206 ) ;
#26575 = ORIENTED_EDGE ( 'NONE', *, *, #1808, .F. ) ;
#26576 = EDGE_CURVE ( 'NONE', #35922, #20993, #42750, .T. ) ;
#26577 = ORIENTED_EDGE ( 'NONE', *, *, #7426, .T. ) ;
#26578 = EDGE_LOOP ( 'NONE', ( #48725, #36367, #39363, #11518 ) ) ;
#26579 = ORIENTED_EDGE ( 'NONE', *, *, #3593, .T. ) ;
#26580 = EDGE_LOOP ( 'NONE', ( #5213, #54200, #31190, #20297 ) ) ;
#26581 = AXIS2_PLACEMENT_3D ( 'NONE', #14240, #32395, #49701 ) ;
#26582 = FACE_OUTER_BOUND ( 'NONE', #8417, .T. ) ;
#26583 = CARTESIAN_POINT ( 'NONE',  ( -5.362734387325203578, 5.246864883482168729, 5.301441730927289875 ) ) ;
#26584 = DIRECTION ( 'NONE',  ( -0.5449076811759708816, 0.6444004775717707689, 0.5364919789714475140 ) ) ;
#26585 = VECTOR ( 'NONE', #140, 999.9999999999998863 ) ;
#26586 = VECTOR ( 'NONE', #36078, 999.9999999999998863 ) ;
#26587 = ORIENTED_EDGE ( 'NONE', *, *, #20658, .F. ) ;
#26588 = LINE ( 'NONE', #43905, #1349 ) ;
#26589 = ORIENTED_EDGE ( 'NONE', *, *, #41658, .T. ) ;
#26590 = ORIENTED_EDGE ( 'NONE', *, *, #2013, .T. ) ;
#26591 = ADVANCED_BREP_SHAPE_REPRESENTATION ( '', ( #41703, #2610 ), #1760 ) ;
#26592 = VECTOR ( 'NONE', #33759, 1000.000000000000227 ) ;
#26593 = VECTOR ( 'NONE', #31855, 1000.000000000000114 ) ;
#26594 = PLANE ( 'NONE',  #42086 ) ;
#26595 = DIRECTION ( 'NONE',  ( 0.005002170337468016433, -0.7660444431189770143, -0.6427681459581293666 ) ) ;
#26596 = CARTESIAN_POINT ( 'NONE',  ( -4.545936964608350728, -6.455664940184357548, 4.984169873386830041 ) ) ;
#26597 = ORIENTED_EDGE ( 'NONE', *, *, #38402, .F. ) ;
#26598 = DIRECTION ( 'NONE',  ( -0.005961354470445682716, -0.6427876096865404731, 0.7660212471507180654 ) ) ;
#26599 = ORIENTED_EDGE ( 'NONE', *, *, #2135, .T. ) ;
#26600 = DIRECTION ( 'NONE',  ( -0.005002170337468016433, -0.7660444431189770143, 0.6427681459581293666 ) ) ;
#26601 = VECTOR ( 'NONE', #32538, 999.9999999999998863 ) ;
#26602 = CARTESIAN_POINT ( 'NONE',  ( -10.74029228357944987, 0.000000000000000000, 11.14194120806293320 ) ) ;
#26603 = CARTESIAN_POINT ( 'NONE',  ( -19.12962290826653700, 0.000000000000000000, 14.40064212555863854 ) ) ;
#26604 = CARTESIAN_POINT ( 'NONE',  ( -24.26986129792355129, -0.1191753592594197858, 6.208864760408702388 ) ) ;
#26605 = CARTESIAN_POINT ( 'NONE',  ( 5.518825648885151480, -1.048584701394832619, -2.502082349829454877 ) ) ;
#26606 = LINE ( 'NONE', #8447, #31192 ) ;
#26607 = FACE_OUTER_BOUND ( 'NONE', #54848, .T. ) ;
#26608 = ORIENTED_EDGE ( 'NONE', *, *, #36120, .F. ) ;
#26609 = CARTESIAN_POINT ( 'NONE',  ( -12.75473883498668570, 0.000000000000000000, 5.459810938303666816 ) ) ;
#26610 = VECTOR ( 'NONE', #34165, 1000.000000000000000 ) ;
#26611 = EDGE_CURVE ( 'NONE', #18181, #32585, #20891, .T. ) ;
#26612 = CARTESIAN_POINT ( 'NONE',  ( -17.40553825601883275, 0.000000000000000000, 5.992955467844123696 ) ) ;
#26613 = DIRECTION ( 'NONE',  ( -0.6427681459581293666, -0.7660444431189770143, -0.005002170337467561935 ) ) ;
#26614 = DIRECTION ( 'NONE',  ( -0.6246952433987893460, -0.7422098413412802076, 0.2426528472758542054 ) ) ;
#26615 = AXIS2_PLACEMENT_3D ( 'NONE', #52354, #22243, #25960 ) ;
#26616 = CARTESIAN_POINT ( 'NONE',  ( -28.51944453287105219, 14.46051606012035151, -4.734328798303309327 ) ) ;
#26617 = DIRECTION ( 'NONE',  ( 0.005961354470445682716, -0.6427876096865404731, -0.7660212471507180654 ) ) ;
#26618 = EDGE_CURVE ( 'NONE', #28751, #35036, #38504, .T. ) ;
#26619 = EDGE_CURVE ( 'NONE', #19450, #2403, #29986, .T. ) ;
#26620 = CARTESIAN_POINT ( 'NONE',  ( -15.87975247367846166, 0.000000000000000000, 2.850166870931599927 ) ) ;
#26621 = LINE ( 'NONE', #16704, #21053 ) ;
#26622 = ORIENTED_EDGE ( 'NONE', *, *, #32280, .F. ) ;
#26623 = VECTOR ( 'NONE', #22338, 999.9999999999998863 ) ;
#26624 = CARTESIAN_POINT ( 'NONE',  ( -12.15116108492864377, 0.000000000000000000, 1.401855352044617975 ) ) ;
#26625 = PLANE ( 'NONE',  #48496 ) ;
#26626 = DIRECTION ( 'NONE',  ( -0.9321478471874540261, 0.000000000000000000, 0.3620778797217457656 ) ) ;
#26627 = AXIS2_PLACEMENT_3D ( 'NONE', #48954, #23119, #31365 ) ;
#26628 = AXIS2_PLACEMENT_3D ( 'NONE', #26515, #52632, #44139 ) ;
#26629 = LINE ( 'NONE', #43947, #37317 ) ;
#26630 = CARTESIAN_POINT ( 'NONE',  ( -19.32961685222932147, 0.000000000000000000, 14.39908572644263351 ) ) ;
#26631 = CARTESIAN_POINT ( 'NONE',  ( -14.01545677930355183, 0.000000000000000000, 2.126011111488108174 ) ) ;
#26632 = CARTESIAN_POINT ( 'NONE',  ( -14.20280369269832832, 0.000000000000000000, 12.40765738797303719 ) ) ;
#26633 = VECTOR ( 'NONE', #41033, 1000.000000000000000 ) ;
#26634 = VECTOR ( 'NONE', #39765, 1000.000000000000000 ) ;
#26635 = CARTESIAN_POINT ( 'NONE',  ( -67.24306867387670650, -9.539447468475627190, -3.347029521210262981 ) ) ;
#26636 = PLANE ( 'NONE',  #50977 ) ;
#26637 = EDGE_LOOP ( 'NONE', ( #809, #15458, #34755, #35967 ) ) ;
#26638 = EDGE_CURVE ( 'NONE', #11765, #280, #25729, .T. ) ;
#26639 = ORIENTED_EDGE ( 'NONE', *, *, #26956, .T. ) ;
#26640 = ORIENTED_EDGE ( 'NONE', *, *, #35815, .F. ) ;
#26641 = VERTEX_POINT ( 'NONE', #55536 ) ;
#26642 = VECTOR ( 'NONE', #41536, 1000.000000000000227 ) ;
#26643 = EDGE_CURVE ( 'NONE', #5703, #42294, #12945, .T. ) ;
#26644 = ORIENTED_EDGE ( 'NONE', *, *, #27193, .T. ) ;
#26645 = DIRECTION ( 'NONE',  ( 0.7660212471507180654, -0.6427876096865404731, 0.005961354470445141482 ) ) ;
#26646 = EDGE_CURVE ( 'NONE', #36770, #13988, #11815, .T. ) ;
#26647 = DIRECTION ( 'NONE',  ( 0.000000000000000000, -1.000000000000000000, 0.000000000000000000 ) ) ;
#26648 = VECTOR ( 'NONE', #1613, 999.9999999999998863 ) ;
#26649 = ORIENTED_EDGE ( 'NONE', *, *, #667, .F. ) ;
#26650 = ORIENTED_EDGE ( 'NONE', *, *, #41847, .F. ) ;
#26651 = EDGE_CURVE ( 'NONE', #24469, #25199, #38806, .T. ) ;
#26652 = VECTOR ( 'NONE', #16137, 999.9999999999998863 ) ;
#26653 = DIRECTION ( 'NONE',  ( 0.5449076811759707706, 0.6444004775717708799, -0.5364919789714476250 ) ) ;
#26654 = ORIENTED_EDGE ( 'NONE', *, *, #11248, .T. ) ;
#26655 = VECTOR ( 'NONE', #54854, 999.9999999999998863 ) ;
#26656 = DIRECTION ( 'NONE',  ( 0.007781995580012662783, 0.000000000000000000, -0.9999697198139514409 ) ) ;
#26657 = CARTESIAN_POINT ( 'NONE',  ( -12.53706982000896630, -1.651309408375658538, 4.261835473683364128 ) ) ;
#26658 = ORIENTED_EDGE ( 'NONE', *, *, #48812, .T. ) ;
#26659 = LINE ( 'NONE', #35456, #43688 ) ;
#26660 = VECTOR ( 'NONE', #37487, 1000.000000000000114 ) ;
#26661 = ORIENTED_EDGE ( 'NONE', *, *, #44278, .F. ) ;
#26662 = DIRECTION ( 'NONE',  ( 0.7660212471507180654, -0.6427876096865404731, 0.005961354470445141482 ) ) ;
#26663 = LINE ( 'NONE', #29627, #45614 ) ;
#26664 = VECTOR ( 'NONE', #2719, 1000.000000000000227 ) ;
#26665 = DIRECTION ( 'NONE',  ( -0.005961354470445682716, -0.6427876096865404731, 0.7660212471507180654 ) ) ;
#26666 = FACE_OUTER_BOUND ( 'NONE', #4532, .T. ) ;
#26667 = VECTOR ( 'NONE', #53514, 999.9999999999998863 ) ;
#26668 = ORIENTED_EDGE ( 'NONE', *, *, #51142, .T. ) ;
#26669 = DIRECTION ( 'NONE',  ( 0.5364919789714477361, 0.6444004775717706579, 0.5449076811759711036 ) ) ;
#26670 = CARTESIAN_POINT ( 'NONE',  ( -18.13900981363277864, 0.000000000000000000, 6.525905505976847820 ) ) ;
#26671 = DIRECTION ( 'NONE',  ( -0.7660212471507179544, -0.6427876096865405842, -0.005961354470445141482 ) ) ;
#26672 = ORIENTED_EDGE ( 'NONE', *, *, #25740, .T. ) ;
#26673 = CARTESIAN_POINT ( 'NONE',  ( -14.93495759592298988, 0.000000000000000000, 12.77129166681078409 ) ) ;
#26674 = ADVANCED_FACE ( 'NONE', ( #7871 ), #12411, .F. ) ;
#26675 = EDGE_LOOP ( 'NONE', ( #31439, #6414, #32408, #41824 ) ) ;
#26676 = EDGE_CURVE ( 'NONE', #36742, #40396, #47866, .T. ) ;
#26677 = FACE_OUTER_BOUND ( 'NONE', #54023, .T. ) ;
#26678 = LINE ( 'NONE', #18151, #16936 ) ;
#26679 = DIRECTION ( 'NONE',  ( -0.5449076811759708816, 0.6444004775717707689, 0.5364919789714475140 ) ) ;
#26680 = PLANE ( 'NONE',  #34135 ) ;
#26681 = DIRECTION ( 'NONE',  ( 0.007781995580012663651, 0.000000000000000000, -0.9999697198139515519 ) ) ;
#26682 = DIRECTION ( 'NONE',  ( 0.9999697198139515519, 0.000000000000000000, 0.007781995580013368816 ) ) ;
#26683 = EDGE_CURVE ( 'NONE', #36758, #5924, #5287, .T. ) ;
#26684 = CARTESIAN_POINT ( 'NONE',  ( 0.4518049228021103203, -3.655895688227122076, 5.998622290806040702 ) ) ;
#26685 = VECTOR ( 'NONE', #24553, 1000.000000000000114 ) ;
#26686 = CARTESIAN_POINT ( 'NONE',  ( 2.072287782118878319, 0.000000000000000000, -2.950529333540147015 ) ) ;
#26687 = CARTESIAN_POINT ( 'NONE',  ( -23.33693525117809386, 0.000000000000000000, 5.746789908705562944 ) ) ;
#26688 = EDGE_LOOP ( 'NONE', ( #54173, #2874, #3155, #19540 ) ) ;
#26689 = CARTESIAN_POINT ( 'NONE',  ( -17.04576418467708621, 1.257817950434005683, 3.262954439389057271 ) ) ;
#26690 = LINE ( 'NONE', #18164, #50304 ) ;
#26691 = FACE_OUTER_BOUND ( 'NONE', #3575, .T. ) ;
#26692 = AXIS2_PLACEMENT_3D ( 'NONE', #42724, #3823, #21149 ) ;
#26693 = CARTESIAN_POINT ( 'NONE',  ( -15.76334127827276888, -0.5179957512181551094, 3.655068085059692606 ) ) ;
#26694 = PLANE ( 'NONE',  #13695 ) ;
#26695 = FACE_OUTER_BOUND ( 'NONE', #23578, .T. ) ;
#26696 = PLANE ( 'NONE',  #3911 ) ;
#26697 = ADVANCED_FACE ( 'NONE', ( #1273 ), #22598, .F. ) ;
#26698 = ORIENTED_EDGE ( 'NONE', *, *, #44578, .T. ) ;
#26699 = VECTOR ( 'NONE', #3826, 1000.000000000000114 ) ;
#26700 = ORIENTED_EDGE ( 'NONE', *, *, #126, .F. ) ;
#26701 = DIRECTION ( 'NONE',  ( 0.9999697198139515519, 0.000000000000000000, 0.007781995580013368816 ) ) ;
#26702 = AXIS2_PLACEMENT_3D ( 'NONE', #39982, #5367, #39145 ) ;
#26703 = LINE ( 'NONE', #44311, #49482 ) ;
#26704 = AXIS2_PLACEMENT_3D ( 'NONE', #51342, #11850, #12455 ) ;
#26705 = EDGE_LOOP ( 'NONE', ( #6361, #8675, #37044, #29086 ) ) ;
#26706 = FACE_OUTER_BOUND ( 'NONE', #28050, .T. ) ;
#26707 = ORIENTED_EDGE ( 'NONE', *, *, #29536, .T. ) ;
#26708 = CARTESIAN_POINT ( 'NONE',  ( -16.81190032086591302, 0.000000000000000000, 3.212244750653343583 ) ) ;
#26709 = VECTOR ( 'NONE', #43807, 999.9999999999998863 ) ;
#26710 = VERTEX_POINT ( 'NONE', #35651 ) ;
#26711 = VECTOR ( 'NONE', #44368, 1000.000000000000114 ) ;
#26712 = EDGE_LOOP ( 'NONE', ( #41598, #55862, #18766, #43146 ) ) ;
#26713 = EDGE_LOOP ( 'NONE', ( #15609, #45351, #18188, #19173, #20345, #29847, #1379, #24457, #4694, #6675, #36048, #26672, #20666, #674, #24079, #50940 ) ) ;
#26714 = PLANE ( 'NONE',  #13021 ) ;
#26715 = FACE_OUTER_BOUND ( 'NONE', #47026, .T. ) ;
#26716 = CARTESIAN_POINT ( 'NONE',  ( -28.93137873341882127, 0.000000000000000000, 8.119251130998824451 ) ) ;
#26717 = LINE ( 'NONE', #53408, #11146 ) ;
#26718 = VERTEX_POINT ( 'NONE', #30577 ) ;
#26719 = EDGE_CURVE ( 'NONE', #44507, #51210, #34810, .T. ) ;
#26720 = ORIENTED_EDGE ( 'NONE', *, *, #43834, .T. ) ;
#26721 = AXIS2_PLACEMENT_3D ( 'NONE', #40555, #36848, #32832 ) ;
#26722 = CARTESIAN_POINT ( 'NONE',  ( -12.60458797795435615, 0.000000000000000000, 11.86609696750642229 ) ) ;
#26723 = VECTOR ( 'NONE', #5708, 1000.000000000000000 ) ;
#26724 = ORIENTED_EDGE ( 'NONE', *, *, #27440, .F. ) ;
#26725 = LINE ( 'NONE', #26436, #12823 ) ;
#26726 = ORIENTED_EDGE ( 'NONE', *, *, #27772, .F. ) ;
#26727 = VECTOR ( 'NONE', #8045, 1000.000000000000114 ) ;
#26728 = DIRECTION ( 'NONE',  ( 0.000000000000000000, -1.000000000000000000, 0.000000000000000000 ) ) ;
#26729 = CARTESIAN_POINT ( 'NONE',  ( -12.70458494993575194, -0.1191753592594197858, 11.86531876794841978 ) ) ;
#26730 = EDGE_CURVE ( 'NONE', #55847, #26836, #27132, .T. ) ;
#26731 = ORIENTED_EDGE ( 'NONE', *, *, #35746, .F. ) ;
#26732 = CARTESIAN_POINT ( 'NONE',  ( -28.92982233430281980, 0.000000000000000000, 7.919257187036034651 ) ) ;
#26733 = VECTOR ( 'NONE', #8518, 999.9999999999998863 ) ;
#26734 = ORIENTED_EDGE ( 'NONE', *, *, #46429, .T. ) ;
#26735 = EDGE_CURVE ( 'NONE', #428, #18282, #47881, .T. ) ;
#26736 = EDGE_CURVE ( 'NONE', #54123, #17188, #35960, .T. ) ;
#26737 = CARTESIAN_POINT ( 'NONE',  ( -22.40634380310664397, 0.000000000000000000, 5.584705972946605534 ) ) ;
#26738 = AXIS2_PLACEMENT_3D ( 'NONE', #6343, #40709, #28767 ) ;
#26739 = VECTOR ( 'NONE', #11096, 1000.000000000000114 ) ;
#26740 = VERTEX_POINT ( 'NONE', #52125 ) ;
#26741 = LINE ( 'NONE', #44601, #24913 ) ;
#26742 = LINE ( 'NONE', #31582, #39362 ) ;
#26743 = AXIS2_PLACEMENT_3D ( 'NONE', #48449, #51853, #34286 ) ;
#26744 = LINE ( 'NONE', #8299, #30115 ) ;
#26745 = ADVANCED_FACE ( 'NONE', ( #13243 ), #4703, .F. ) ;
#26746 = VERTEX_POINT ( 'NONE', #52419 ) ;
#26747 = VECTOR ( 'NONE', #55660, 999.9999999999998863 ) ;
#26748 = CARTESIAN_POINT ( 'NONE',  ( -10.67320487561729969, 0.000000000000000000, 2.521353358429592184 ) ) ;
#26749 = EDGE_CURVE ( 'NONE', #28760, #33629, #4995, .T. ) ;
#26750 = PLANE ( 'NONE',  #50978 ) ;
#26751 = PLANE ( 'NONE',  #33994 ) ;
#26752 = LINE ( 'NONE', #895, #16862 ) ;
#26753 = PLANE ( 'NONE',  #13135 ) ;
#26754 = EDGE_CURVE ( 'NONE', #1987, #18030, #39652, .T. ) ;
#26755 = PLANE ( 'NONE',  #11591 ) ;
#26756 = AXIS2_PLACEMENT_3D ( 'NONE', #19919, #28745, #46052 ) ;
#26757 = AXIS2_PLACEMENT_3D ( 'NONE', #38785, #39328, #12921 ) ;
#26758 = VERTEX_POINT ( 'NONE', #13776 ) ;
#26759 = PLANE ( 'NONE',  #26185 ) ;
#26760 = DIRECTION ( 'NONE',  ( -0.6246952433987893460, -0.7422098413412802076, 0.2426528472758542054 ) ) ;
#26761 = LINE ( 'NONE', #39822, #1484 ) ;
#26762 = EDGE_LOOP ( 'NONE', ( #15845, #50878, #25992, #47094 ) ) ;
#26763 = CARTESIAN_POINT ( 'NONE',  ( -15.82887794256448366, 0.000000000000000000, 8.221217821810743231 ) ) ;
#26764 = FACE_OUTER_BOUND ( 'NONE', #26506, .T. ) ;
#26765 = VERTEX_POINT ( 'NONE', #31101 ) ;
#26766 = ADVANCED_FACE ( 'NONE', ( #48423 ), #44684, .F. ) ;
#26767 = CARTESIAN_POINT ( 'NONE',  ( -1.086233639165236964, 0.000000000000000000, -2.796443541562362078 ) ) ;
#26768 = CARTESIAN_POINT ( 'NONE',  ( -9.808144436391993182, 0.000000000000000000, 10.77986332834118777 ) ) ;
#26769 = DIRECTION ( 'NONE',  ( -0.7660212471507179544, -0.6427876096865405842, -0.005961354470445141482 ) ) ;
#26770 = PLANE ( 'NONE',  #31114 ) ;
#26771 = VECTOR ( 'NONE', #25436, 999.9999999999998863 ) ;
#26772 = EDGE_CURVE ( 'NONE', #49950, #35486, #40456, .T. ) ;
#26773 = ORIENTED_EDGE ( 'NONE', *, *, #17502, .F. ) ;
#26774 = ORIENTED_EDGE ( 'NONE', *, *, #37370, .T. ) ;
#26775 = DIRECTION ( 'NONE',  ( 0.5449076811759707706, 0.6444004775717708799, -0.5364919789714476250 ) ) ;
#26776 = CARTESIAN_POINT ( 'NONE',  ( -19.62132281647664556, -0.1134144341942082690, 4.403214549183394055 ) ) ;
#26777 = CARTESIAN_POINT ( 'NONE',  ( -66.06974441054278202, 2.000000000000016431, 4.495433075559859937 ) ) ;
#26778 = VECTOR ( 'NONE', #9221, 1000.000000000000227 ) ;
#26779 = CARTESIAN_POINT ( 'NONE',  ( -11.13054826722768098, 24.50000000000005684, -3.000000000000000000 ) ) ;
#26780 = DIRECTION ( 'NONE',  ( 0.5364919789714477361, 0.6444004775717706579, 0.5449076811759711036 ) ) ;
#26781 = LINE ( 'NONE', #13998, #3153 ) ;
#26782 = AXIS2_PLACEMENT_3D ( 'NONE', #50756, #12453, #16134 ) ;
#26783 = ORIENTED_EDGE ( 'NONE', *, *, #55222, .T. ) ;
#26784 = LINE ( 'NONE', #48348, #44648 ) ;
#26785 = DIRECTION ( 'NONE',  ( -1.000000000000000000, 0.000000000000000000, -0.000000000000000000 ) ) ;
#26786 = VECTOR ( 'NONE', #44898, 999.9999999999998863 ) ;
#26788 = VERTEX_POINT ( 'NONE', #9503 ) ;
#26787 = VECTOR ( 'NONE', #56225, 999.9999999999998863 ) ;
#26789 = DIRECTION ( 'NONE',  ( -0.6427681459581293666, -0.7660444431189770143, -0.005002170337467561935 ) ) ;
#26790 = DIRECTION ( 'NONE',  ( 0.007781995580012662783, 0.000000000000000000, -0.9999697198139514409 ) ) ;
#26791 = LINE ( 'NONE', #39287, #52033 ) ;
#26792 = AXIS2_PLACEMENT_3D ( 'NONE', #54458, #46220, #7328 ) ;
#26793 = ORIENTED_EDGE ( 'NONE', *, *, #8568, .F. ) ;
#26794 = AXIS2_PLACEMENT_3D ( 'NONE', #3732, #7734, #29875 ) ;
#26795 = CARTESIAN_POINT ( 'NONE',  ( -12.15116108492864377, 0.000000000000000000, 1.401855352044617975 ) ) ;
#26796 = EDGE_CURVE ( 'NONE', #31672, #48670, #1545, .T. ) ;
#26797 = ORIENTED_EDGE ( 'NONE', *, *, #34736, .T. ) ;
#26798 = VECTOR ( 'NONE', #33617, 1000.000000000000227 ) ;
#26799 = VERTEX_POINT ( 'NONE', #5260 ) ;
#26800 = VECTOR ( 'NONE', #21670, 1000.000000000000000 ) ;
#26801 = ORIENTED_EDGE ( 'NONE', *, *, #19657, .F. ) ;
#26802 = ORIENTED_EDGE ( 'NONE', *, *, #47755, .T. ) ;
#26803 = CARTESIAN_POINT ( 'NONE',  ( -68.75329340164451253, -8.572274407770867910, 6.394134653913044808 ) ) ;
#26804 = VERTEX_POINT ( 'NONE', #52935 ) ;
#26805 = CARTESIAN_POINT ( 'NONE',  ( -12.76270579218648571, -2.460819163488157546, 5.678023567659291615 ) ) ;
#26806 = PLANE ( 'NONE',  #21356 ) ;
#26807 = ADVANCED_FACE ( 'NONE', ( #19122 ), #49530, .F. ) ;
#26808 = ORIENTED_EDGE ( 'NONE', *, *, #2447, .F. ) ;
#26809 = CARTESIAN_POINT ( 'NONE',  ( -19.26252944426717306, 0.000000000000000000, 5.778497876809297829 ) ) ;
#26810 = VERTEX_POINT ( 'NONE', #1243 ) ;
#26811 = CARTESIAN_POINT ( 'NONE',  ( -4.243673151615032779, 6.695908571362696016, -1.569986807829671038 ) ) ;
#26812 = ORIENTED_EDGE ( 'NONE', *, *, #45210, .F. ) ;
#26813 = EDGE_CURVE ( 'NONE', #54636, #25808, #27955, .T. ) ;
#26814 = AXIS2_PLACEMENT_3D ( 'NONE', #13087, #51695, #594 ) ;
#26815 = LINE ( 'NONE', #1231, #12867 ) ;
#26816 = CARTESIAN_POINT ( 'NONE',  ( -19.32961685222932147, 0.000000000000000000, 14.39908572644263351 ) ) ;
#26817 = AXIS2_PLACEMENT_3D ( 'NONE', #21332, #26156, #34393 ) ;
#26818 = DIRECTION ( 'NONE',  ( 0.007781995580012663651, -3.146120232559066537E-19, -0.9999697198139514409 ) ) ;
#26819 = LINE ( 'NONE', #45249, #41134 ) ;
#26820 = CARTESIAN_POINT ( 'NONE',  ( -18.12995690313369224, -1.651309408375657428, 6.434302752013834947 ) ) ;
#26821 = PLANE ( 'NONE',  #21077 ) ;
#26822 = VECTOR ( 'NONE', #26078, 999.9999999999998863 ) ;
#26823 = ORIENTED_EDGE ( 'NONE', *, *, #8122, .T. ) ;
#26824 = ORIENTED_EDGE ( 'NONE', *, *, #26173, .F. ) ;
#26825 = EDGE_CURVE ( 'NONE', #52748, #40704, #32828, .T. ) ;
#26826 = PLANE ( 'NONE',  #23752 ) ;
#26827 = DIRECTION ( 'NONE',  ( -0.7660212471507179544, -0.6427876096865405842, -0.005961354470445141482 ) ) ;
#26828 = VECTOR ( 'NONE', #43775, 1000.000000000000227 ) ;
#26829 = ADVANCED_FACE ( 'NONE', ( #40983 ), #35923, .T. ) ;
#26830 = CARTESIAN_POINT ( 'NONE',  ( -14.94916102560700821, 0.000000000000000000, 2.688082935172642962 ) ) ;
#26831 = VECTOR ( 'NONE', #43317, 1000.000000000000227 ) ;
#26832 = CARTESIAN_POINT ( 'NONE',  ( 5.618093201498282063, -1.050357395465043364, -2.260480044901387764 ) ) ;
#26833 = ORIENTED_EDGE ( 'NONE', *, *, #11105, .T. ) ;
#26834 = DIRECTION ( 'NONE',  ( -0.5364919789714478471, 0.6444004775717705469, -0.5449076811759709926 ) ) ;
#26835 = DIRECTION ( 'NONE',  ( 0.007781995580012663651, -3.146120232559066537E-19, -0.9999697198139514409 ) ) ;
#26836 = VERTEX_POINT ( 'NONE', #6109 ) ;
#26837 = CARTESIAN_POINT ( 'NONE',  ( -14.99307481429513622, -0.1191753592594185784, 7.389055067291834256 ) ) ;
#26838 = CARTESIAN_POINT ( 'NONE',  ( -20.13687485811055211, 1.581621852479006440, 7.298878075135696086 ) ) ;
#26839 = VERTEX_POINT ( 'NONE', #1796 ) ;
#26840 = VECTOR ( 'NONE', #16084, 1000.000000000000227 ) ;
#26841 = ADVANCED_FACE ( 'NONE', ( #49228 ), #31374, .F. ) ;
#26842 = CARTESIAN_POINT ( 'NONE',  ( -66.67098249761872353, -8.735215231846519046, 1.683582515887789066 ) ) ;
#26843 = CARTESIAN_POINT ( 'NONE',  ( -13.67407281376373263, 0.000000000000000000, 4.175334245699378499 ) ) ;
#26844 = AXIS2_PLACEMENT_3D ( 'NONE', #53554, #27165, #36253 ) ;
#26845 = AXIS2_PLACEMENT_3D ( 'NONE', #17860, #13844, #27197 ) ;
#26846 = CYLINDRICAL_SURFACE ( 'NONE', #1456, 0.5000000000000004441 ) ;
#26847 = CARTESIAN_POINT ( 'NONE',  ( -16.33317936670417225, 0.000000000000000000, 13.31440848639340224 ) ) ;
#26848 = VECTOR ( 'NONE', #36938, 1000.000000000000000 ) ;
#26849 = FACE_OUTER_BOUND ( 'NONE', #9079, .T. ) ;
#26850 = ORIENTED_EDGE ( 'NONE', *, *, #38165, .F. ) ;
#26851 = VECTOR ( 'NONE', #6447, 999.9999999999998863 ) ;
#26852 = EDGE_LOOP ( 'NONE', ( #30037, #38721, #12243, #51603 ) ) ;
#26853 = DIRECTION ( 'NONE',  ( 0.2426528472758541499, 0.7422098413412800966, 0.6246952433987894571 ) ) ;
#26854 = LINE ( 'NONE', #52667, #42211 ) ;
#26855 = DIRECTION ( 'NONE',  ( 0.007781995580012663651, 0.000000000000000000, -0.9999697198139515519 ) ) ;
#26856 = DIRECTION ( 'NONE',  ( 0.000000000000000000, -1.000000000000000000, 0.000000000000000000 ) ) ;
#26857 = LINE ( 'NONE', #18050, #22175 ) ;
#26858 = EDGE_LOOP ( 'NONE', ( #31697, #13970, #29519, #17423 ) ) ;
#26859 = CARTESIAN_POINT ( 'NONE',  ( -13.04051704107165399, 25.12932982184632635, -3.513244100307224116 ) ) ;
#26860 = DIRECTION ( 'NONE',  ( 0.005002170337468016433, -0.7660444431189770143, -0.6427681459581293666 ) ) ;
#26861 = VECTOR ( 'NONE', #15059, 999.9999999999998863 ) ;
#26862 = LINE ( 'NONE', #39909, #1475 ) ;
#26863 = DIRECTION ( 'NONE',  ( 0.007781995580012663651, -3.146120232559066537E-19, -0.9999697198139514409 ) ) ;
#26864 = VERTEX_POINT ( 'NONE', #36446 ) ;
#26865 = DIRECTION ( 'NONE',  ( 0.6427681459581294776, -0.7660444431189769032, 0.005002170337467562802 ) ) ;
#26866 = ORIENTED_EDGE ( 'NONE', *, *, #41610, .T. ) ;
#26867 = CARTESIAN_POINT ( 'NONE',  ( -11.25506635995362359, -1.813211359398158029, 1.195320179481486722 ) ) ;
#26868 = AXIS2_PLACEMENT_3D ( 'NONE', #28495, #2378, #53502 ) ;
#26869 = EDGE_CURVE ( 'NONE', #49537, #53352, #14595, .T. ) ;
#26870 = LINE ( 'NONE', #49274, #16644 ) ;
#26871 = EDGE_LOOP ( 'NONE', ( #4427, #17825, #35251, #30529 ) ) ;
#26872 = PLANE ( 'NONE',  #17237 ) ;
#26873 = VECTOR ( 'NONE', #33197, 1000.000000000000000 ) ;
#26874 = ADVANCED_FACE ( 'NONE', ( #23409 ), #26826, .F. ) ;
#26875 = ORIENTED_EDGE ( 'NONE', *, *, #10192, .T. ) ;
#26876 = ORIENTED_EDGE ( 'NONE', *, *, #47928, .F. ) ;
#26877 = VECTOR ( 'NONE', #13616, 1000.000000000000227 ) ;
#26878 = EDGE_LOOP ( 'NONE', ( #28769, #4066, #8999, #15220, #55223, #35442 ) ) ;
#26879 = CARTESIAN_POINT ( 'NONE',  ( -27.99923088623136636, 0.000000000000000000, 7.757173251277078130 ) ) ;
#26880 = VECTOR ( 'NONE', #25285, 1000.000000000000000 ) ;
#26881 = EDGE_LOOP ( 'NONE', ( #19786, #17671, #39751, #40429 ) ) ;
#26882 = EDGE_CURVE ( 'NONE', #3963, #28164, #10648, .T. ) ;
#26883 = ORIENTED_EDGE ( 'NONE', *, *, #9607, .T. ) ;
#26884 = DIRECTION ( 'NONE',  ( 0.000000000000000000, -1.000000000000000000, 0.000000000000000000 ) ) ;
#26885 = CARTESIAN_POINT ( 'NONE',  ( -11.40636015113596180, 0.000000000000000000, 11.32142374880780089 ) ) ;
#26887 = EDGE_CURVE ( 'NONE', #49177, #32990, #53248, .T. ) ;
#26886 = ORIENTED_EDGE ( 'NONE', *, *, #9159, .T. ) ;
#26888 = VECTOR ( 'NONE', #37083, 1000.000000000000114 ) ;
#26889 = EDGE_CURVE ( 'NONE', #22744, #17816, #5805, .T. ) ;
#26890 = ADVANCED_FACE ( 'NONE', ( #9801 ), #5513, .F. ) ;
#26891 = VECTOR ( 'NONE', #29631, 999.9999999999998863 ) ;
#26892 = VERTEX_POINT ( 'NONE', #23127 ) ;
#26893 = LINE ( 'NONE', #23189, #18586 ) ;
#26894 = VERTEX_POINT ( 'NONE', #36192 ) ;
#26895 = ORIENTED_EDGE ( 'NONE', *, *, #39444, .T. ) ;
#26896 = AXIS2_PLACEMENT_3D ( 'NONE', #9701, #43225, #4323 ) ;
#26897 = AXIS2_PLACEMENT_3D ( 'NONE', #4370, #59, #22233 ) ;
#26898 = FACE_OUTER_BOUND ( 'NONE', #26688, .T. ) ;
#26899 = FACE_OUTER_BOUND ( 'NONE', #26003, .T. ) ;
#26900 = LINE ( 'NONE', #1308, #20507 ) ;
#26901 = DIRECTION ( 'NONE',  ( 0.007781995580012662783, 0.000000000000000000, -0.9999697198139514409 ) ) ;
#26902 = EDGE_LOOP ( 'NONE', ( #15982, #5687, #11117, #17161 ) ) ;
#26903 = CARTESIAN_POINT ( 'NONE',  ( -6.110905869600904872, 1.712176620043476140E-14, 3.600000000000000089 ) ) ;
#26904 = ORIENTED_EDGE ( 'NONE', *, *, #49772, .T. ) ;
#26905 = EDGE_CURVE ( 'NONE', #34917, #2726, #53495, .T. ) ;
#26906 = FACE_OUTER_BOUND ( 'NONE', #28764, .T. ) ;
#26907 = VECTOR ( 'NONE', #51946, 999.9999999999998863 ) ;
#26908 = ADVANCED_FACE ( 'NONE', ( #11726 ), #32737, .F. ) ;
#26909 = CARTESIAN_POINT ( 'NONE',  ( -12.13851405436063047, 0.000000000000000000, 11.68505802764555135 ) ) ;
#26910 = CARTESIAN_POINT ( 'NONE',  ( -18.67619601524082285, 0.000000000000000000, 3.936400510096834893 ) ) ;
#26911 = CARTESIAN_POINT ( 'NONE',  ( -14.42424669531936132, -3.917936722690662954, 2.359185689018677312 ) ) ;
#26912 = LINE ( 'NONE', #2071, #43048 ) ;
#26913 = EDGE_CURVE ( 'NONE', #1004, #37960, #20804, .T. ) ;
#26914 = LINE ( 'NONE', #30033, #10329 ) ;
#26915 = DIRECTION ( 'NONE',  ( 0.007781995580012663651, -3.146120232559066537E-19, -0.9999697198139514409 ) ) ;
#26916 = ORIENTED_EDGE ( 'NONE', *, *, #30039, .F. ) ;
#26917 = PLANE ( 'NONE',  #1153 ) ;
#26918 = VECTOR ( 'NONE', #46036, 999.9999999999998863 ) ;
#26919 = ADVANCED_FACE ( 'NONE', ( #2901, #50633, #38121 ), #55172, .T. ) ;
#26920 = CARTESIAN_POINT ( 'NONE',  ( -19.08265387484136255, 0.000000000000000000, 8.365222198729652447 ) ) ;
#26921 = LINE ( 'NONE', #8766, #605 ) ;
#26923 = DIRECTION ( 'NONE',  ( -0.5364919789714478471, 0.6444004775717705469, -0.5449076811759709926 ) ) ;
#26922 = AXIS2_PLACEMENT_3D ( 'NONE', #28592, #16354, #25444 ) ;
#26924 = CARTESIAN_POINT ( 'NONE',  ( -28.40705682302959900, 14.52540313465091160, -4.730581911476714474 ) ) ;
#26925 = CARTESIAN_POINT ( 'NONE',  ( -13.43961370871902972, -4.889348428825662118, 9.926587849587082957 ) ) ;
#26926 = ADVANCED_FACE ( 'NONE', ( #46643 ), #7194, .F. ) ;
#26927 = CARTESIAN_POINT ( 'NONE',  ( -17.26532721389163072, 0.000000000000000000, 13.67648636611514590 ) ) ;
#26928 = VECTOR ( 'NONE', #43108, 1000.000000000000000 ) ;
#26929 = PLANE ( 'NONE',  #12105 ) ;
#26930 = ORIENTED_EDGE ( 'NONE', *, *, #23360, .T. ) ;
#26931 = LINE ( 'NONE', #18682, #47464 ) ;
#26932 = CARTESIAN_POINT ( 'NONE',  ( 2.072287782118878319, 0.000000000000000000, -2.950529333540147015 ) ) ;
#26933 = LINE ( 'NONE', #35182, #10073 ) ;
#26934 = VECTOR ( 'NONE', #7600, 1000.000000000000114 ) ;
#26935 = CARTESIAN_POINT ( 'NONE',  ( -56.02165185617580079, 5.343604887189308705, -3.000000000000007105 ) ) ;
#26936 = PLANE ( 'NONE',  #42105 ) ;
#26937 = LINE ( 'NONE', #4772, #12339 ) ;
#26938 = CARTESIAN_POINT ( 'NONE',  ( -56.75000000000000711, 6.050000000000001599, -2.449489742783172108 ) ) ;
#26939 = VECTOR ( 'NONE', #49646, 1000.000000000000227 ) ;
#26940 = AXIS2_PLACEMENT_3D ( 'NONE', #33815, #6578, #23894 ) ;
#26941 = CARTESIAN_POINT ( 'NONE',  ( -66.78432981023388493, -9.486898575435347425, 0.6700356180039961362 ) ) ;
#26942 = DIRECTION ( 'NONE',  ( 0.007781995580012663651, 0.000000000000000000, -0.9999697198139515519 ) ) ;
#26943 = ORIENTED_EDGE ( 'NONE', *, *, #51670, .T. ) ;
#26944 = VECTOR ( 'NONE', #4871, 999.9999999999998863 ) ;
#26945 = EDGE_LOOP ( 'NONE', ( #19462, #13522, #4069, #37539 ) ) ;
#26946 = ORIENTED_EDGE ( 'NONE', *, *, #29681, .T. ) ;
#26947 = ORIENTED_EDGE ( 'NONE', *, *, #54240, .T. ) ;
#26948 = ORIENTED_EDGE ( 'NONE', *, *, #1241, .T. ) ;
#26949 = CARTESIAN_POINT ( 'NONE',  ( -17.47589215640082827, 2.876837460659009693, 3.378375551940059562 ) ) ;
#26950 = LINE ( 'NONE', #51918, #41215 ) ;
#26951 = EDGE_CURVE ( 'NONE', #37046, #23668, #20230, .T. ) ;
#26952 = EDGE_CURVE ( 'NONE', #49895, #54809, #33329, .T. ) ;
#26953 = VERTEX_POINT ( 'NONE', #16261 ) ;
#26954 = VECTOR ( 'NONE', #8337, 1000.000000000000114 ) ;
#26955 = ORIENTED_EDGE ( 'NONE', *, *, #33091, .T. ) ;
#26956 = EDGE_CURVE ( 'NONE', #15321, #35294, #24243, .T. ) ;
#26957 = AXIS2_PLACEMENT_3D ( 'NONE', #1563, #31391, #48711 ) ;
#26958 = CARTESIAN_POINT ( 'NONE',  ( -66.57070431223807816, -9.328541353163785743, -6.245432549306846326 ) ) ;
#26959 = ORIENTED_EDGE ( 'NONE', *, *, #45115, .T. ) ;
#26960 = DIRECTION ( 'NONE',  ( -0.5364919789714478471, 0.6444004775717705469, -0.5449076811759709926 ) ) ;
#26961 = FACE_OUTER_BOUND ( 'NONE', #6495, .T. ) ;
#26962 = ORIENTED_EDGE ( 'NONE', *, *, #5208, .T. ) ;
#26963 = CARTESIAN_POINT ( 'NONE',  ( 2.072287782118878319, 0.000000000000000000, -2.950529333540147015 ) ) ;
#26964 = ORIENTED_EDGE ( 'NONE', *, *, #20901, .T. ) ;
#26965 = VECTOR ( 'NONE', #11164, 1000.000000000000000 ) ;
#26966 = FACE_OUTER_BOUND ( 'NONE', #41771, .T. ) ;
#26967 = CARTESIAN_POINT ( 'NONE',  ( -27.99923088623136636, 0.000000000000000000, 7.757173251277078130 ) ) ;
#26968 = FACE_OUTER_BOUND ( 'NONE', #5028, .T. ) ;
#26969 = DIRECTION ( 'NONE',  ( 0.005961354470445682716, -0.6427876096865404731, -0.7660212471507180654 ) ) ;
#26970 = ORIENTED_EDGE ( 'NONE', *, *, #26055, .F. ) ;
#26971 = DIRECTION ( 'NONE',  ( 0.7660212471507180654, -0.6427876096865404731, 0.005961354470445141482 ) ) ;
#26972 = CARTESIAN_POINT ( 'NONE',  ( -6.520961821973863870, -6.264410134614024628, -0.6854105512135232336 ) ) ;
#26973 = PLANE ( 'NONE',  #15749 ) ;
#26974 = VERTEX_POINT ( 'NONE', #50047 ) ;
#26975 = FACE_OUTER_BOUND ( 'NONE', #50993, .T. ) ;
#26976 = ORIENTED_EDGE ( 'NONE', *, *, #47442, .F. ) ;
#26977 = EDGE_CURVE ( 'NONE', #48888, #35555, #46345, .T. ) ;
#26978 = DIRECTION ( 'NONE',  ( 0.9999697198139515519, 0.000000000000000000, 0.007781995580013368816 ) ) ;
#26979 = DIRECTION ( 'NONE',  ( -0.7660212471507179544, -0.6427876096865405842, -0.005961354470445141482 ) ) ;
#26980 = DIRECTION ( 'NONE',  ( 0.007781995580012662783, 0.000000000000000000, -0.9999697198139514409 ) ) ;
#26981 = CARTESIAN_POINT ( 'NONE',  ( -17.49357527494113285, 0.1245042932765033361, 3.880752594646831533 ) ) ;
#26982 = CARTESIAN_POINT ( 'NONE',  ( -19.72141823409769046, 0.000000000000000000, 5.036262558525757882 ) ) ;
#26983 = ADVANCED_FACE ( 'NONE', ( #41811 ), #3206, .F. ) ;
#26984 = DIRECTION ( 'NONE',  ( 0.000000000000000000, -1.000000000000000000, 0.000000000000000000 ) ) ;
#26985 = PLANE ( 'NONE',  #23436 ) ;
#26986 = LINE ( 'NONE', #1941, #17553 ) ;
#26987 = EDGE_CURVE ( 'NONE', #15529, #9986, #28485, .T. ) ;
#26988 = LINE ( 'NONE', #30406, #47747 ) ;
#26989 = ORIENTED_EDGE ( 'NONE', *, *, #7444, .T. ) ;
#26990 = PLANE ( 'NONE',  #28445 ) ;
#26991 = CARTESIAN_POINT ( 'NONE',  ( -11.30636317915456779, -0.1191753592594197858, 11.32220194836580340 ) ) ;
#26993 = EDGE_CURVE ( 'NONE', #50717, #20913, #34858, .T. ) ;
#26992 = CARTESIAN_POINT ( 'NONE',  ( -14.15595403163651866, 0.000000000000000000, 6.387576553477955166 ) ) ;
#26994 = DIRECTION ( 'NONE',  ( 0.6246952433987894571, -0.7422098413412800966, -0.2426528472758541777 ) ) ;
#26995 = EDGE_CURVE ( 'NONE', #4182, #24424, #41276, .T. ) ;
#26996 = DIRECTION ( 'NONE',  ( 0.6427681459581294776, -0.7660444431189769032, 0.005002170337467562802 ) ) ;
#26997 = FACE_OUTER_BOUND ( 'NONE', #28604, .T. ) ;
#26998 = CARTESIAN_POINT ( 'NONE',  ( -23.33849165029409889, 0.000000000000000000, 5.946783852668351855 ) ) ;
#26999 = EDGE_LOOP ( 'NONE', ( #48206, #51849, #48003, #41916 ) ) ;
#27000 = VECTOR ( 'NONE', #26855, 999.9999999999998863 ) ;
#27001 = ORIENTED_EDGE ( 'NONE', *, *, #52916, .T. ) ;
#27002 = DIRECTION ( 'NONE',  ( -0.7660212471507179544, -0.6427876096865405842, -0.005961354470445141482 ) ) ;
#27003 = FACE_OUTER_BOUND ( 'NONE', #44288, .T. ) ;
#27004 = VECTOR ( 'NONE', #55661, 1000.000000000000227 ) ;
#27005 = VERTEX_POINT ( 'NONE', #19959 ) ;
#27006 = PLANE ( 'NONE',  #48520 ) ;
#27007 = ORIENTED_EDGE ( 'NONE', *, *, #19321, .T. ) ;
#27008 = LINE ( 'NONE', #44316, #41964 ) ;
#27009 = EDGE_LOOP ( 'NONE', ( #21610, #51834, #8650, #41581 ) ) ;
#27010 = ORIENTED_EDGE ( 'NONE', *, *, #26045, .F. ) ;
#27011 = VERTEX_POINT ( 'NONE', #54580 ) ;
#27012 = DIRECTION ( 'NONE',  ( -0.000000000000000000, -0.000000000000000000, 1.000000000000000000 ) ) ;
#27013 = CARTESIAN_POINT ( 'NONE',  ( 2.072287782118878319, 0.000000000000000000, -2.950529333540147015 ) ) ;
#27014 = LINE ( 'NONE', #9396, #23020 ) ;
#27015 = ADVANCED_FACE ( 'NONE', ( #15692 ), #33030, .F. ) ;
#27016 = DIRECTION ( 'NONE',  ( 0.005002170337468016433, -0.7660444431189770143, -0.6427681459581293666 ) ) ;
#27017 = VERTEX_POINT ( 'NONE', #26452 ) ;
#27018 = ORIENTED_EDGE ( 'NONE', *, *, #50534, .T. ) ;
#27019 = EDGE_CURVE ( 'NONE', #41786, #44220, #26200, .T. ) ;
#27020 = ADVANCED_FACE ( 'NONE', ( #22215 ), #39242, .F. ) ;
#27021 = DIRECTION ( 'NONE',  ( -0.5364919789714478471, 0.6444004775717705469, -0.5449076811759709926 ) ) ;
#27022 = ORIENTED_EDGE ( 'NONE', *, *, #4284, .F. ) ;
#27023 = FACE_OUTER_BOUND ( 'NONE', #11130, .T. ) ;
#27024 = ORIENTED_EDGE ( 'NONE', *, *, #46929, .T. ) ;
#27025 = LINE ( 'NONE', #31272, #9722 ) ;
#27026 = CARTESIAN_POINT ( 'NONE',  ( -21.47341775636118655, -0.1191753592594197858, 5.122631121243466090 ) ) ;
#27027 = VERTEX_POINT ( 'NONE', #30744 ) ;
#27028 = DIRECTION ( 'NONE',  ( 0.007781995580012663651, 0.000000000000000000, -0.9999697198139515519 ) ) ;
#27029 = VERTEX_POINT ( 'NONE', #29637 ) ;
#27030 = EDGE_CURVE ( 'NONE', #51526, #31162, #13137, .T. ) ;
#27031 = FACE_OUTER_BOUND ( 'NONE', #11785, .T. ) ;
#27032 = ORIENTED_EDGE ( 'NONE', *, *, #31807, .F. ) ;
#27033 = LINE ( 'NONE', #53162, #18596 ) ;
#27034 = LINE ( 'NONE', #44343, #50162 ) ;
#27035 = DIRECTION ( 'NONE',  ( 0.007781995580012663651, -3.146120232559066537E-19, -0.9999697198139514409 ) ) ;
#27036 = EDGE_LOOP ( 'NONE', ( #18559, #7370, #42164 ) ) ;
#27037 = VECTOR ( 'NONE', #17766, 999.9999999999998863 ) ;
#27038 = CARTESIAN_POINT ( 'NONE',  ( -34.64355613791357769, -1.000000000000000000, 10.23836012842048326 ) ) ;
#27039 = CARTESIAN_POINT ( 'NONE',  ( -68.86860983449916773, 1.667510478463746004, 7.477472888882761737 ) ) ;
#27040 = CARTESIAN_POINT ( 'NONE',  ( -56.40918267430362221, 3.913378331250040087, -2.245061400351528569 ) ) ;
#27041 = EDGE_CURVE ( 'NONE', #27886, #48678, #17674, .T. ) ;
#27042 = DIRECTION ( 'NONE',  ( 0.007781995580012662783, 0.000000000000000000, -0.9999697198139514409 ) ) ;
#27043 = LINE ( 'NONE', #10273, #1625 ) ;
#27044 = CARTESIAN_POINT ( 'NONE',  ( -67.40686789321162564, -11.43753496933752167, 4.727715060443837380 ) ) ;
#27045 = ORIENTED_EDGE ( 'NONE', *, *, #33116, .F. ) ;
#27046 = PLANE ( 'NONE',  #36166 ) ;
#27047 = DIRECTION ( 'NONE',  ( 0.005002170337468016433, -0.7660444431189770143, -0.6427681459581293666 ) ) ;
#27048 = LINE ( 'NONE', #17685, #19648 ) ;
#27049 = ORIENTED_EDGE ( 'NONE', *, *, #22595, .F. ) ;
#27050 = DIRECTION ( 'NONE',  ( 0.005002170337468016433, -0.7660444431189770143, -0.6427681459581293666 ) ) ;
#27051 = PLANE ( 'NONE',  #5488 ) ;
#27052 = ORIENTED_EDGE ( 'NONE', *, *, #22906, .T. ) ;
#27053 = CARTESIAN_POINT ( 'NONE',  ( -15.60102546347950536, 0.000000000000000000, 12.95077420755565356 ) ) ;
#27054 = EDGE_CURVE ( 'NONE', #27257, #29102, #30169, .T. ) ;
#27055 = FACE_OUTER_BOUND ( 'NONE', #39135, .T. ) ;
#27056 = CARTESIAN_POINT ( 'NONE',  ( -12.56336705153974620, 0.000000000000000000, 6.569296447192962241 ) ) ;
#27057 = DIRECTION ( 'NONE',  ( 0.007781995580012662783, 0.000000000000000000, -0.9999697198139514409 ) ) ;
#27058 = EDGE_LOOP ( 'NONE', ( #14614, #1285, #24818, #19441 ) ) ;
#27059 = ORIENTED_EDGE ( 'NONE', *, *, #18551, .F. ) ;
#27060 = LINE ( 'NONE', #35871, #4954 ) ;
#27061 = DIRECTION ( 'NONE',  ( 0.5364919789714477361, 0.6444004775717706579, 0.5449076811759711036 ) ) ;
#27062 = PLANE ( 'NONE',  #11584 ) ;
#27063 = ADVANCED_FACE ( 'NONE', ( #8044 ), #12581, .F. ) ;
#27064 = CARTESIAN_POINT ( 'NONE',  ( -15.87975247367846166, 0.000000000000000000, 2.850166870931599927 ) ) ;
#27065 = LINE ( 'NONE', #39841, #3796 ) ;
#27066 = DIRECTION ( 'NONE',  ( -0.5364919789714478471, 0.6444004775717705469, -0.5449076811759709926 ) ) ;
#27068 = ADVANCED_FACE ( 'NONE', ( #46943 ), #52324, .F. ) ;
#27067 = ORIENTED_EDGE ( 'NONE', *, *, #49750, .T. ) ;
#27069 = FACE_OUTER_BOUND ( 'NONE', #25876, .T. ) ;
#27070 = EDGE_CURVE ( 'NONE', #51439, #26046, #48045, .T. ) ;
#27071 = CARTESIAN_POINT ( 'NONE',  ( 4.994031378522667985, 0.000000000000000000, 2.289010529401726668 ) ) ;
#27072 = EDGE_LOOP ( 'NONE', ( #23977, #41727, #12271, #2025 ) ) ;
#27073 = CARTESIAN_POINT ( 'NONE',  ( -12.15271748404464880, 0.000000000000000000, 1.601849296007406664 ) ) ;
#27074 = EDGE_CURVE ( 'NONE', #25250, #47436, #4052, .T. ) ;
#27075 = PLANE ( 'NONE',  #16830 ) ;
#27076 = CARTESIAN_POINT ( 'NONE',  ( -9.542064456761055524, 0.000000000000000000, 10.59726798936431180 ) ) ;
#27077 = ORIENTED_EDGE ( 'NONE', *, *, #30532, .F. ) ;
#27078 = VECTOR ( 'NONE', #23061, 1000.000000000000227 ) ;
#27079 = LINE ( 'NONE', #48081, #34846 ) ;
#27080 = ADVANCED_FACE ( 'NONE', ( #51189 ), #21380, .T. ) ;
#27081 = ORIENTED_EDGE ( 'NONE', *, *, #34188, .F. ) ;
#27082 = EDGE_CURVE ( 'NONE', #24756, #13654, #43772, .T. ) ;
#27083 = ORIENTED_EDGE ( 'NONE', *, *, #4499, .T. ) ;
#27084 = ORIENTED_EDGE ( 'NONE', *, *, #15511, .F. ) ;
#27085 = EDGE_LOOP ( 'NONE', ( #55900, #3365, #17301, #12035 ) ) ;
#27086 = CARTESIAN_POINT ( 'NONE',  ( -18.24840714568802014, -0.1191753592594162470, 7.733053388173527942 ) ) ;
#27087 = ORIENTED_EDGE ( 'NONE', *, *, #11789, .F. ) ;
#27088 = CARTESIAN_POINT ( 'NONE',  ( -14.16457619215236541, 0.000000000000000000, 7.495505663251248230 ) ) ;
#27089 = CARTESIAN_POINT ( 'NONE',  ( -16.33317936670417225, 0.000000000000000000, 13.31440848639340224 ) ) ;
#27090 = EDGE_CURVE ( 'NONE', #37629, #1446, #47486, .T. ) ;
#27091 = ORIENTED_EDGE ( 'NONE', *, *, #48033, .T. ) ;
#27092 = CARTESIAN_POINT ( 'NONE',  ( -14.46888367232926420, 0.000000000000000000, 12.59025272694991315 ) ) ;
#27093 = ORIENTED_EDGE ( 'NONE', *, *, #12165, .F. ) ;
#27094 = LINE ( 'NONE', #44399, #23193 ) ;
#27095 = ORIENTED_EDGE ( 'NONE', *, *, #21807, .T. ) ;
#27096 = ADVANCED_FACE ( 'NONE', ( #21916 ), #8599, .F. ) ;
#27097 = CARTESIAN_POINT ( 'NONE',  ( -11.88054826722768276, 25.79903810567671130, 3.000000000000000888 ) ) ;
#27098 = LINE ( 'NONE', #26816, #285 ) ;
#27099 = LINE ( 'NONE', #18277, #562 ) ;
#27100 = LINE ( 'NONE', #27660, #37477 ) ;
#27101 = CARTESIAN_POINT ( 'NONE',  ( -13.07066190154808361, 0.000000000000000000, 12.04713590736729678 ) ) ;
#27102 =( NAMED_UNIT ( * ) SI_UNIT ( $, .STERADIAN. ) SOLID_ANGLE_UNIT ( ) );
#27103 = VERTEX_POINT ( 'NONE', #4354 ) ;
#27104 = VERTEX_POINT ( 'NONE', #29898 ) ;
#27105 = CARTESIAN_POINT ( 'NONE',  ( -16.79925329029790149, 0.000000000000000000, 13.49544742625427496 ) ) ;
#27106 = LINE ( 'NONE', #6110, #24868 ) ;
#27107 = CARTESIAN_POINT ( 'NONE',  ( -22.36868959911851462, 19.74370688441071309, -4.657437592157546824 ) ) ;
#27108 = DIRECTION ( 'NONE',  ( -0.5364919789714478471, 0.6444004775717705469, -0.5449076811759709926 ) ) ;
#27109 = ORIENTED_EDGE ( 'NONE', *, *, #6314, .T. ) ;
#27110 = FACE_OUTER_BOUND ( 'NONE', #11756, .T. ) ;
#27111 = CARTESIAN_POINT ( 'NONE',  ( -70.08024661842391367, -0.7499901437495212209, -7.503442492476274595 ) ) ;
#27112 = VERTEX_POINT ( 'NONE', #40 ) ;
#27113 = CARTESIAN_POINT ( 'NONE',  ( -21.06965149344186372, 20.49370688441071664, -4.657437592157546824 ) ) ;
#27114 = DIRECTION ( 'NONE',  ( -0.7660212471507179544, -0.6427876096865405842, -0.005961354470445141482 ) ) ;
#27115 = EDGE_LOOP ( 'NONE', ( #4799, #44517, #14775, #6383 ) ) ;
#27116 = AXIS2_PLACEMENT_3D ( 'NONE', #7142, #55376, #15935 ) ;
#27117 = CARTESIAN_POINT ( 'NONE',  ( -66.66796270868890417, -8.734742092342063557, -1.671631898859750720 ) ) ;
#27118 = FACE_OUTER_BOUND ( 'NONE', #16025, .T. ) ;
#27119 = ADVANCED_FACE ( 'NONE', ( #21662 ), #25620, .F. ) ;
#27120 = DIRECTION ( 'NONE',  ( -0.9321478471874540261, 0.000000000000000000, 0.3620778797217457656 ) ) ;
#27121 = CARTESIAN_POINT ( 'NONE',  ( -14.13870971060482162, 0.000000000000000000, 4.171718333931368150 ) ) ;
#27122 = DIRECTION ( 'NONE',  ( 0.005002170337468016433, -0.7660444431189770143, -0.6427681459581293666 ) ) ;
#27123 = VERTEX_POINT ( 'NONE', #56026 ) ;
#27124 = ORIENTED_EDGE ( 'NONE', *, *, #29442, .F. ) ;
#27125 = DIRECTION ( 'NONE',  ( 0.5449076811759707706, 0.6444004775717708799, -0.5364919789714476250 ) ) ;
#27126 = PLANE ( 'NONE',  #25892 ) ;
#27127 = CARTESIAN_POINT ( 'NONE',  ( 3.004435629306332345, -1.000000000000000000, -3.312607213261892003 ) ) ;
#27128 = EDGE_CURVE ( 'NONE', #24033, #39633, #34429, .T. ) ;
#27129 = PLANE ( 'NONE',  #3753 ) ;
#27130 = DIRECTION ( 'NONE',  ( 0.007781995580012663651, 0.000000000000000000, -0.9999697198139515519 ) ) ;
#27131 = EDGE_LOOP ( 'NONE', ( #38545, #3259, #6983, #21314 ) ) ;
#27132 = LINE ( 'NONE', #35371, #13739 ) ;
#27133 = DIRECTION ( 'NONE',  ( 0.000000000000000000, -0.000000000000000000, -1.000000000000000000 ) ) ;
#27134 = ADVANCED_FACE ( 'NONE', ( #19055 ), #36130, .F. ) ;
#27135 = CARTESIAN_POINT ( 'NONE',  ( -16.79925329029790149, 0.000000000000000000, 13.49544742625427496 ) ) ;
#27136 = DIRECTION ( 'NONE',  ( 0.7660212471507180654, -0.6427876096865404731, 0.005961354470445141482 ) ) ;
#27137 = ORIENTED_EDGE ( 'NONE', *, *, #35281, .F. ) ;
#27138 = CARTESIAN_POINT ( 'NONE',  ( -17.35017059011151375, 1.553641160433663071, 12.97584759397192045 ) ) ;
#27139 = ORIENTED_EDGE ( 'NONE', *, *, #22600, .T. ) ;
#27140 = CARTESIAN_POINT ( 'NONE',  ( -14.93495759592298988, 0.000000000000000000, 12.77129166681078409 ) ) ;
#27141 = PLANE ( 'NONE',  #45657 ) ;
#27142 = ORIENTED_EDGE ( 'NONE', *, *, #26404, .T. ) ;
#27143 = CARTESIAN_POINT ( 'NONE',  ( -10.27421835998572064, 0.000000000000000000, 10.96090226820206048 ) ) ;
#27144 = EDGE_CURVE ( 'NONE', #55458, #35036, #53167, .T. ) ;
#27145 = ORIENTED_EDGE ( 'NONE', *, *, #39608, .T. ) ;
#27146 = ADVANCED_FACE ( 'NONE', ( #35544 ), #31292, .F. ) ;
#27147 = VERTEX_POINT ( 'NONE', #27589 ) ;
#27148 = VERTEX_POINT ( 'NONE', #49154 ) ;
#27149 = LINE ( 'NONE', #27997, #22129 ) ;
#27150 = VERTEX_POINT ( 'NONE', #14526 ) ;
#27151 = ORIENTED_EDGE ( 'NONE', *, *, #37079, .F. ) ;
#27152 = LINE ( 'NONE', #45050, #30220 ) ;
#27153 = CARTESIAN_POINT ( 'NONE',  ( -20.64507249176656956, 4.981562823951512620, 4.542241061477253261 ) ) ;
#27154 = ORIENTED_EDGE ( 'NONE', *, *, #1320, .T. ) ;
#27155 = EDGE_CURVE ( 'NONE', #17736, #52910, #5447, .T. ) ;
#27156 =( GEOMETRIC_REPRESENTATION_CONTEXT ( 3 ) GLOBAL_UNCERTAINTY_ASSIGNED_CONTEXT ( ( #16612 ) ) GLOBAL_UNIT_ASSIGNED_CONTEXT ( ( #49682, #28086, #15309 ) ) REPRESENTATION_CONTEXT ( 'NONE', 'WORKASPACE' ) );
#27157 = ORIENTED_EDGE ( 'NONE', *, *, #12410, .T. ) ;
#27158 = LINE ( 'NONE', #52699, #11322 ) ;
#27159 = ORIENTED_EDGE ( 'NONE', *, *, #10177, .T. ) ;
#27160 = ORIENTED_EDGE ( 'NONE', *, *, #17206, .T. ) ;
#27161 = ADVANCED_FACE ( 'NONE', ( #22761 ), #39814, .T. ) ;
#27162 = CARTESIAN_POINT ( 'NONE',  ( -9.808144436391993182, 0.000000000000000000, 10.77986332834118777 ) ) ;
#27163 = PLANE ( 'NONE',  #49343 ) ;
#27164 = LINE ( 'NONE', #10704, #18737 ) ;
#27165 = DIRECTION ( 'NONE',  ( -0.005961354470445682716, -0.6427876096865404731, 0.7660212471507180654 ) ) ;
#27166 = ORIENTED_EDGE ( 'NONE', *, *, #47901, .F. ) ;
#27167 = LINE ( 'NONE', #9579, #11060 ) ;
#27168 = ORIENTED_EDGE ( 'NONE', *, *, #15461, .T. ) ;
#27169 = DIRECTION ( 'NONE',  ( 0.9932609354084158682, 0.1139014070068027212, 0.02142857142857160571 ) ) ;
#27170 = FACE_OUTER_BOUND ( 'NONE', #44257, .T. ) ;
#27171 = DIRECTION ( 'NONE',  ( 0.9999697198139515519, 0.000000000000000000, 0.007781995580013368816 ) ) ;
#27172 = CARTESIAN_POINT ( 'NONE',  ( 4.854282358214434545, 0.000000000000000000, 1.997863978257570228 ) ) ;
#27173 = LINE ( 'NONE', #10715, #22115 ) ;
#27174 = CARTESIAN_POINT ( 'NONE',  ( -14.59472444693005500, 0.000000000000000000, 3.060173312390066513 ) ) ;
#27175 = ORIENTED_EDGE ( 'NONE', *, *, #32043, .T. ) ;
#27176 = LINE ( 'NONE', #48777, #45587 ) ;
#27177 = ORIENTED_EDGE ( 'NONE', *, *, #52393, .T. ) ;
#27178 = PLANE ( 'NONE',  #35594 ) ;
#27179 = CARTESIAN_POINT ( 'NONE',  ( -15.13495153988577968, 0.000000000000000000, 12.76973526769478084 ) ) ;
#27180 = LINE ( 'NONE', #44781, #5452 ) ;
#27181 = EDGE_CURVE ( 'NONE', #31243, #52679, #52853, .T. ) ;
#27182 = CARTESIAN_POINT ( 'NONE',  ( -28.38032086473889137, 14.54083914736709993, -4.729686555805564296 ) ) ;
#27183 = LINE ( 'NONE', #26925, #12283 ) ;
#27184 = CARTESIAN_POINT ( 'NONE',  ( 2.072287782118878319, 0.000000000000000000, -2.950529333540147015 ) ) ;
#27185 = FACE_OUTER_BOUND ( 'NONE', #7286, .T. ) ;
#27186 = EDGE_CURVE ( 'NONE', #42836, #40959, #53690, .T. ) ;
#27187 = ORIENTED_EDGE ( 'NONE', *, *, #50667, .T. ) ;
#27188 = EDGE_CURVE ( 'NONE', #13585, #8019, #40078, .T. ) ;
#27189 = CARTESIAN_POINT ( 'NONE',  ( -11.20636620717317378, 0.000000000000000000, 11.32298014792380414 ) ) ;
#27190 = CARTESIAN_POINT ( 'NONE',  ( -8.446367469219440594, -0.08969168290429911650, 5.248751129891273237 ) ) ;
#27191 = CARTESIAN_POINT ( 'NONE',  ( -18.29325764774754859, 3.848249166794010634, 3.664874947303708996 ) ) ;
#27192 = EDGE_CURVE ( 'NONE', #52348, #38688, #9730, .T. ) ;
#27193 = EDGE_CURVE ( 'NONE', #9089, #42380, #32133, .T. ) ;
#27194 = EDGE_CURVE ( 'NONE', #83, #32693, #893, .T. ) ;
#27195 = CARTESIAN_POINT ( 'NONE',  ( -14.66887761629205222, 0.000000000000000000, 12.58869632783390990 ) ) ;
#27196 = DIRECTION ( 'NONE',  ( -0.6427681459581293666, -0.7660444431189770143, -0.005002170337467561935 ) ) ;
#27197 = DIRECTION ( 'NONE',  ( -0.005002170337468016433, -0.7660444431189770143, 0.6427681459581293666 ) ) ;
#27198 = DIRECTION ( 'NONE',  ( -0.005002170337468016433, -0.7660444431189770143, 0.6427681459581293666 ) ) ;
#27199 = CARTESIAN_POINT ( 'NONE',  ( -66.84260698025838110, -9.493516685082097339, -1.367274824955978518 ) ) ;
#27200 = CARTESIAN_POINT ( 'NONE',  ( -16.25365031537483063, 0.000000000000000000, 3.095096183115911614 ) ) ;
#27201 = ORIENTED_EDGE ( 'NONE', *, *, #22357, .F. ) ;
#27202 = ADVANCED_FACE ( 'NONE', ( #44073 ), #45194, .F. ) ;
#27203 = ADVANCED_FACE ( 'NONE', ( #35284 ), #52580, .F. ) ;
#27204 = ORIENTED_EDGE ( 'NONE', *, *, #44317, .F. ) ;
#27205 = ORIENTED_EDGE ( 'NONE', *, *, #17277, .F. ) ;
#27206 = EDGE_LOOP ( 'NONE', ( #10318, #55802, #38170, #40436 ) ) ;
#27207 = ADVANCED_FACE ( 'NONE', ( #30991 ), #26750, .F. ) ;
#27208 = EDGE_LOOP ( 'NONE', ( #52449, #24792, #41597, #36803, #25366 ) ) ;
#27209 = CARTESIAN_POINT ( 'NONE',  ( -18.80807110705793406, 0.000000000000000000, 7.090036842313388377 ) ) ;
#27210 = FACE_OUTER_BOUND ( 'NONE', #7227, .T. ) ;
#27211 = EDGE_CURVE ( 'NONE', #3728, #28007, #5190, .T. ) ;
#27212 = EDGE_LOOP ( 'NONE', ( #24288, #49586, #3669, #7823 ) ) ;
#27213 = ORIENTED_EDGE ( 'NONE', *, *, #23735, .F. ) ;
#27214 = ORIENTED_EDGE ( 'NONE', *, *, #17369, .F. ) ;
#27215 = AXIS2_PLACEMENT_3D ( 'NONE', #32302, #10437, #45335 ) ;
#27216 = CARTESIAN_POINT ( 'NONE',  ( -13.07066190154808361, 0.000000000000000000, 12.04713590736729678 ) ) ;
#27217 = ORIENTED_EDGE ( 'NONE', *, *, #40347, .F. ) ;
#27218 = FACE_OUTER_BOUND ( 'NONE', #29262, .T. ) ;
#27219 = CARTESIAN_POINT ( 'NONE',  ( -25.20278734466900517, 0.000000000000000000, 6.670939612111840944 ) ) ;
#27220 = ORIENTED_EDGE ( 'NONE', *, *, #25297, .F. ) ;
#27221 = DIRECTION ( 'NONE',  ( 0.7660212471507180654, -0.6427876096865404731, 0.005961354470445141482 ) ) ;
#27222 = ORIENTED_EDGE ( 'NONE', *, *, #21047, .T. ) ;
#27223 = DIRECTION ( 'NONE',  ( -0.9999697198139514409, -0.000000000000000000, -0.007781995580013368816 ) ) ;
#27224 = LINE ( 'NONE', #40590, #13040 ) ;
#27225 = CARTESIAN_POINT ( 'NONE',  ( -11.30636317915456779, -0.1191753592594197858, 11.32220194836580340 ) ) ;
#27226 = DIRECTION ( 'NONE',  ( -0.2426528472758541499, 0.7422098413412800966, -0.6246952433987894571 ) ) ;
#27227 = VERTEX_POINT ( 'NONE', #9987 ) ;
#27228 = PLANE ( 'NONE',  #25856 ) ;
#27229 = PLANE ( 'NONE',  #37454 ) ;
#27230 = DIRECTION ( 'NONE',  ( -0.6427681459581293666, -0.7660444431189770143, -0.005002170337467561935 ) ) ;
#27231 = VERTEX_POINT ( 'NONE', #27038 ) ;
#27232 = FACE_OUTER_BOUND ( 'NONE', #11533, .T. ) ;
#27233 = ORIENTED_EDGE ( 'NONE', *, *, #6621, .T. ) ;
#27234 = LINE ( 'NONE', #26386, #48301 ) ;
#27235 = CARTESIAN_POINT ( 'NONE',  ( -46.02156441860540781, 4.933012701892111274, -5.000000000000000000 ) ) ;
#27236 = LINE ( 'NONE', #40011, #49397 ) ;
#27237 = DIRECTION ( 'NONE',  ( 0.000000000000000000, -1.000000000000000000, 0.000000000000000000 ) ) ;
#27238 = LINE ( 'NONE', #35229, #23232 ) ;
#27239 = LINE ( 'NONE', #22704, #15881 ) ;
#27240 = CARTESIAN_POINT ( 'NONE',  ( -17.74560456716937296, 0.000000000000000000, 3.774316574337878372 ) ) ;
#27241 = DIRECTION ( 'NONE',  ( 0.000000000000000000, -1.000000000000000000, 0.000000000000000000 ) ) ;
#27242 =( LENGTH_UNIT ( ) NAMED_UNIT ( * ) SI_UNIT ( .MILLI., .METRE. ) );
#27243 = DIRECTION ( 'NONE',  ( 0.007781995580012662783, 0.000000000000000000, -0.9999697198139514409 ) ) ;
#27244 = ORIENTED_EDGE ( 'NONE', *, *, #43017, .T. ) ;
#27245 = CARTESIAN_POINT ( 'NONE',  ( -11.27738753480351264, -0.1191753592594194527, 7.598893875874236592 ) ) ;
#27246 = CARTESIAN_POINT ( 'NONE',  ( -12.30890265829330410, 0.000000000000000000, 7.879279013581050428 ) ) ;
#27247 = CARTESIAN_POINT ( 'NONE',  ( -67.32595136268157887, -0.9999999999999978906, 0.5932824550257459473 ) ) ;
#27248 = DIRECTION ( 'NONE',  ( -0.5449076811759708816, 0.6444004775717707689, 0.5364919789714475140 ) ) ;
#27249 = ADVANCED_FACE ( 'NONE', ( #14274 ), #18807, .F. ) ;
#27250 = EDGE_CURVE ( 'NONE', #22670, #39800, #15589, .T. ) ;
#27251 = DIRECTION ( 'NONE',  ( -0.3620778797217456546, 0.000000000000000000, -0.9321478471874540261 ) ) ;
#27252 = ADVANCED_FACE ( 'NONE', ( #3127 ), #7386, .F. ) ;
#27253 = PLANE ( 'NONE',  #12425 ) ;
#27254 = DIRECTION ( 'NONE',  ( -0.6427681459581293666, -0.7660444431189770143, -0.005002170337467561935 ) ) ;
#27255 = ORIENTED_EDGE ( 'NONE', *, *, #29169, .T. ) ;
#27256 = AXIS2_PLACEMENT_3D ( 'NONE', #54527, #14542, #23357 ) ;
#27257 = VERTEX_POINT ( 'NONE', #37210 ) ;
#27258 = CARTESIAN_POINT ( 'NONE',  ( -14.78014544495433924, -1.003701604285654359, 4.070287485779154224 ) ) ;
#27259 = DIRECTION ( 'NONE',  ( 0.005002170337468016433, -0.7660444431189770143, -0.6427681459581293666 ) ) ;
#27260 = ORIENTED_EDGE ( 'NONE', *, *, #46067, .T. ) ;
#27261 = LINE ( 'NONE', #10530, #37665 ) ;
#27262 = ORIENTED_EDGE ( 'NONE', *, *, #37372, .F. ) ;
#27263 = CARTESIAN_POINT ( 'NONE',  ( 5.618093201498282063, -1.050357395465043364, -2.260480044901387764 ) ) ;
#27264 = ADVANCED_FACE ( 'NONE', ( #50569 ), #7133, .F. ) ;
#27265 = VERTEX_POINT ( 'NONE', #46276 ) ;
#27266 = ORIENTED_EDGE ( 'NONE', *, *, #39323, .T. ) ;
#27267 = EDGE_LOOP ( 'NONE', ( #19854, #31381, #35139, #55550 ) ) ;
#27268 = ADVANCED_FACE ( 'NONE', ( #36962 ), #54514, .F. ) ;
#27269 = DIRECTION ( 'NONE',  ( -0.3620778797217461542, 0.000000000000000000, -0.9321478471874538041 ) ) ;
#27270 = LINE ( 'NONE', #49953, #53158 ) ;
#27271 = CARTESIAN_POINT ( 'NONE',  ( -29.86197018149027116, 0.000000000000000000, 8.281335066757780083 ) ) ;
#27272 = EDGE_CURVE ( 'NONE', #21119, #1201, #19332, .T. ) ;
#27273 = VECTOR ( 'NONE', #41475, 999.9999999999998863 ) ;
#27274 = DIRECTION ( 'NONE',  ( 0.007781995580012662783, 0.000000000000000000, -0.9999697198139514409 ) ) ;
#27275 = ORIENTED_EDGE ( 'NONE', *, *, #19770, .F. ) ;
#27276 = VERTEX_POINT ( 'NONE', #55109 ) ;
#27277 = EDGE_CURVE ( 'NONE', #14069, #19074, #24429, .T. ) ;
#27278 = CARTESIAN_POINT ( 'NONE',  ( -17.95227482402690811, -0.3560938001956556742, 3.843233064070847416 ) ) ;
#27279 = VERTEX_POINT ( 'NONE', #16200 ) ;
#27280 = DIRECTION ( 'NONE',  ( -0.6427681459581293666, -0.7660444431189770143, -0.005002170337467561935 ) ) ;
#27281 = ORIENTED_EDGE ( 'NONE', *, *, #33406, .F. ) ;
#27282 = LINE ( 'NONE', #17657, #7004 ) ;
#27283 = DIRECTION ( 'NONE',  ( -0.6427681459581293666, -0.7660444431189770143, -0.005002170337467561935 ) ) ;
#27284 = ORIENTED_EDGE ( 'NONE', *, *, #172, .T. ) ;
#27285 = VECTOR ( 'NONE', #55647, 1000.000000000000227 ) ;
#27286 = CARTESIAN_POINT ( 'NONE',  ( -10.28764359011173646, -0.1191753592594197858, 0.7776965645825208995 ) ) ;
#27287 = ORIENTED_EDGE ( 'NONE', *, *, #50191, .F. ) ;
#27288 = ADVANCED_BREP_SHAPE_REPRESENTATION ( '', ( #41257, #2610 ), #44334 ) ;
#27289 = AXIS2_PLACEMENT_3D ( 'NONE', #27839, #32379, #32900 ) ;
#27290 = DIRECTION ( 'NONE',  ( -0.6427681459581293666, -0.7660444431189770143, -0.005002170337467561935 ) ) ;
#27291 = VERTEX_POINT ( 'NONE', #53986 ) ;
#27292 = FACE_OUTER_BOUND ( 'NONE', #15101, .T. ) ;
#27293 = CARTESIAN_POINT ( 'NONE',  ( -8.875996589204540044, 0.000000000000000000, 10.41778544861944233 ) ) ;
#27294 = CARTESIAN_POINT ( 'NONE',  ( -10.84028925556084388, -0.1191753592594197858, 11.14116300850493246 ) ) ;
#27295 = VERTEX_POINT ( 'NONE', #50825 ) ;
#27296 = DIRECTION ( 'NONE',  ( 0.005961354470445682716, -0.6427876096865404731, -0.7660212471507180654 ) ) ;
#27297 = DIRECTION ( 'NONE',  ( -0.5364919789714478471, 0.6444004775717705469, -0.5449076811759709926 ) ) ;
#27298 = CARTESIAN_POINT ( 'NONE',  ( -18.39746900504187010, 0.000000000000000000, 14.03700784672088808 ) ) ;
#27299 = FACE_OUTER_BOUND ( 'NONE', #45112, .T. ) ;
#27300 = FACE_OUTER_BOUND ( 'NONE', #54285, .T. ) ;
#27301 = CARTESIAN_POINT ( 'NONE',  ( -67.71562085171136403, -9.593594598721105982, -4.676733487554993296 ) ) ;
#27302 = ORIENTED_EDGE ( 'NONE', *, *, #31747, .F. ) ;
#27303 = DIRECTION ( 'NONE',  ( 0.9659258262890692004, -0.2588190451025176864, 0.000000000000000000 ) ) ;
#27304 = CARTESIAN_POINT ( 'NONE',  ( -22.85266645506453997, 5.305366725996512045, 14.46508349092411372 ) ) ;
#27305 = CARTESIAN_POINT ( 'NONE',  ( -14.55450947277682161, -0.1941918491731548790, 2.654099391803227181 ) ) ;
#27306 = ORIENTED_EDGE ( 'NONE', *, *, #21946, .F. ) ;
#27307 = DIRECTION ( 'NONE',  ( -0.7660212471507179544, -0.6427876096865405842, -0.005961354470445141482 ) ) ;
#27308 = CARTESIAN_POINT ( 'NONE',  ( -27.06552663992790997, 0.000000000000000000, 7.195101427592543786 ) ) ;
#27309 = ORIENTED_EDGE ( 'NONE', *, *, #11846, .T. ) ;
#27310 = ADVANCED_FACE ( 'NONE', ( #11921 ), #28982, .F. ) ;
#27311 = LINE ( 'NONE', #44625, #2572 ) ;
#27312 = VECTOR ( 'NONE', #48193, 1000.000000000000000 ) ;
#27313 = VECTOR ( 'NONE', #176, 1000.000000000000114 ) ;
#27314 = DIRECTION ( 'NONE',  ( -0.005002170337468016433, -0.7660444431189770143, 0.6427681459581293666 ) ) ;
#27315 = EDGE_CURVE ( 'NONE', #21327, #55867, #45727, .T. ) ;
#27316 = EDGE_CURVE ( 'NONE', #15809, #22275, #54812, .T. ) ;
#27317 = DIRECTION ( 'NONE',  ( 0.007781995580012662783, 0.000000000000000000, -0.9999697198139514409 ) ) ;
#27318 = LINE ( 'NONE', #44094, #38364 ) ;
#27319 = VERTEX_POINT ( 'NONE', #54264 ) ;
#27320 = EDGE_LOOP ( 'NONE', ( #10911, #53449, #293, #14047, #12246 ) ) ;
#27321 = DIRECTION ( 'NONE',  ( -0.6427681459581293666, -0.7660444431189770143, -0.005002170337467561935 ) ) ;
#27322 = LINE ( 'NONE', #53713, #9603 ) ;
#27323 = DIRECTION ( 'NONE',  ( 0.5449076811759707706, 0.6444004775717708799, -0.5364919789714476250 ) ) ;
#27324 = DIRECTION ( 'NONE',  ( 0.005961354470445682716, -0.6427876096865404731, -0.7660212471507180654 ) ) ;
#27325 = DIRECTION ( 'NONE',  ( -0.9999697198139514409, -0.000000000000000000, -0.007781995580013368816 ) ) ;
#27326 = ORIENTED_EDGE ( 'NONE', *, *, #37662, .T. ) ;
#27327 = DIRECTION ( 'NONE',  ( 0.6427681459581294776, -0.7660444431189769032, 0.005002170337467562802 ) ) ;
#27328 = ORIENTED_EDGE ( 'NONE', *, *, #12847, .F. ) ;
#27329 = DIRECTION ( 'NONE',  ( 0.007781995580012662783, 0.000000000000000000, -0.9999697198139514409 ) ) ;
#27330 = AXIS2_PLACEMENT_3D ( 'NONE', #1980, #41184, #54501 ) ;
#27331 = FACE_OUTER_BOUND ( 'NONE', #56187, .T. ) ;
#27332 = ORIENTED_EDGE ( 'NONE', *, *, #24767, .F. ) ;
#27333 = DIRECTION ( 'NONE',  ( 0.9999697198139515519, 0.000000000000000000, 0.007781995580013368816 ) ) ;
#27334 = DIRECTION ( 'NONE',  ( -0.7660212471507179544, -0.6427876096865405842, -0.005961354470445141482 ) ) ;
#27335 = DIRECTION ( 'NONE',  ( 0.9999697198139515519, 0.000000000000000000, 0.007781995580013368816 ) ) ;
#27336 = ORIENTED_EDGE ( 'NONE', *, *, #38202, .T. ) ;
#27337 = DIRECTION ( 'NONE',  ( 0.005002170337468016433, -0.7660444431189770143, -0.6427681459581293666 ) ) ;
#27338 = ORIENTED_EDGE ( 'NONE', *, *, #14486, .T. ) ;
#27339 = EDGE_CURVE ( 'NONE', #41467, #35980, #15923, .T. ) ;
#27340 = EDGE_LOOP ( 'NONE', ( #53276, #34592, #13943, #35840 ) ) ;
#27341 = ORIENTED_EDGE ( 'NONE', *, *, #10545, .T. ) ;
#27342 = EDGE_CURVE ( 'NONE', #51521, #40951, #10826, .T. ) ;
#27343 = ORIENTED_EDGE ( 'NONE', *, *, #24596, .F. ) ;
#27344 = LINE ( 'NONE', #44664, #19381 ) ;
#27345 = ORIENTED_EDGE ( 'NONE', *, *, #9191, .F. ) ;
#27346 = DIRECTION ( 'NONE',  ( 0.007781995580012663651, -3.146120232559066537E-19, -0.9999697198139514409 ) ) ;
#27347 = FACE_OUTER_BOUND ( 'NONE', #27206, .T. ) ;
#27348 = AXIS2_PLACEMENT_3D ( 'NONE', #40252, #31480, #1342 ) ;
#27349 = VECTOR ( 'NONE', #12841, 999.9999999999998863 ) ;
#27350 = ORIENTED_EDGE ( 'NONE', *, *, #24319, .T. ) ;
#27351 = EDGE_CURVE ( 'NONE', #4025, #38304, #41201, .T. ) ;
#27352 = VERTEX_POINT ( 'NONE', #49977 ) ;
#27353 = CARTESIAN_POINT ( 'NONE',  ( -14.46888367232926420, 0.000000000000000000, 12.59025272694991315 ) ) ;
#27354 = ORIENTED_EDGE ( 'NONE', *, *, #14826, .T. ) ;
#27355 = CARTESIAN_POINT ( 'NONE',  ( -10.94028622754223967, 0.000000000000000000, 11.14038480894692995 ) ) ;
#27356 = CARTESIAN_POINT ( 'NONE',  ( 2.072287782118878319, 0.000000000000000000, -2.950529333540147015 ) ) ;
#27357 = AXIS2_PLACEMENT_3D ( 'NONE', #47789, #4602, #35014 ) ;
#27358 = FACE_OUTER_BOUND ( 'NONE', #28823, .T. ) ;
#27359 = DIRECTION ( 'NONE',  ( 1.776356839400250465E-15, 0.000000000000000000, -1.000000000000000000 ) ) ;
#27360 = DIRECTION ( 'NONE',  ( 0.005961354470445682716, -0.6427876096865404731, -0.7660212471507180654 ) ) ;
#27361 = DIRECTION ( 'NONE',  ( 0.007781995580012663651, 0.000000000000000000, -0.9999697198139515519 ) ) ;
#27362 = CARTESIAN_POINT ( 'NONE',  ( -15.97845555265929285, 2.714935509636507316, 7.543567584037618623 ) ) ;
#27363 = EDGE_LOOP ( 'NONE', ( #55244, #14863, #38378, #49642 ) ) ;
#27364 = ORIENTED_EDGE ( 'NONE', *, *, #26298, .T. ) ;
#27365 = DIRECTION ( 'NONE',  ( -0.8531650599175527594, 0.4028455766673922356, 0.3313982828793700652 ) ) ;
#27366 = PLANE ( 'NONE',  #51167 ) ;
#27367 = ADVANCED_FACE ( 'NONE', ( #46026 ), #2296, .F. ) ;
#27368 = VECTOR ( 'NONE', #4041, 1000.000000000000227 ) ;
#27369 = LINE ( 'NONE', #17755, #47839 ) ;
#27370 = DIRECTION ( 'NONE',  ( 0.5364919789714477361, 0.6444004775717706579, 0.5449076811759711036 ) ) ;
#27371 = ORIENTED_EDGE ( 'NONE', *, *, #7873, .T. ) ;
#27372 = CARTESIAN_POINT ( 'NONE',  ( -11.87243407472968926, 0.000000000000000000, 11.50246268866867361 ) ) ;
#27373 = DIRECTION ( 'NONE',  ( -0.5449076811759708816, 0.6444004775717707689, 0.5364919789714475140 ) ) ;
#27374 = EDGE_LOOP ( 'NONE', ( #19300, #45861, #45177, #21045 ) ) ;
#27375 = DIRECTION ( 'NONE',  ( 0.000000000000000000, -0.000000000000000000, -1.000000000000000000 ) ) ;
#27376 = EDGE_CURVE ( 'NONE', #52765, #42286, #20156, .T. ) ;
#27377 = CARTESIAN_POINT ( 'NONE',  ( -20.72814514249575168, 20.40220053346460460, 4.343046601168861542 ) ) ;
#27378 = ORIENTED_EDGE ( 'NONE', *, *, #37481, .F. ) ;
#27379 = PLANE ( 'NONE',  #14365 ) ;
#27380 = CARTESIAN_POINT ( 'NONE',  ( -17.31821934845932631, 1.581621852479005774, 3.358454237843607082 ) ) ;
#27381 = EDGE_CURVE ( 'NONE', #39217, #53467, #37491, .T. ) ;
#27382 = DIRECTION ( 'NONE',  ( 0.007781995580012663651, -3.146120232559066537E-19, -0.9999697198139514409 ) ) ;
#27383 = ADVANCED_FACE ( 'NONE', ( #17304 ), #3978, .F. ) ;
#27384 = EDGE_CURVE ( 'NONE', #14373, #8011, #46874, .T. ) ;
#27385 = DIRECTION ( 'NONE',  ( 0.000000000000000000, -0.000000000000000000, -1.000000000000000000 ) ) ;
#27386 = LINE ( 'NONE', #45279, #37377 ) ;
#27387 = ORIENTED_EDGE ( 'NONE', *, *, #27978, .T. ) ;
#27388 = ORIENTED_EDGE ( 'NONE', *, *, #55147, .F. ) ;
#27389 = DIRECTION ( 'NONE',  ( 0.6427681459581294776, -0.7660444431189769032, 0.005002170337467562802 ) ) ;
#27390 = CARTESIAN_POINT ( 'NONE',  ( -19.60834386242827776, 0.000000000000000000, 4.298478389818581213 ) ) ;
#27391 = CARTESIAN_POINT ( 'NONE',  ( -12.29740644427217156, 0.000000000000000000, 6.402040200549994786 ) ) ;
#27392 = VECTOR ( 'NONE', #5219, 1000.000000000000227 ) ;
#27393 = AXIS2_PLACEMENT_3D ( 'NONE', #31214, #5650, #6234 ) ;
#27394 = PRODUCT_DEFINITION ( 'UNKNOWN', '', #25369, #50699 ) ;
#27395 = CARTESIAN_POINT ( 'NONE',  ( -11.67244013076689946, 0.000000000000000000, 11.50401908778467863 ) ) ;
#27396 = FACE_BOUND ( 'NONE', #15812, .T. ) ;
#27397 = ORIENTED_EDGE ( 'NONE', *, *, #2594, .T. ) ;
#27398 = CARTESIAN_POINT ( 'NONE',  ( -16.32483125059555107, 23.23313012887437168, -3.980127950647806223 ) ) ;
#27399 = CARTESIAN_POINT ( 'NONE',  ( -18.34056015671156459, 0.000000000000000000, 6.724343050823632595 ) ) ;
#27400 = ADVANCED_FACE ( 'NONE', ( #38911 ), #7981, .F. ) ;
#27401 = LINE ( 'NONE', #2407, #17828 ) ;
#27402 = CARTESIAN_POINT ( 'NONE',  ( -13.24105050548075724, 0.000000000000000000, 8.241356893302796749 ) ) ;
#27403 = AXIS2_PLACEMENT_3D ( 'NONE', #40601, #40009, #30930 ) ;
#27404 = ORIENTED_EDGE ( 'NONE', *, *, #2128, .T. ) ;
#27405 = CARTESIAN_POINT ( 'NONE',  ( -18.10994763196841006, -1.651309408375658760, 3.863154378167301228 ) ) ;
#27406 = ORIENTED_EDGE ( 'NONE', *, *, #10563, .F. ) ;
#27407 = CARTESIAN_POINT ( 'NONE',  ( -21.35351436783577483, 20.32981857746640841, -4.374509389852473618 ) ) ;
#27408 = FACE_OUTER_BOUND ( 'NONE', #30498, .T. ) ;
#27409 = ORIENTED_EDGE ( 'NONE', *, *, #1085, .T. ) ;
#27410 = DIRECTION ( 'NONE',  ( -0.5364919789714478471, 0.6444004775717705469, -0.5449076811759709926 ) ) ;
#27411 = AXIS2_PLACEMENT_3D ( 'NONE', #12702, #21213, #29164 ) ;
#27412 = VERTEX_POINT ( 'NONE', #34627 ) ;
#27413 = EDGE_LOOP ( 'NONE', ( #4864, #32090, #36720, #16441 ) ) ;
#27414 = ORIENTED_EDGE ( 'NONE', *, *, #8882, .T. ) ;
#27415 = DIRECTION ( 'NONE',  ( 0.007781995580012662783, 0.000000000000000000, -0.9999697198139514409 ) ) ;
#27416 = ORIENTED_EDGE ( 'NONE', *, *, #50118, .F. ) ;
#27417 = ORIENTED_EDGE ( 'NONE', *, *, #22529, .F. ) ;
#27418 = DIRECTION ( 'NONE',  ( 0.005002170337468016433, -0.7660444431189770143, -0.6427681459581293666 ) ) ;
#27419 = CARTESIAN_POINT ( 'NONE',  ( -13.00457969848779705, -2.784623065533159636, 1.843897454566881144 ) ) ;
#27420 = ORIENTED_EDGE ( 'NONE', *, *, #2638, .F. ) ;
#27421 = VERTEX_POINT ( 'NONE', #43183 ) ;
#27422 = DIRECTION ( 'NONE',  ( 0.5364919789714477361, 0.6444004775717706579, 0.5449076811759711036 ) ) ;
#27423 = ADVANCED_FACE ( 'NONE', ( #17052 ), #34938, .F. ) ;
#27424 = ORIENTED_EDGE ( 'NONE', *, *, #48258, .F. ) ;
#27425 = VECTOR ( 'NONE', #40477, 1000.000000000000114 ) ;
#27426 = ORIENTED_EDGE ( 'NONE', *, *, #14097, .F. ) ;
#27427 = CARTESIAN_POINT ( 'NONE',  ( -24.27063949748155380, 0.000000000000000000, 6.308861732390097288 ) ) ;
#27428 = LINE ( 'NONE', #760, #52998 ) ;
#27429 = CARTESIAN_POINT ( 'NONE',  ( 5.359786524431354948, 0.000000000000000000, 2.456654125669140765 ) ) ;
#27430 = CARTESIAN_POINT ( 'NONE',  ( -67.02664427580020856, -11.39393312870849151, -7.454399636913917604 ) ) ;
#27431 = AXIS2_PLACEMENT_3D ( 'NONE', #6326, #45476, #23627 ) ;
#27432 = EDGE_LOOP ( 'NONE', ( #16501, #19531, #18926, #36169, #42573, #54009 ) ) ;
#27433 = DIRECTION ( 'NONE',  ( 0.5449076811759707706, 0.6444004775717708799, -0.5364919789714476250 ) ) ;
#27434 = EDGE_LOOP ( 'NONE', ( #41925, #2596, #20387, #569 ) ) ;
#27435 = EDGE_CURVE ( 'NONE', #17107, #5134, #4539, .T. ) ;
#27436 = AXIS2_PLACEMENT_3D ( 'NONE', #51634, #3385, #33741 ) ;
#27437 = VECTOR ( 'NONE', #16992, 1000.000000000000227 ) ;
#27438 = DIRECTION ( 'NONE',  ( 0.005002170337468016433, -0.7660444431189770143, -0.6427681459581293666 ) ) ;
#27439 = EDGE_CURVE ( 'NONE', #15806, #11344, #47719, .T. ) ;
#27440 = EDGE_CURVE ( 'NONE', #42498, #51400, #8829, .T. ) ;
#27441 = DIRECTION ( 'NONE',  ( 0.007781995580012663651, 0.000000000000000000, -0.9999697198139515519 ) ) ;
#27442 = VECTOR ( 'NONE', #14697, 999.9999999999998863 ) ;
#27443 = VECTOR ( 'NONE', #46494, 1000.000000000000227 ) ;
#27444 = CARTESIAN_POINT ( 'NONE',  ( -70.00279782826048347, 0.1332992376639058896, -7.501782499249456393 ) ) ;
#27445 = DIRECTION ( 'NONE',  ( 0.007781995580012662783, 0.000000000000000000, -0.9999697198139514409 ) ) ;
#27446 = CARTESIAN_POINT ( 'NONE',  ( -19.51511390298037441, -5.536956232915666298, 4.284996200178408543 ) ) ;
#27447 = CARTESIAN_POINT ( 'NONE',  ( -18.62376508501084516, 0.000000000000000000, 9.107457517013187953 ) ) ;
#27448 = ORIENTED_EDGE ( 'NONE', *, *, #23176, .F. ) ;
#27449 = PLANE ( 'NONE',  #31984 ) ;
#27450 = EDGE_CURVE ( 'NONE', #9775, #37986, #8235, .T. ) ;
#27451 = ORIENTED_EDGE ( 'NONE', *, *, #18189, .F. ) ;
#27452 = PLANE ( 'NONE',  #21114 ) ;
#27453 = CARTESIAN_POINT ( 'NONE',  ( -18.50832163360941607, 4.657758921906512306, 3.722585503579211252 ) ) ;
#27454 = ADVANCED_FACE ( 'NONE', ( #25852 ), #34099, .F. ) ;
#27455 = PLANE ( 'NONE',  #27215 ) ;
#27456 = VECTOR ( 'NONE', #13204, 999.9999999999998863 ) ;
#27457 = LINE ( 'NONE', #10138, #18659 ) ;
#27458 = VECTOR ( 'NONE', #35322, 1000.000000000000227 ) ;
#27459 = EDGE_CURVE ( 'NONE', #48603, #25745, #51417, .T. ) ;
#27460 = DIRECTION ( 'NONE',  ( 0.9999697198139515519, 0.000000000000000000, 0.007781995580013368816 ) ) ;
#27461 = CARTESIAN_POINT ( 'NONE',  ( -70.71258200891328727, -1.000000000000000000, 8.208045577613541255 ) ) ;
#27462 = ORIENTED_EDGE ( 'NONE', *, *, #4878, .T. ) ;
#27463 = CARTESIAN_POINT ( 'NONE',  ( -13.45815220315852834, 0.000000000000000000, 2.130348184563771063 ) ) ;
#27464 = FACE_OUTER_BOUND ( 'NONE', #20772, .T. ) ;
#27465 = DIRECTION ( 'NONE',  ( 0.000000000000000000, -0.000000000000000000, -1.000000000000000000 ) ) ;
#27466 = VECTOR ( 'NONE', #546, 999.9999999999998863 ) ;
#27467 = EDGE_CURVE ( 'NONE', #33250, #17419, #46391, .T. ) ;
#27468 = CARTESIAN_POINT ( 'NONE',  ( -10.78260220767254118, -0.1191753592594188005, 3.728501240626274527 ) ) ;
#27469 = CARTESIAN_POINT ( 'NONE',  ( -14.63627885039329257, 0.000000000000000000, 8.399824917293743809 ) ) ;
#27470 = VECTOR ( 'NONE', #6800, 999.9999999999998863 ) ;
#27471 = CARTESIAN_POINT ( 'NONE',  ( -19.33759994122731385, 21.49370731433205250, -4.239680377485293583 ) ) ;
#27472 = EDGE_CURVE ( 'NONE', #19882, #39633, #51673, .T. ) ;
#27473 = CARTESIAN_POINT ( 'NONE',  ( -1.086233639165236964, -1.000000000000000000, -2.796443541562362078 ) ) ;
#27474 = VECTOR ( 'NONE', #18179, 1000.000000000000227 ) ;
#27475 = DIRECTION ( 'NONE',  ( 0.000000000000000000, -1.000000000000000000, 0.000000000000000000 ) ) ;
#27476 = VECTOR ( 'NONE', #50156, 999.9999999999998863 ) ;
#27477 = VECTOR ( 'NONE', #12074, 1000.000000000000114 ) ;
#27478 = ORIENTED_EDGE ( 'NONE', *, *, #36259, .T. ) ;
#27479 = VECTOR ( 'NONE', #5549, 1000.000000000000000 ) ;
#27480 = VERTEX_POINT ( 'NONE', #47133 ) ;
#27481 = ORIENTED_EDGE ( 'NONE', *, *, #8357, .F. ) ;
#27482 = AXIS2_PLACEMENT_3D ( 'NONE', #52266, #12529, #38924 ) ;
#27483 = ORIENTED_EDGE ( 'NONE', *, *, #8364, .T. ) ;
#27484 = ORIENTED_EDGE ( 'NONE', *, *, #28759, .F. ) ;
#27485 = CARTESIAN_POINT ( 'NONE',  ( -2.579292853887890757, -4.639166217699263406, -2.216488638059722849 ) ) ;
#27486 = FACE_OUTER_BOUND ( 'NONE', #32696, .T. ) ;
#27487 = ORIENTED_EDGE ( 'NONE', *, *, #16164, .T. ) ;
#27488 = ORIENTED_EDGE ( 'NONE', *, *, #24670, .T. ) ;
#27489 = VECTOR ( 'NONE', #29829, 1000.000000000000227 ) ;
#27490 = EDGE_CURVE ( 'NONE', #19740, #26046, #52254, .T. ) ;
#27491 = ORIENTED_EDGE ( 'NONE', *, *, #5979, .F. ) ;
#27492 = AXIS2_PLACEMENT_3D ( 'NONE', #35143, #16965, #39087 ) ;
#27493 = FACE_OUTER_BOUND ( 'NONE', #5684, .T. ) ;
#27494 = CARTESIAN_POINT ( 'NONE',  ( -11.20636620717317378, 0.000000000000000000, 11.32298014792380414 ) ) ;
#27495 = LINE ( 'NONE', #9640, #21416 ) ;
#27496 = EDGE_LOOP ( 'NONE', ( #15151, #12619, #32045, #32337 ) ) ;
#27497 = DIRECTION ( 'NONE',  ( 0.007781995580012663651, -3.146120232559066537E-19, -0.9999697198139514409 ) ) ;
#27498 = EDGE_CURVE ( 'NONE', #37937, #9627, #30681, .T. ) ;
#27499 = VECTOR ( 'NONE', #43316, 1000.000000000000227 ) ;
#27500 = ADVANCED_FACE ( 'NONE', ( #47981 ), #20743, .F. ) ;
#27501 = VERTEX_POINT ( 'NONE', #38060 ) ;
#27502 = DIRECTION ( 'NONE',  ( 0.007781995580012663651, -3.146120232559066537E-19, -0.9999697198139514409 ) ) ;
#27504 = VECTOR ( 'NONE', #42256, 1000.000000000000227 ) ;
#27503 = CARTESIAN_POINT ( 'NONE',  ( -15.87975247367846166, 0.000000000000000000, 2.850166870931599927 ) ) ;
#27505 = EDGE_CURVE ( 'NONE', #50409, #33297, #33793, .T. ) ;
#27506 = DIRECTION ( 'NONE',  ( 0.3313982828793700097, 0.4028455766673915694, 0.8531650599175529814 ) ) ;
#27507 = FACE_OUTER_BOUND ( 'NONE', #52018, .T. ) ;
#27508 = LINE ( 'NONE', #24093, #23191 ) ;
#27509 = CARTESIAN_POINT ( 'NONE',  ( 1.971453974394196562, 0.000000000000000000, 10.00639841352631088 ) ) ;
#27510 = PLANE ( 'NONE',  #8511 ) ;
#27511 = AXIS2_PLACEMENT_3D ( 'NONE', #53806, #15736, #23700 ) ;
#27512 = ORIENTED_EDGE ( 'NONE', *, *, #2594, .F. ) ;
#27513 = LINE ( 'NONE', #35766, #31036 ) ;
#27514 = ORIENTED_EDGE ( 'NONE', *, *, #33646, .T. ) ;
#27515 = VECTOR ( 'NONE', #46636, 1000.000000000000227 ) ;
#27516 = VECTOR ( 'NONE', #48400, 999.9999999999998863 ) ;
#27517 = DIRECTION ( 'NONE',  ( 0.007781995580012663651, 0.000000000000000000, -0.9999697198139515519 ) ) ;
#27518 = CARTESIAN_POINT ( 'NONE',  ( -15.86710544311044302, 0.000000000000000000, 13.13336954653252953 ) ) ;
#27519 = CARTESIAN_POINT ( 'NONE',  ( -27.06630483948590893, -0.1191753592594197858, 7.295098399573937797 ) ) ;
#27520 = EDGE_CURVE ( 'NONE', #29311, #2552, #4818, .T. ) ;
#27521 = LINE ( 'NONE', #53376, #52243 ) ;
#27522 = FACE_OUTER_BOUND ( 'NONE', #19524, .T. ) ;
#27523 = DIRECTION ( 'NONE',  ( 0.000000000000000000, -1.000000000000000000, 0.000000000000000000 ) ) ;
#27524 = DIRECTION ( 'NONE',  ( -0.7886751345948130876, 0.2113248654051844977, -0.5773502691896263972 ) ) ;
#27525 = EDGE_CURVE ( 'NONE', #38808, #43441, #31217, .T. ) ;
#27526 = VECTOR ( 'NONE', #36352, 999.9999999999998863 ) ;
#27527 = FACE_OUTER_BOUND ( 'NONE', #9119, .T. ) ;
#27528 = AXIS2_PLACEMENT_3D ( 'NONE', #12728, #39125, #3919 ) ;
#27529 = EDGE_CURVE ( 'NONE', #39202, #6097, #44839, .T. ) ;
#27530 = CARTESIAN_POINT ( 'NONE',  ( -10.47421230394850866, 0.000000000000000000, 10.95934586908605723 ) ) ;
#27531 = ORIENTED_EDGE ( 'NONE', *, *, #43529, .T. ) ;
#27532 = CARTESIAN_POINT ( 'NONE',  ( -20.27093655581709797, -1.975113310420657520, 7.797349324992047137 ) ) ;
#27533 = CARTESIAN_POINT ( 'NONE',  ( -12.70458494993575194, -0.1191753592594197858, 11.86531876794841978 ) ) ;
#27534 = DIRECTION ( 'NONE',  ( 0.007781995580012663651, 0.000000000000000000, -0.9999697198139515519 ) ) ;
#27535 = DIRECTION ( 'NONE',  ( 0.5449076811759707706, 0.6444004775717708799, -0.5364919789714476250 ) ) ;
#27536 = EDGE_CURVE ( 'NONE', #20287, #49088, #23277, .T. ) ;
#27537 = LINE ( 'NONE', #32083, #50888 ) ;
#27538 = DIRECTION ( 'NONE',  ( 0.000000000000000000, -0.000000000000000000, -1.000000000000000000 ) ) ;
#27539 = DIRECTION ( 'NONE',  ( -0.5364919789714478471, 0.6444004775717705469, -0.5449076811759709926 ) ) ;
#27540 = ORIENTED_EDGE ( 'NONE', *, *, #10159, .T. ) ;
#27541 = ORIENTED_EDGE ( 'NONE', *, *, #21478, .T. ) ;
#27542 = AXIS2_PLACEMENT_3D ( 'NONE', #34680, #42928, #8579 ) ;
#27543 = LINE ( 'NONE', #23005, #44033 ) ;
#27544 = FACE_OUTER_BOUND ( 'NONE', #18326, .T. ) ;
#27545 = VECTOR ( 'NONE', #11845, 1000.000000000000227 ) ;
#27546 = VERTEX_POINT ( 'NONE', #13890 ) ;
#27547 = DIRECTION ( 'NONE',  ( -0.005961354470445682716, -0.6427876096865404731, 0.7660212471507180654 ) ) ;
#27548 = VECTOR ( 'NONE', #4482, 1000.000000000000227 ) ;
#27549 = ORIENTED_EDGE ( 'NONE', *, *, #39377, .T. ) ;
#27550 = FACE_BOUND ( 'NONE', #39735, .T. ) ;
#27551 = ORIENTED_EDGE ( 'NONE', *, *, #50261, .T. ) ;
#27552 = VERTEX_POINT ( 'NONE', #35225 ) ;
#27553 = VERTEX_POINT ( 'NONE', #44291 ) ;
#27554 = CARTESIAN_POINT ( 'NONE',  ( -17.20686196644532728, 0.000000000000000000, 6.163827626255103276 ) ) ;
#27555 = VECTOR ( 'NONE', #45700, 1000.000000000000227 ) ;
#27556 = CARTESIAN_POINT ( 'NONE',  ( 2.072287782118878319, 0.000000000000000000, -2.950529333540147015 ) ) ;
#27557 = PLANE ( 'NONE',  #49358 ) ;
#27558 = ADVANCED_FACE ( 'NONE', ( #48545 ), #22699, .F. ) ;
#27559 = VECTOR ( 'NONE', #24426, 1000.000000000000227 ) ;
#27560 = CARTESIAN_POINT ( 'NONE',  ( -16.43317633868556626, -0.1191753592594197858, 13.31363028683540151 ) ) ;
#27561 = ORIENTED_EDGE ( 'NONE', *, *, #48204, .T. ) ;
#27563 = ORIENTED_EDGE ( 'NONE', *, *, #26540, .T. ) ;
#27562 = ADVANCED_FACE ( 'NONE', ( #9353 ), #1393, .F. ) ;
#27564 = AXIS2_PLACEMENT_3D ( 'NONE', #19851, #40872, #11332 ) ;
#27565 = AXIS2_PLACEMENT_3D ( 'NONE', #6957, #14903, #28509 ) ;
#27566 = CARTESIAN_POINT ( 'NONE',  ( -11.34358382343173410, 0.000000000000000000, 3.254800454061105963 ) ) ;
#27568 = EDGE_CURVE ( 'NONE', #43270, #428, #1096, .T. ) ;
#27567 = EDGE_LOOP ( 'NONE', ( #23190, #23260, #806, #11017 ) ) ;
#27569 = DIRECTION ( 'NONE',  ( -0.9999697198139514409, -0.000000000000000000, -0.007781995580013368816 ) ) ;
#27570 = ORIENTED_EDGE ( 'NONE', *, *, #40533, .F. ) ;
#27571 = CARTESIAN_POINT ( 'NONE',  ( -20.54049170961573267, 0.000000000000000000, 4.660556269540326646 ) ) ;
#27572 = PLANE ( 'NONE',  #17652 ) ;
#27573 = EDGE_CURVE ( 'NONE', #3951, #931, #833, .T. ) ;
#27574 = EDGE_CURVE ( 'NONE', #50902, #10838, #18434, .T. ) ;
#27575 = ADVANCED_FACE ( 'NONE', ( #26677 ), #43997, .F. ) ;
#27576 = ORIENTED_EDGE ( 'NONE', *, *, #16680, .T. ) ;
#27577 = DIRECTION ( 'NONE',  ( -0.9999697198139514409, -0.000000000000000000, -0.007781995580013368816 ) ) ;
#27578 = ORIENTED_EDGE ( 'NONE', *, *, #9618, .T. ) ;
#27579 = ADVANCED_FACE ( 'NONE', ( #49089 ), #18740, .F. ) ;
#27580 = VECTOR ( 'NONE', #52705, 1000.000000000000227 ) ;
#27581 = DIRECTION ( 'NONE',  ( 0.000000000000000000, -0.000000000000000000, -1.000000000000000000 ) ) ;
#27582 = AXIS2_PLACEMENT_3D ( 'NONE', #26235, #35062, #21120 ) ;
#27583 = VERTEX_POINT ( 'NONE', #53090 ) ;
#27584 = CARTESIAN_POINT ( 'NONE',  ( -17.46532115785441519, 0.000000000000000000, 13.67492996699914265 ) ) ;
#27585 = CARTESIAN_POINT ( 'NONE',  ( -10.06709704724974763, 0.4073222041869798971, 1.076279759381168599 ) ) ;
#27586 = PLANE ( 'NONE',  #53689 ) ;
#27587 = ORIENTED_EDGE ( 'NONE', *, *, #35223, .T. ) ;
#27588 = VECTOR ( 'NONE', #16324, 1000.000000000000227 ) ;
#27589 = CARTESIAN_POINT ( 'NONE',  ( -16.41364898034673558, -0.1191753592594159833, 9.593992249496130498 ) ) ;
#27590 = CARTESIAN_POINT ( 'NONE',  ( -12.13851405436063047, 0.000000000000000000, 11.68505802764555135 ) ) ;
#27591 = CARTESIAN_POINT ( 'NONE',  ( -69.97756022945675625, 0.4191520680014513278, 7.501241569353455318 ) ) ;
#27592 = EDGE_CURVE ( 'NONE', #21318, #29013, #48833, .T. ) ;
#27593 = VECTOR ( 'NONE', #1855, 999.9999999999998863 ) ;
#27594 = CARTESIAN_POINT ( 'NONE',  ( -18.19747506107908563, 0.000000000000000000, 14.03856424583689311 ) ) ;
#27595 = PLANE ( 'NONE',  #3146 ) ;
#27596 = FACE_OUTER_BOUND ( 'NONE', #13548, .T. ) ;
#27597 = EDGE_CURVE ( 'NONE', #14368, #4104, #44546, .T. ) ;
#27598 = CARTESIAN_POINT ( 'NONE',  ( -68.18449814332990400, -11.52670909917258690, -6.247493715003795245 ) ) ;
#27599 = ORIENTED_EDGE ( 'NONE', *, *, #55023, .T. ) ;
#27600 = CARTESIAN_POINT ( 'NONE',  ( -3.184385661761863773, -6.114012816731704270, -1.981450042443219539 ) ) ;
#27601 = CARTESIAN_POINT ( 'NONE',  ( -15.40103151951671734, 0.000000000000000000, 12.95233060667165681 ) ) ;
#27602 = EDGE_CURVE ( 'NONE', #18340, #26523, #5121, .T. ) ;
#27603 = CARTESIAN_POINT ( 'NONE',  ( -66.73496964911797136, 1.799964814818122178E-11, 2.845885083211338262 ) ) ;
#27604 = ORIENTED_EDGE ( 'NONE', *, *, #25614, .F. ) ;
#27605 = VECTOR ( 'NONE', #5090, 1000.000000000000000 ) ;
#27606 = PLANE ( 'NONE',  #55611 ) ;
#27607 = LINE ( 'NONE', #40928, #53560 ) ;
#27608 = ORIENTED_EDGE ( 'NONE', *, *, #26188, .T. ) ;
#27609 = VECTOR ( 'NONE', #7316, 1000.000000000000227 ) ;
#27610 = EDGE_CURVE ( 'NONE', #26525, #19811, #53373, .T. ) ;
#27611 = PLANE ( 'NONE',  #20417 ) ;
#27612 = DIRECTION ( 'NONE',  ( 0.007781995580012663651, -3.146120232559066537E-19, -0.9999697198139514409 ) ) ;
#27613 = EDGE_CURVE ( 'NONE', #34665, #40913, #27234, .T. ) ;
#27614 = CARTESIAN_POINT ( 'NONE',  ( -19.91123888593303803, 0.7721120973665051013, 5.882689981159765047 ) ) ;
#27615 = ORIENTED_EDGE ( 'NONE', *, *, #5751, .T. ) ;
#27616 = VECTOR ( 'NONE', #43594, 999.9999999999998863 ) ;
#27617 = AXIS2_PLACEMENT_3D ( 'NONE', #12871, #16559, #7482 ) ;
#27618 = ORIENTED_EDGE ( 'NONE', *, *, #18745, .F. ) ;
#27619 = PLANE ( 'NONE',  #38606 ) ;
#27620 = DIRECTION ( 'NONE',  ( 0.007781995580012663651, 0.000000000000000000, -0.9999697198139515519 ) ) ;
#27621 = CARTESIAN_POINT ( 'NONE',  ( -16.36399307677613280, -0.1191753592594193417, 4.423729705925692812 ) ) ;
#27622 = CARTESIAN_POINT ( 'NONE',  ( -27.99767448711536133, 0.000000000000000000, 7.557179307314289218 ) ) ;
#27623 = ORIENTED_EDGE ( 'NONE', *, *, #15567, .F. ) ;
#27624 = DIRECTION ( 'NONE',  ( 0.000000000000000000, 0.000000000000000000, -1.000000000000000000 ) ) ;
#27625 = ORIENTED_EDGE ( 'NONE', *, *, #17770, .T. ) ;
#27626 = CARTESIAN_POINT ( 'NONE',  ( -17.65293688786543314, 0.000000000000000000, 3.775037735645530912 ) ) ;
#27627 = AXIS2_PLACEMENT_3D ( 'NONE', #55099, #29545, #479 ) ;
#27628 = PLANE ( 'NONE',  #39571 ) ;
#27629 = ORIENTED_EDGE ( 'NONE', *, *, #19798, .F. ) ;
#27630 = VECTOR ( 'NONE', #45715, 1000.000000000000114 ) ;
#27631 = CARTESIAN_POINT ( 'NONE',  ( -13.68433194158294164, 3.848249166794009746, 8.512412852383034689 ) ) ;
#27632 = CARTESIAN_POINT ( 'NONE',  ( -31.72626587586518099, 0.000000000000000000, 9.005490826201270949 ) ) ;
#27633 = VECTOR ( 'NONE', #17306, 1000.000000000000000 ) ;
#27634 = CARTESIAN_POINT ( 'NONE',  ( -60.88973930853472893, 7.404220597074750110, -3.000000000000006661 ) ) ;
#27635 = ORIENTED_EDGE ( 'NONE', *, *, #41123, .T. ) ;
#27636 = CARTESIAN_POINT ( 'NONE',  ( -13.63673279712320507, -0.1191753592594197858, 12.22739664767016521 ) ) ;
#27637 = ORIENTED_EDGE ( 'NONE', *, *, #35791, .T. ) ;
#27638 = ORIENTED_EDGE ( 'NONE', *, *, #12053, .F. ) ;
#27639 = ORIENTED_EDGE ( 'NONE', *, *, #8058, .F. ) ;
#27640 = DIRECTION ( 'NONE',  ( -0.5364919789714478471, 0.6444004775717705469, -0.5449076811759709926 ) ) ;
#27641 = AXIS2_PLACEMENT_3D ( 'NONE', #36831, #2700, #27753 ) ;
#27642 = ORIENTED_EDGE ( 'NONE', *, *, #14569, .T. ) ;
#27643 = AXIS2_PLACEMENT_3D ( 'NONE', #41650, #20063, #28894 ) ;
#27644 = CARTESIAN_POINT ( 'NONE',  ( -17.22566268659302580, 0.000000000000000000, 8.579679789764480091 ) ) ;
#27645 = VERTEX_POINT ( 'NONE', #43700 ) ;
#27646 = DIRECTION ( 'NONE',  ( -0.3313982828793700097, 0.4028455766673915694, -0.8531650599175529814 ) ) ;
#27647 = CARTESIAN_POINT ( 'NONE',  ( -18.40664086144219169, -1.975113310420657520, 7.073193565548556272 ) ) ;
#27648 = AXIS2_PLACEMENT_3D ( 'NONE', #42950, #25358, #12304 ) ;
#27649 = EDGE_CURVE ( 'NONE', #32585, #12755, #17902, .T. ) ;
#27650 = EDGE_CURVE ( 'NONE', #43814, #44524, #19835, .T. ) ;
#27651 = ORIENTED_EDGE ( 'NONE', *, *, #1326, .F. ) ;
#27652 = LINE ( 'NONE', #35603, #4985 ) ;
#27653 = ORIENTED_EDGE ( 'NONE', *, *, #42331, .F. ) ;
#27654 = ADVANCED_FACE ( 'NONE', ( #53912 ), #45966, .F. ) ;
#27655 = VECTOR ( 'NONE', #19435, 1000.000000000000227 ) ;
#27656 = DIRECTION ( 'NONE',  ( -0.6427681459581293666, -0.7660444431189770143, -0.005002170337467561935 ) ) ;
#27657 = VECTOR ( 'NONE', #52391, 999.9999999999998863 ) ;
#27658 = PLANE ( 'NONE',  #54686 ) ;
#27659 = DIRECTION ( 'NONE',  ( -0.3620778797217457656, 0.000000000000000000, -0.9321478471874539151 ) ) ;
#27660 = CARTESIAN_POINT ( 'NONE',  ( -19.79006065298467121, -3.594132820645660420, 10.26764763322216112 ) ) ;
#27661 = CARTESIAN_POINT ( 'NONE',  ( -21.35352775840775408, 20.32981084641607339, 4.374505632834054580 ) ) ;
#27662 = PLANE ( 'NONE',  #11939 ) ;
#27663 = CARTESIAN_POINT ( 'NONE',  ( 2.072287782118878319, 0.000000000000000000, -2.950529333540147015 ) ) ;
#27664 = ORIENTED_EDGE ( 'NONE', *, *, #6171, .T. ) ;
#27665 = ORIENTED_EDGE ( 'NONE', *, *, #18047, .T. ) ;
#27666 = DIRECTION ( 'NONE',  ( 0.9999697198139515519, 0.000000000000000000, 0.007781995580013368816 ) ) ;
#27667 = DIRECTION ( 'NONE',  ( 0.7660212471507180654, -0.6427876096865404731, 0.005961354470445141482 ) ) ;
#27668 = PLANE ( 'NONE',  #42401 ) ;
#27669 = VECTOR ( 'NONE', #17259, 1000.000000000000227 ) ;
#27670 = CARTESIAN_POINT ( 'NONE',  ( -15.13495153988577968, 0.000000000000000000, 12.76973526769478084 ) ) ;
#27671 = VERTEX_POINT ( 'NONE', #24370 ) ;
#27672 = CLOSED_SHELL ( 'NONE', ( #1795, #51154, #17072, #21565, #55733, #30221, #3165, #49444, #31876, #14752, #933, #27929, #33085, #55639, #22849, #38702, #39445, #19090, #4476, #3147, #9055, #46556, #26919, #27080, #35921, #19544, #15981, #55658, #10890, #37759, #34518, #4051, #6816, #17391, #37231, #45932, #42385 ) ) ;
#27673 = DIRECTION ( 'NONE',  ( -0.6427681459581293666, -0.7660444431189770143, -0.005002170337467561935 ) ) ;
#27674 = CARTESIAN_POINT ( 'NONE',  ( -10.43598480340254397, 0.000000000000000000, 6.047194144364267387 ) ) ;
#27675 = VERTEX_POINT ( 'NONE', #41681 ) ;
#27676 = LINE ( 'NONE', #5268, #35679 ) ;
#27677 = DIRECTION ( 'NONE',  ( 0.007781995580012662783, 0.000000000000000000, -0.9999697198139514409 ) ) ;
#27678 = VECTOR ( 'NONE', #15706, 999.9999999999998863 ) ;
#27679 = VERTEX_POINT ( 'NONE', #10768 ) ;
#27680 = PLANE ( 'NONE',  #4390 ) ;
#27681 = CARTESIAN_POINT ( 'NONE',  ( -17.85580488533350518, 0.000000000000000000, 4.142791039787291574 ) ) ;
#27682 = VECTOR ( 'NONE', #29771, 1000.000000000000227 ) ;
#27683 = DIRECTION ( 'NONE',  ( -0.8531650599175527594, 0.4028455766673922356, 0.3313982828793700652 ) ) ;
#27684 = ADVANCED_FACE ( 'NONE', ( #11021 ), #37730, .F. ) ;
#27685 = LINE ( 'NONE', #49810, #30551 ) ;
#27686 = FACE_OUTER_BOUND ( 'NONE', #41275, .T. ) ;
#27687 = ORIENTED_EDGE ( 'NONE', *, *, #55673, .F. ) ;
#27688 = VECTOR ( 'NONE', #1527, 1000.000000000000227 ) ;
#27689 = VECTOR ( 'NONE', #4061, 1000.000000000000227 ) ;
#27690 = ADVANCED_FACE ( 'NONE', ( #49674 ), #28646, .F. ) ;
#27691 = ORIENTED_EDGE ( 'NONE', *, *, #53935, .F. ) ;
#27692 = AXIS2_PLACEMENT_3D ( 'NONE', #38467, #4122, #8367 ) ;
#27693 = PLANE ( 'NONE',  #27565 ) ;
#27694 = DIRECTION ( 'NONE',  ( -0.6427681459581293666, -0.7660444431189770143, -0.005002170337467561935 ) ) ;
#27695 = DIRECTION ( 'NONE',  ( 0.5364919789714477361, 0.6444004775717706579, 0.5449076811759711036 ) ) ;
#27696 = ADVANCED_FACE ( 'NONE', ( #20090 ), #15029, .F. ) ;
#27697 = AXIS2_PLACEMENT_3D ( 'NONE', #55309, #16404, #38567 ) ;
#27698 = DIRECTION ( 'NONE',  ( 0.007781995580012663651, 0.000000000000000000, -0.9999697198139515519 ) ) ;
#27699 = ADVANCED_FACE ( 'NONE', ( #41433 ), #16142, .F. ) ;
#27700 = CARTESIAN_POINT ( 'NONE',  ( -12.72887235343914725, 0.000000000000000000, 2.136023608983785849 ) ) ;
#27701 = ORIENTED_EDGE ( 'NONE', *, *, #381, .T. ) ;
#27702 = DIRECTION ( 'NONE',  ( 0.000000000000000000, -1.000000000000000000, 0.000000000000000000 ) ) ;
#27703 = DIRECTION ( 'NONE',  ( -0.9999697198139514409, -0.000000000000000000, -0.007781995580013368816 ) ) ;
#27704 = VECTOR ( 'NONE', #43357, 1000.000000000000000 ) ;
#27705 = DIRECTION ( 'NONE',  ( 0.005961354470445682716, -0.6427876096865404731, -0.7660212471507180654 ) ) ;
#27706 = CIRCLE ( 'NONE', #47728, 2.750000000000006217 ) ;
#27707 = PLANE ( 'NONE',  #9692 ) ;
#27708 = ORIENTED_EDGE ( 'NONE', *, *, #36904, .F. ) ;
#27709 = DIRECTION ( 'NONE',  ( 0.005961354470445682716, -0.6427876096865404731, -0.7660212471507180654 ) ) ;
#27710 = VERTEX_POINT ( 'NONE', #41953 ) ;
#27711 = FACE_OUTER_BOUND ( 'NONE', #37106, .T. ) ;
#27712 = DIRECTION ( 'NONE',  ( 0.005961354470445682716, -0.6427876096865404731, -0.7660212471507180654 ) ) ;
#27713 = EDGE_LOOP ( 'NONE', ( #40497, #24537, #23408, #29230 ) ) ;
#27714 = LINE ( 'NONE', #1591, #12709 ) ;
#27715 = ORIENTED_EDGE ( 'NONE', *, *, #36943, .F. ) ;
#27716 = VECTOR ( 'NONE', #51826, 1000.000000000000000 ) ;
#27717 = ORIENTED_EDGE ( 'NONE', *, *, #44544, .F. ) ;
#27718 = ORIENTED_EDGE ( 'NONE', *, *, #20528, .T. ) ;
#27719 = CARTESIAN_POINT ( 'NONE',  ( -32.96103433568752195, 13.62821379940322508, 4.845353415783987927 ) ) ;
#27720 = ORIENTED_EDGE ( 'NONE', *, *, #41395, .T. ) ;
#27721 = AXIS2_PLACEMENT_3D ( 'NONE', #21875, #38079, #55391 ) ;
#27722 = ORIENTED_EDGE ( 'NONE', *, *, #17215, .T. ) ;
#27723 = DIRECTION ( 'NONE',  ( 0.000000000000000000, -1.000000000000000000, 0.000000000000000000 ) ) ;
#27724 = CARTESIAN_POINT ( 'NONE',  ( -29.86352658060627618, 0.000000000000000000, 8.481329010720569883 ) ) ;
#27725 = VECTOR ( 'NONE', #53565, 1000.000000000000227 ) ;
#27726 = ORIENTED_EDGE ( 'NONE', *, *, #28272, .T. ) ;
#27727 = EDGE_CURVE ( 'NONE', #50963, #15779, #15848, .T. ) ;
#27728 = ORIENTED_EDGE ( 'NONE', *, *, #53929, .T. ) ;
#27729 = CARTESIAN_POINT ( 'NONE',  ( -10.22449464541862341, 0.000000000000000000, 4.571511730449213218 ) ) ;
#27730 = ORIENTED_EDGE ( 'NONE', *, *, #6596, .F. ) ;
#27731 = VECTOR ( 'NONE', #21664, 1000.000000000000227 ) ;
#27732 = ORIENTED_EDGE ( 'NONE', *, *, #55868, .T. ) ;
#27733 = EDGE_CURVE ( 'NONE', #39217, #2132, #50509, .T. ) ;
#27734 = EDGE_CURVE ( 'NONE', #3468, #26120, #3059, .T. ) ;
#27735 = VECTOR ( 'NONE', #17660, 1000.000000000000227 ) ;
#27736 = VECTOR ( 'NONE', #31351, 1000.000000000000227 ) ;
#27737 = LINE ( 'NONE', #10702, #4801 ) ;
#27738 = DIRECTION ( 'NONE',  ( 0.000000000000000000, -1.000000000000000000, 0.000000000000000000 ) ) ;
#27739 = CARTESIAN_POINT ( 'NONE',  ( 5.500940387028403933, 0.000000000000000000, 2.400892578144000922 ) ) ;
#27740 = CARTESIAN_POINT ( 'NONE',  ( -26.13415699229845757, -0.1191753592594197858, 6.933020519852192365 ) ) ;
#27741 = ORIENTED_EDGE ( 'NONE', *, *, #1578, .T. ) ;
#27742 = DIRECTION ( 'NONE',  ( 0.000000000000000000, -1.000000000000000000, 0.000000000000000000 ) ) ;
#27743 = VERTEX_POINT ( 'NONE', #28077 ) ;
#27744 = VECTOR ( 'NONE', #27683, 999.9999999999998863 ) ;
#27745 = VECTOR ( 'NONE', #25536, 1000.000000000000114 ) ;
#27746 = AXIS2_PLACEMENT_3D ( 'NONE', #53932, #32906, #46234 ) ;
#27747 = CARTESIAN_POINT ( 'NONE',  ( -14.94916102560700821, 0.000000000000000000, 2.688082935172642962 ) ) ;
#27748 = EDGE_CURVE ( 'NONE', #36809, #26836, #11604, .T. ) ;
#27749 = VECTOR ( 'NONE', #31688, 999.9999999999998863 ) ;
#27750 = LINE ( 'NONE', #45070, #45123 ) ;
#27751 = VECTOR ( 'NONE', #50444, 1000.000000000000227 ) ;
#27752 = LINE ( 'NONE', #19191, #12267 ) ;
#27753 = DIRECTION ( 'NONE',  ( 0.005002170337468016433, -0.7660444431189770143, -0.6427681459581293666 ) ) ;
#27754 = FACE_OUTER_BOUND ( 'NONE', #23637, .T. ) ;
#27755 = DIRECTION ( 'NONE',  ( 0.000000000000000000, -1.000000000000000000, 0.000000000000000000 ) ) ;
#27756 = EDGE_LOOP ( 'NONE', ( #12838, #8659, #49417, #12895 ) ) ;
#27757 = CARTESIAN_POINT ( 'NONE',  ( 1.086233639165236964, 0.000000000000000000, 2.796443541562362078 ) ) ;
#27758 = EDGE_LOOP ( 'NONE', ( #42638, #1024 ) ) ;
#27759 = CARTESIAN_POINT ( 'NONE',  ( -13.94446387365259810, 0.000000000000000000, 4.911894139562900996 ) ) ;
#27760 = DIRECTION ( 'NONE',  ( -0.7660212471507179544, -0.6427876096865405842, -0.005961354470445141482 ) ) ;
#27761 = DIRECTION ( 'NONE',  ( -0.7660212471507179544, -0.6427876096865405842, -0.005961354470445141482 ) ) ;
#27762 = FACE_OUTER_BOUND ( 'NONE', #29951, .T. ) ;
#27763 = DIRECTION ( 'NONE',  ( 0.6427681459581294776, -0.7660444431189769032, 0.005002170337467562802 ) ) ;
#27764 = AXIS2_PLACEMENT_3D ( 'NONE', #9166, #29922, #17402 ) ;
#27765 = CARTESIAN_POINT ( 'NONE',  ( -71.01620612404938981, -1.000000000000001776, -8.550077602493738382 ) ) ;
#27766 = ORIENTED_EDGE ( 'NONE', *, *, #25515, .F. ) ;
#27767 = CARTESIAN_POINT ( 'NONE',  ( -23.33693525117809386, 0.000000000000000000, 5.746789908705562944 ) ) ;
#27768 = LINE ( 'NONE', #49874, #53919 ) ;
#27769 = DIRECTION ( 'NONE',  ( -0.5364919789714478471, 0.6444004775717705469, -0.5449076811759709926 ) ) ;
#27770 = VECTOR ( 'NONE', #21393, 1000.000000000000227 ) ;
#27771 = CARTESIAN_POINT ( 'NONE',  ( -68.48236398700224470, 1.836504256775132404, -7.469194291234003025 ) ) ;
#27772 = EDGE_CURVE ( 'NONE', #9097, #52074, #6236, .T. ) ;
#27773 = VECTOR ( 'NONE', #3691, 1000.000000000000000 ) ;
#27774 = CARTESIAN_POINT ( 'NONE',  ( -17.31625929850056878, -0.1191753592594162470, 7.370975508451782510 ) ) ;
#27775 = PLANE ( 'NONE',  #5512 ) ;
#27776 = LINE ( 'NONE', #45619, #26542 ) ;
#27777 = AXIS2_PLACEMENT_3D ( 'NONE', #55306, #29185, #12152 ) ;
#27778 = AXIS2_PLACEMENT_3D ( 'NONE', #49788, #37556, #6352 ) ;
#27779 = CARTESIAN_POINT ( 'NONE',  ( -70.12381838982661009, -8.729438269679169693, -8.047023921085742160 ) ) ;
#27780 = CARTESIAN_POINT ( 'NONE',  ( -12.55630129013990448, 0.000000000000000000, 5.661361281382457200 ) ) ;
#27781 = VECTOR ( 'NONE', #41968, 1000.000000000000114 ) ;
#27782 = EDGE_CURVE ( 'NONE', #42852, #6281, #32612, .T. ) ;
#27783 = ORIENTED_EDGE ( 'NONE', *, *, #24695, .F. ) ;
#27784 = VECTOR ( 'NONE', #45946, 1000.000000000000000 ) ;
#27785 = EDGE_CURVE ( 'NONE', #22811, #32117, #45382, .T. ) ;
#27786 = EDGE_CURVE ( 'NONE', #15806, #45145, #2221, .T. ) ;
#27787 = AXIS2_PLACEMENT_3D ( 'NONE', #40948, #19372, #15144 ) ;
#27788 = EDGE_LOOP ( 'NONE', ( #32791, #20872, #29624, #20489 ) ) ;
#27789 = VECTOR ( 'NONE', #49249, 1000.000000000000227 ) ;
#27790 = ORIENTED_EDGE ( 'NONE', *, *, #51672, .F. ) ;
#27791 = ORIENTED_EDGE ( 'NONE', *, *, #55505, .F. ) ;
#27792 = VERTEX_POINT ( 'NONE', #54204 ) ;
#27793 = DIRECTION ( 'NONE',  ( 0.9999697198139515519, 0.000000000000000000, 0.007781995580013368816 ) ) ;
#27794 = EDGE_CURVE ( 'NONE', #54764, #43539, #24103, .T. ) ;
#27795 = CARTESIAN_POINT ( 'NONE',  ( -13.08408713167409942, -0.1191753592594197858, 1.863930203747758085 ) ) ;
#27797 = EDGE_CURVE ( 'NONE', #9219, #40567, #50205, .T. ) ;
#27796 = ORIENTED_EDGE ( 'NONE', *, *, #16105, .T. ) ;
#27798 = ORIENTED_EDGE ( 'NONE', *, *, #27459, .F. ) ;
#27799 = ORIENTED_EDGE ( 'NONE', *, *, #27650, .T. ) ;
#27800 = ADVANCED_FACE ( 'NONE', ( #17248 ), #38003, .F. ) ;
#27801 = VECTOR ( 'NONE', #38809, 999.9999999999998863 ) ;
#27802 = DIRECTION ( 'NONE',  ( 0.000000000000000000, -0.000000000000000000, -1.000000000000000000 ) ) ;
#27803 = LINE ( 'NONE', #15285, #33729 ) ;
#27804 = FACE_OUTER_BOUND ( 'NONE', #18302, .T. ) ;
#27805 = EDGE_LOOP ( 'NONE', ( #44887, #18477, #39025, #45305 ) ) ;
#27806 = VECTOR ( 'NONE', #47426, 999.9999999999998863 ) ;
#27807 = CARTESIAN_POINT ( 'NONE',  ( -15.52856807626791813, -2.460819163488160655, 2.834631295277566743 ) ) ;
#27808 = EDGE_CURVE ( 'NONE', #24601, #25044, #47346, .T. ) ;
#27809 = VERTEX_POINT ( 'NONE', #29484 ) ;
#27810 = DIRECTION ( 'NONE',  ( -0.6427681459581293666, -0.7660444431189770143, -0.005002170337467561935 ) ) ;
#27811 = VECTOR ( 'NONE', #39000, 1000.000000000000227 ) ;
#27812 = DIRECTION ( 'NONE',  ( 0.5000000000000011102, -0.8660254037844380415, 0.000000000000000000 ) ) ;
#27813 = ADVANCED_FACE ( 'NONE', ( #25783 ), #55304, .F. ) ;
#27814 = FACE_OUTER_BOUND ( 'NONE', #4190, .T. ) ;
#27815 = DIRECTION ( 'NONE',  ( 0.7660212471507180654, -0.6427876096865404731, 0.005961354470445141482 ) ) ;
#27816 = VECTOR ( 'NONE', #31464, 1000.000000000000000 ) ;
#27817 = CARTESIAN_POINT ( 'NONE',  ( -11.09304826722767956, 24.43504809471621542, 3.000000000000000000 ) ) ;
#27818 = DIRECTION ( 'NONE',  ( 0.000000000000000000, -0.000000000000000000, -1.000000000000000000 ) ) ;
#27819 = DIRECTION ( 'NONE',  ( -0.5449076811759708816, 0.6444004775717707689, 0.5364919789714475140 ) ) ;
#27820 = CARTESIAN_POINT ( 'NONE',  ( -8.108005289889504752, 5.801717509616975299, -0.06894897205205396951 ) ) ;
#27821 = VERTEX_POINT ( 'NONE', #34570 ) ;
#27822 = FACE_OUTER_BOUND ( 'NONE', #29706, .T. ) ;
#27823 = VERTEX_POINT ( 'NONE', #4486 ) ;
#27824 = VECTOR ( 'NONE', #35917, 999.9999999999998863 ) ;
#27825 = CARTESIAN_POINT ( 'NONE',  ( -17.94484721929616455, 1.743523803501505709, 6.713128782598690947 ) ) ;
#27826 = DIRECTION ( 'NONE',  ( 0.7660212471507180654, -0.6427876096865404731, 0.005961354470445141482 ) ) ;
#27827 = DIRECTION ( 'NONE',  ( 0.6427681459581294776, -0.7660444431189769032, 0.005002170337467562802 ) ) ;
#27828 = DIRECTION ( 'NONE',  ( -0.7660212471507179544, -0.6427876096865405842, -0.005961354470445141482 ) ) ;
#27829 = DIRECTION ( 'NONE',  ( 0.007781995580012663651, -3.146120232559066537E-19, -0.9999697198139514409 ) ) ;
#27830 = DIRECTION ( 'NONE',  ( 0.005002170337468016433, -0.7660444431189770143, -0.6427681459581293666 ) ) ;
#27831 = DIRECTION ( 'NONE',  ( 0.007781995580012662783, 0.000000000000000000, -0.9999697198139514409 ) ) ;
#27832 = VECTOR ( 'NONE', #37772, 999.9999999999998863 ) ;
#27833 = AXIS2_PLACEMENT_3D ( 'NONE', #13381, #42892, #47433 ) ;
#27834 = CARTESIAN_POINT ( 'NONE',  ( -16.46321184919952785, 0.000000000000000000, 4.322954534386297176 ) ) ;
#27835 = PLANE ( 'NONE',  #50995 ) ;
#27836 = ORIENTED_EDGE ( 'NONE', *, *, #7414, .F. ) ;
#27837 = DIRECTION ( 'NONE',  ( -0.005002170337468016433, -0.7660444431189770143, 0.6427681459581293666 ) ) ;
#27838 = PLANE ( 'NONE',  #38516 ) ;
#27839 = CARTESIAN_POINT ( 'NONE',  ( -58.00000000000000711, 2.000000000000000000, 7.102951435054649637E-15 ) ) ;
#27840 = LINE ( 'NONE', #1113, #48510 ) ;
#27841 = DIRECTION ( 'NONE',  ( 0.007781995580012663651, -3.146120232559066537E-19, -0.9999697198139514409 ) ) ;
#27842 = EDGE_CURVE ( 'NONE', #10018, #14930, #21795, .T. ) ;
#27843 = FACE_OUTER_BOUND ( 'NONE', #30432, .T. ) ;
#27844 = DIRECTION ( 'NONE',  ( 0.9999697198139515519, 0.000000000000000000, 0.007781995580013368816 ) ) ;
#27845 = CARTESIAN_POINT ( 'NONE',  ( -17.19536575242419474, 0.000000000000000000, 4.686588813224045857 ) ) ;
#27846 = AXIS2_PLACEMENT_3D ( 'NONE', #19056, #49731, #6856 ) ;
#27847 = ORIENTED_EDGE ( 'NONE', *, *, #13239, .T. ) ;
#27848 = ORIENTED_EDGE ( 'NONE', *, *, #52909, .T. ) ;
#27849 = CARTESIAN_POINT ( 'NONE',  ( -31.72626587586518099, 0.000000000000000000, 9.005490826201270949 ) ) ;
#27850 = PRODUCT ( 'Steel Pivot Pin Shaft', 'Steel Pivot Pin Shaft', '', ( #47354 ) ) ;
#27851 = DIRECTION ( 'NONE',  ( -0.5364919789714478471, 0.6444004775717705469, -0.5449076811759709926 ) ) ;
#27852 = ORIENTED_EDGE ( 'NONE', *, *, #45197, .T. ) ;
#27853 = DIRECTION ( 'NONE',  ( 0.5364919789714477361, 0.6444004775717706579, 0.5449076811759711036 ) ) ;
#27854 = VECTOR ( 'NONE', #54098, 1000.000000000000227 ) ;
#27855 = ORIENTED_EDGE ( 'NONE', *, *, #55608, .T. ) ;
#27856 = CARTESIAN_POINT ( 'NONE',  ( 5.345667018682350502, -1.081588725305391074, -2.421850695157840239 ) ) ;
#27857 = EDGE_CURVE ( 'NONE', #27103, #27945, #21545, .T. ) ;
#27858 = VECTOR ( 'NONE', #25637, 1000.000000000000227 ) ;
#27859 = ORIENTED_EDGE ( 'NONE', *, *, #5661, .F. ) ;
#27860 = ORIENTED_EDGE ( 'NONE', *, *, #14359, .F. ) ;
#27861 = ORIENTED_EDGE ( 'NONE', *, *, #30439, .T. ) ;
#27862 = LINE ( 'NONE', #23317, #46515 ) ;
#27863 = CARTESIAN_POINT ( 'NONE',  ( -16.99924723426068951, 0.000000000000000000, 13.49389102713827171 ) ) ;
#27864 = DIRECTION ( 'NONE',  ( -0.6427681459581293666, -0.7660444431189770143, -0.005002170337467561935 ) ) ;
#27865 = VECTOR ( 'NONE', #32876, 999.9999999999998863 ) ;
#27866 = EDGE_CURVE ( 'NONE', #40728, #44870, #8765, .T. ) ;
#27867 = ORIENTED_EDGE ( 'NONE', *, *, #2516, .F. ) ;
#27868 = ORIENTED_EDGE ( 'NONE', *, *, #30885, .T. ) ;
#27869 = EDGE_CURVE ( 'NONE', #20518, #35510, #46805, .T. ) ;
#27870 = AXIS2_PLACEMENT_3D ( 'NONE', #3518, #29670, #55196 ) ;
#27871 = LINE ( 'NONE', #45179, #27273 ) ;
#27872 = ORIENTED_EDGE ( 'NONE', *, *, #30959, .T. ) ;
#27873 = CARTESIAN_POINT ( 'NONE',  ( -18.16355864079104165, 0.000000000000000000, 9.680377076001752457 ) ) ;
#27874 = ORIENTED_EDGE ( 'NONE', *, *, #28887, .T. ) ;
#27875 = DIRECTION ( 'NONE',  ( 0.9999697198139515519, 0.000000000000000000, 0.007781995580013368816 ) ) ;
#27876 = CARTESIAN_POINT ( 'NONE',  ( -15.86710544311044302, 0.000000000000000000, 13.13336954653252953 ) ) ;
#27877 = EDGE_CURVE ( 'NONE', #15287, #9855, #55892, .T. ) ;
#27878 = ORIENTED_EDGE ( 'NONE', *, *, #52080, .F. ) ;
#27879 = CARTESIAN_POINT ( 'NONE',  ( -24.83619454210204580, 18.20872041849631984, -4.561852789702152577 ) ) ;
#27880 = ADVANCED_FACE ( 'NONE', ( #51884 ), #13001, .F. ) ;
#27881 = DIRECTION ( 'NONE',  ( -0.3620778797217455991, 0.000000000000000000, -0.9321478471874540261 ) ) ;
#27882 = ORIENTED_EDGE ( 'NONE', *, *, #49876, .T. ) ;
#27883 = DIRECTION ( 'NONE',  ( 0.005961354470445682716, -0.6427876096865404731, -0.7660212471507180654 ) ) ;
#27884 = CARTESIAN_POINT ( 'NONE',  ( -15.50102849149811135, -0.1191753592594197858, 12.95155240711365430 ) ) ;
#27885 = CARTESIAN_POINT ( 'NONE',  ( -15.07085755779227121, 0.000000000000000000, 4.533796213653115359 ) ) ;
#27886 = VERTEX_POINT ( 'NONE', #30326 ) ;
#27887 = DIRECTION ( 'NONE',  ( 0.5364919789714477361, 0.6444004775717706579, 0.5449076811759711036 ) ) ;
#27888 = DIRECTION ( 'NONE',  ( -0.5449076811759708816, 0.6444004775717707689, 0.5364919789714475140 ) ) ;
#27889 = DIRECTION ( 'NONE',  ( 0.5449076811759707706, 0.6444004775717708799, -0.5364919789714476250 ) ) ;
#27890 = CARTESIAN_POINT ( 'NONE',  ( -13.56467548170849113, -0.1191753592594185229, 2.968186363502689051 ) ) ;
#27891 = DIRECTION ( 'NONE',  ( -0.5364919789714478471, 0.6444004775717705469, -0.5449076811759709926 ) ) ;
#27892 = DIRECTION ( 'NONE',  ( 0.9999697198139515519, 0.000000000000000000, 0.007781995580013368816 ) ) ;
#27893 = VECTOR ( 'NONE', #54922, 1000.000000000000000 ) ;
#27894 = CARTESIAN_POINT ( 'NONE',  ( -66.74797292598515241, -11.36197671352631033, 2.764386752171343886 ) ) ;
#27895 = ORIENTED_EDGE ( 'NONE', *, *, #38149, .T. ) ;
#27896 = DIRECTION ( 'NONE',  ( -0.5364919789714478471, 0.6444004775717705469, -0.5449076811759709926 ) ) ;
#27897 =( BOUNDED_SURFACE ( )  B_SPLINE_SURFACE ( 3, 2, ( 
 ( #49357, #10752, #48522 ),
 ( #44816, #9637, #6217 ),
 ( #6475, #41112, #2200 ),
 ( #26958, #44270, #31501 ),
 ( #1074, #53607, #22958 ),
 ( #10477, #40580, #36050 ),
 ( #49071, #32596, #29463 ),
 ( #11289, #15823, #3033 ),
 ( #16376, #24083, #20367 ),
 ( #49898, #46784, #16122 ),
 ( #42243, #7052, #3344 ),
 ( #55286, #7589, #2495 ),
 ( #20667, #45641, #24918 ),
 ( #6759, #37982, #19815 ),
 ( #41408, #45944, #50179 ),
 ( #33701, #24351, #37136 ),
 ( #15532, #11001, #28622 ),
 ( #41659, #51016, #25213 ),
 ( #54435, #29159, #41933 ),
 ( #12126, #7902, #2745 ),
 ( #54718, #20070, #33441 ),
 ( #32866, #42521, #50745 ),
 ( #37396, #55031, #19537 ),
 ( #36879, #11838, #33170 ),
 ( #50486, #11585, #28901 ),
 ( #54184, #37708, #46472 ),
 ( #15284, #46197, #7302 ),
 ( #24614, #28323, #42778 ) ),
 .UNSPECIFIED., .F., .F., .F. ) 
 B_SPLINE_SURFACE_WITH_KNOTS ( ( 4, 2, 2, 2, 2, 2, 2, 2, 2, 2, 2, 2, 2, 4 ),
 ( 3, 3 ),
 ( 0.005951394764495080564, 0.008223488340404870242, 0.009359535128359765949, 0.01049558191631465992, 0.01276767549222445133, 0.01390372228017934531, 0.01503976906813424101, 0.01617581585608913672, 0.01731186264404403069, 0.01958395621995382210, 0.02072000300790871608, 0.02185604979586361352, 0.02299209658381850749, 0.02412814337177340146 ),
 ( 0.000000000000000000, 1.000000000000000000 ),
 .UNSPECIFIED. ) 
 GEOMETRIC_REPRESENTATION_ITEM ( )  RATIONAL_B_SPLINE_SURFACE ( (
 ( 1.000000000000000000, 0.9218171296615468302, 1.000000000000000000),
 ( 1.000000000000000000, 0.9219582590430798197, 1.000000000000000000),
 ( 1.000000000000000000, 0.9217654209506799257, 1.000000000000000000),
 ( 1.000000000000000000, 0.9218193965221213038, 1.000000000000000000),
 ( 1.000000000000000000, 0.9217886515252998736, 1.000000000000000000),
 ( 1.000000000000000000, 0.9217705453229111390, 1.000000000000000000),
 ( 1.000000000000000000, 0.9217728555244316668, 1.000000000000000000),
 ( 1.000000000000000000, 0.9217839018303625176, 1.000000000000000000),
 ( 1.000000000000000000, 0.9217902773702886243, 1.000000000000000000),
 ( 1.000000000000000000, 0.9218159477367721122, 1.000000000000000000),
 ( 1.000000000000000000, 0.9218381644593317548, 1.000000000000000000),
 ( 1.000000000000000000, 0.9218170478688526570, 1.000000000000000000),
 ( 1.000000000000000000, 0.9218183721990944601, 1.000000000000000000),
 ( 1.000000000000000000, 0.9218243750419194971, 1.000000000000000000),
 ( 1.000000000000000000, 0.9218291361985332388, 1.000000000000000000),
 ( 1.000000000000000000, 0.9218339850781324119, 1.000000000000000000),
 ( 1.000000000000000000, 0.9218340914605103187, 1.000000000000000000),
 ( 1.000000000000000000, 0.9218311426340464187, 1.000000000000000000),
 ( 1.000000000000000000, 0.9218408506499762289, 1.000000000000000000),
 ( 1.000000000000000000, 0.9218298856244220296, 1.000000000000000000),
 ( 1.000000000000000000, 0.9218235216675588761, 1.000000000000000000),
 ( 1.000000000000000000, 0.9218049054827647248, 1.000000000000000000),
 ( 1.000000000000000000, 0.9217926302233848679, 1.000000000000000000),
 ( 1.000000000000000000, 0.9217749384510963706, 1.000000000000000000),
 ( 1.000000000000000000, 0.9217695517188546628, 1.000000000000000000),
 ( 1.000000000000000000, 0.9217886187906820794, 1.000000000000000000),
 ( 1.000000000000000000, 0.9218984684751962977, 1.000000000000000000),
 ( 1.000000000000000000, 0.9217608302862904113, 1.000000000000000000) ) ) 
 REPRESENTATION_ITEM ( '' )  SURFACE ( )  );
#27898 = CARTESIAN_POINT ( 'NONE',  ( -15.09672403933981499, 0.000000000000000000, 7.857583542972994550 ) ) ;
#27899 = CARTESIAN_POINT ( 'NONE',  ( -65.67246414475930294, 5.724587470723463412E-14, -1.520040349668396962 ) ) ;
#27900 = ORIENTED_EDGE ( 'NONE', *, *, #8048, .T. ) ;
#27901 = PLANE ( 'NONE',  #41100 ) ;
#27902 = CARTESIAN_POINT ( 'NONE',  ( -15.16696776448257822, 4.010151117816512567, 2.445352267504874444 ) ) ;
#27903 = EDGE_CURVE ( 'NONE', #40567, #43820, #21232, .T. ) ;
#27904 = VECTOR ( 'NONE', #47562, 999.9999999999998863 ) ;
#27905 = DIRECTION ( 'NONE',  ( 0.007781995580012663651, 0.000000000000000000, -0.9999697198139515519 ) ) ;
#27906 = EDGE_CURVE ( 'NONE', #53549, #46700, #189, .T. ) ;
#27907 = DIRECTION ( 'NONE',  ( 0.7660212471507180654, -0.6427876096865404731, 0.005961354470445141482 ) ) ;
#27908 = CARTESIAN_POINT ( 'NONE',  ( -17.28751876344774274, -0.1191753592594176486, 3.677878475874140740 ) ) ;
#27909 = EDGE_LOOP ( 'NONE', ( #29666, #27540, #1646, #53484 ) ) ;
#27910 = EDGE_CURVE ( 'NONE', #8254, #8418, #33459, .T. ) ;
#27911 = EDGE_LOOP ( 'NONE', ( #43041, #32036, #34291, #2035 ) ) ;
#27912 = EDGE_CURVE ( 'NONE', #52707, #52840, #29183, .T. ) ;
#27913 = CARTESIAN_POINT ( 'NONE',  ( -10.18275984876991558, -0.1191753592594204103, 0.7785127941096396942 ) ) ;
#27914 = CARTESIAN_POINT ( 'NONE',  ( -65.57067994458799376, 1.999999999999980904, 2.608662443145409071 ) ) ;
#27915 = EDGE_CURVE ( 'NONE', #43426, #51541, #24941, .T. ) ;
#27916 = ADVANCED_FACE ( 'NONE', ( #20688 ), #16400, .F. ) ;
#27917 = EDGE_CURVE ( 'NONE', #44396, #48501, #51040, .T. ) ;
#27918 = LINE ( 'NONE', #40687, #34766 ) ;
#27919 = ORIENTED_EDGE ( 'NONE', *, *, #19588, .T. ) ;
#27920 = CARTESIAN_POINT ( 'NONE',  ( -17.83139810946674686, -0.1191753592594197858, 13.85674710641801788 ) ) ;
#27921 = ORIENTED_EDGE ( 'NONE', *, *, #18647, .F. ) ;
#27922 = DIRECTION ( 'NONE',  ( -0.7660212471507179544, -0.6427876096865405842, -0.005961354470445141482 ) ) ;
#27923 = ORIENTED_EDGE ( 'NONE', *, *, #21094, .F. ) ;
#27924 = CARTESIAN_POINT ( 'NONE',  ( 2.072287782118878319, 0.000000000000000000, -2.950529333540147015 ) ) ;
#27925 = DIRECTION ( 'NONE',  ( 0.007781995580012662783, 0.000000000000000000, -0.9999697198139514409 ) ) ;
#27926 = PLANE ( 'NONE',  #7605 ) ;
#27927 = VERTEX_POINT ( 'NONE', #12150 ) ;
#27928 = PLANE ( 'NONE',  #53749 ) ;
#27929 = ADVANCED_FACE ( 'NONE', ( #8183 ), #39699, .F. ) ;
#27930 = ORIENTED_EDGE ( 'NONE', *, *, #29853, .F. ) ;
#27932 = ORIENTED_EDGE ( 'NONE', *, *, #21867, .T. ) ;
#27931 = ADVANCED_FACE ( 'NONE', ( #10135 ), #31463, .F. ) ;
#27933 = ORIENTED_EDGE ( 'NONE', *, *, #14689, .T. ) ;
#27934 = DIRECTION ( 'NONE',  ( 0.005002170337468016433, -0.7660444431189770143, -0.6427681459581293666 ) ) ;
#27935 = ADVANCED_FACE ( 'NONE', ( #1329 ), #27452, .F. ) ;
#27936 = ORIENTED_EDGE ( 'NONE', *, *, #35403, .F. ) ;
#27937 = CARTESIAN_POINT ( 'NONE',  ( -12.80458192191714595, 0.000000000000000000, 11.86454056839041726 ) ) ;
#27938 = ORIENTED_EDGE ( 'NONE', *, *, #47024, .T. ) ;
#27939 = LINE ( 'NONE', #37007, #19483 ) ;
#27940 = CARTESIAN_POINT ( 'NONE',  ( -27.56484202182514665, 16.74370688441070953, -4.657437592157546824 ) ) ;
#27941 = EDGE_CURVE ( 'NONE', #21134, #5084, #35170, .T. ) ;
#27942 = VECTOR ( 'NONE', #38977, 999.9999999999998863 ) ;
#27943 = ORIENTED_EDGE ( 'NONE', *, *, #2751, .F. ) ;
#27944 = FACE_OUTER_BOUND ( 'NONE', #54779, .T. ) ;
#27945 = VERTEX_POINT ( 'NONE', #22077 ) ;
#27946 = CARTESIAN_POINT ( 'NONE',  ( -19.33760068587298164, 21.49370688441072019, 4.239878526350478793 ) ) ;
#27947 = FACE_OUTER_BOUND ( 'NONE', #25037, .T. ) ;
#27948 = PLANE ( 'NONE',  #15958 ) ;
#27949 = CARTESIAN_POINT ( 'NONE',  ( -4.849237023859344298, 4.749459929012077808, 5.101981916513284254 ) ) ;
#27950 = PLANE ( 'NONE',  #49588 ) ;
#27951 = DIRECTION ( 'NONE',  ( 0.000000000000000000, -1.000000000000000000, 0.000000000000000000 ) ) ;
#27952 = DIRECTION ( 'NONE',  ( 0.6427681459581294776, -0.7660444431189769032, 0.005002170337467562802 ) ) ;
#27953 = VERTEX_POINT ( 'NONE', #14420 ) ;
#27954 = ORIENTED_EDGE ( 'NONE', *, *, #25260, .F. ) ;
#27955 = LINE ( 'NONE', #53759, #36439 ) ;
#27956 = PLANE ( 'NONE',  #33010 ) ;
#27957 = CARTESIAN_POINT ( 'NONE',  ( 5.907100043276122037, -1.017206840181698935, -1.544800305917336303 ) ) ;
#27958 = DIRECTION ( 'NONE',  ( 0.005002170337468016433, -0.7660444431189770143, -0.6427681459581293666 ) ) ;
#27959 = CARTESIAN_POINT ( 'NONE',  ( -17.41990852354524577, 0.000000000000000000, 7.839503984132946357 ) ) ;
#27960 = ORIENTED_EDGE ( 'NONE', *, *, #7375, .F. ) ;
#27961 = CARTESIAN_POINT ( 'NONE',  ( -18.62244743062156260, 0.000000000000000000, 8.938141757718215175 ) ) ;
#27962 = LINE ( 'NONE', #50360, #16897 ) ;
#27963 = ORIENTED_EDGE ( 'NONE', *, *, #8043, .F. ) ;
#27964 = DIRECTION ( 'NONE',  ( -0.5449076811759708816, 0.6444004775717707689, 0.5364919789714475140 ) ) ;
#27965 = LINE ( 'NONE', #48707, #47617 ) ;
#27966 = ORIENTED_EDGE ( 'NONE', *, *, #34271, .T. ) ;
#27967 = CARTESIAN_POINT ( 'NONE',  ( -70.07530963300145288, 1.999999999999999112, -7.815307374640574345 ) ) ;
#27968 = FACE_OUTER_BOUND ( 'NONE', #24795, .T. ) ;
#27969 = CARTESIAN_POINT ( 'NONE',  ( -11.87243407472968926, 0.000000000000000000, 11.50246268866867361 ) ) ;
#27970 = LINE ( 'NONE', #31931, #5130 ) ;
#27971 = DIRECTION ( 'NONE',  ( 0.5364919789714477361, 0.6444004775717706579, 0.5449076811759711036 ) ) ;
#27972 = VERTEX_POINT ( 'NONE', #26612 ) ;
#27973 = VERTEX_POINT ( 'NONE', #52464 ) ;
#27974 = LINE ( 'NONE', #28809, #29391 ) ;
#27975 = CARTESIAN_POINT ( 'NONE',  ( -16.28489267888972591, 0.000000000000000000, 7.109672800269438042 ) ) ;
#27976 = DIRECTION ( 'NONE',  ( 0.5364919789714477361, 0.6444004775717706579, 0.5449076811759711036 ) ) ;
#27977 = EDGE_CURVE ( 'NONE', #2279, #10694, #22918, .T. ) ;
#27978 = EDGE_CURVE ( 'NONE', #3951, #51394, #39410, .T. ) ;
#27979 = VECTOR ( 'NONE', #13223, 1000.000000000000227 ) ;
#27980 = CARTESIAN_POINT ( 'NONE',  ( 5.850167639498142336, 0.0001172167714158106350, -1.544991171441945532 ) ) ;
#27981 = DIRECTION ( 'NONE',  ( 0.9999697198139515519, 0.000000000000000000, 0.007781995580013368816 ) ) ;
#27983 = EDGE_CURVE ( 'NONE', #52378, #46741, #5055, .T. ) ;
#27982 = VERTEX_POINT ( 'NONE', #26920 ) ;
#27984 = DIRECTION ( 'NONE',  ( 0.005002170337468016433, -0.7660444431189770143, -0.6427681459581293666 ) ) ;
#27985 = DIRECTION ( 'NONE',  ( 0.007781995580012663651, -3.146120232559066537E-19, -0.9999697198139514409 ) ) ;
#27986 = PLANE ( 'NONE',  #48680 ) ;
#27987 = EDGE_LOOP ( 'NONE', ( #44407, #164, #25086, #53803 ) ) ;
#27988 = CARTESIAN_POINT ( 'NONE',  ( -29.86197018149027116, 0.000000000000000000, 8.281335066757780083 ) ) ;
#27989 = EDGE_LOOP ( 'NONE', ( #34336, #15238, #41106, #48089 ) ) ;
#27990 = CARTESIAN_POINT ( 'NONE',  ( -27.99923088623136636, 0.000000000000000000, 7.757173251277078130 ) ) ;
#27991 = CARTESIAN_POINT ( 'NONE',  ( -19.94248935626058383, 3.038739411681508518, 4.331320150471698049 ) ) ;
#27992 = ORIENTED_EDGE ( 'NONE', *, *, #50598, .T. ) ;
#27993 = DIRECTION ( 'NONE',  ( 0.007781995580012663651, -3.146120232559066537E-19, -0.9999697198139514409 ) ) ;
#27994 = ORIENTED_EDGE ( 'NONE', *, *, #51269, .F. ) ;
#27995 = ORIENTED_EDGE ( 'NONE', *, *, #19157, .F. ) ;
#27996 = ORIENTED_EDGE ( 'NONE', *, *, #48168, .F. ) ;
#27997 = CARTESIAN_POINT ( 'NONE',  ( -27.06552663992790997, 0.000000000000000000, 7.195101427592543786 ) ) ;
#27998 = ORIENTED_EDGE ( 'NONE', *, *, #438, .T. ) ;
#27999 = EDGE_CURVE ( 'NONE', #931, #33376, #30873, .T. ) ;
#28000 = ORIENTED_EDGE ( 'NONE', *, *, #46752, .T. ) ;
#28001 = LINE ( 'NONE', #23184, #33814 ) ;
#28002 = ORIENTED_EDGE ( 'NONE', *, *, #21110, .T. ) ;
#28003 = ADVANCED_FACE ( 'NONE', ( #22383 ), #27178, .F. ) ;
#28004 = ORIENTED_EDGE ( 'NONE', *, *, #1547, .F. ) ;
#28005 = DIRECTION ( 'NONE',  ( -0.5364919789714478471, 0.6444004775717705469, -0.5449076811759709926 ) ) ;
#28006 = ORIENTED_EDGE ( 'NONE', *, *, #15907, .F. ) ;
#28007 = VERTEX_POINT ( 'NONE', #35420 ) ;
#28008 = CARTESIAN_POINT ( 'NONE',  ( -13.03818250801268341, 0.000000000000000000, 7.873603589161035643 ) ) ;
#28009 = LINE ( 'NONE', #22626, #17607 ) ;
#28010 = LINE ( 'NONE', #45062, #53197 ) ;
#28011 = DIRECTION ( 'NONE',  ( -0.5449076811759708816, 0.6444004775717707689, 0.5364919789714475140 ) ) ;
#28012 = EDGE_CURVE ( 'NONE', #33376, #23572, #44778, .T. ) ;
#28013 = EDGE_LOOP ( 'NONE', ( #36003, #47217, #27664, #31334 ) ) ;
#28014 = DIRECTION ( 'NONE',  ( 0.000000000000000000, -0.000000000000000000, -1.000000000000000000 ) ) ;
#28015 = ORIENTED_EDGE ( 'NONE', *, *, #36547, .F. ) ;
#28016 = VECTOR ( 'NONE', #25629, 999.9999999999998863 ) ;
#28017 = ORIENTED_EDGE ( 'NONE', *, *, #19082, .T. ) ;
#28018 = CARTESIAN_POINT ( 'NONE',  ( -19.42910703681909368, 21.15220053346460816, -4.255330291692488665 ) ) ;
#28019 = UNCERTAINTY_MEASURE_WITH_UNIT (LENGTH_MEASURE( 1.000000000000000082E-05 ), #43780, 'distance_accuracy_value', 'NONE');
#28020 = LINE ( 'NONE', #24308, #31510 ) ;
#28021 = CARTESIAN_POINT ( 'NONE',  ( -12.12982302922070943, -2.298917212465658721, 1.519608817024182823 ) ) ;
#28022 = LINE ( 'NONE', #44771, #23933 ) ;
#28023 = LINE ( 'NONE', #15245, #50364 ) ;
#28024 = ORIENTED_EDGE ( 'NONE', *, *, #141, .F. ) ;
#28025 = PLANE ( 'NONE',  #5713 ) ;
#28026 = ORIENTED_EDGE ( 'NONE', *, *, #10563, .T. ) ;
#28027 = CARTESIAN_POINT ( 'NONE',  ( -9.486592635183393796, 0.000000000000000000, 3.469258045095933607 ) ) ;
#28028 = CARTESIAN_POINT ( 'NONE',  ( -11.40636015113596180, 0.000000000000000000, 11.32142374880780089 ) ) ;
#28029 = CARTESIAN_POINT ( 'NONE',  ( -11.77243710274829525, -0.1191753592594197858, 11.50324088822667612 ) ) ;
#28030 = PLANE ( 'NONE',  #48563 ) ;
#28031 = CARTESIAN_POINT ( 'NONE',  ( -25.20278734466900517, 0.000000000000000000, 6.670939612111840944 ) ) ;
#28032 = ORIENTED_EDGE ( 'NONE', *, *, #13043, .T. ) ;
#28033 = LINE ( 'NONE', #1884, #43010 ) ;
#28034 = DIRECTION ( 'NONE',  ( 0.6246952433987894571, -0.7422098413412800966, -0.2426528472758541777 ) ) ;
#28035 = DIRECTION ( 'NONE',  ( 0.000000000000000000, -1.000000000000000000, 0.000000000000000000 ) ) ;
#28036 = EDGE_CURVE ( 'NONE', #17736, #46146, #49032, .T. ) ;
#28037 = DIRECTION ( 'NONE',  ( -0.6427681459581293666, -0.7660444431189770143, -0.005002170337467561935 ) ) ;
#28038 = DIRECTION ( 'NONE',  ( 0.000000000000000000, -0.000000000000000000, -1.000000000000000000 ) ) ;
#28039 = EDGE_CURVE ( 'NONE', #34678, #13391, #34869, .T. ) ;
#28040 = CARTESIAN_POINT ( 'NONE',  ( -29.86352658060627618, 0.000000000000000000, 8.481329010720569883 ) ) ;
#28041 = ADVANCED_FACE ( 'NONE', ( #1039, #48477 ), #52181, .F. ) ;
#28042 = DIRECTION ( 'NONE',  ( 0.6427681459581294776, -0.7660444431189769032, 0.005002170337467562802 ) ) ;
#28043 = CARTESIAN_POINT ( 'NONE',  ( 0.000000000000000000, 3.800000000000002043, -2.749999999999994671 ) ) ;
#28044 = LINE ( 'NONE', #45348, #45548 ) ;
#28045 = ORIENTED_EDGE ( 'NONE', *, *, #34269, .T. ) ;
#28046 = VECTOR ( 'NONE', #2306, 1000.000000000000227 ) ;
#28047 = ORIENTED_EDGE ( 'NONE', *, *, #2710, .T. ) ;
#28048 = ORIENTED_EDGE ( 'NONE', *, *, #52496, .T. ) ;
#28049 = ORIENTED_EDGE ( 'NONE', *, *, #16723, .F. ) ;
#28050 = EDGE_LOOP ( 'NONE', ( #13310, #27488, #6723, #47580, #27954, #16654, #688, #9175 ) ) ;
#28051 = EDGE_LOOP ( 'NONE', ( #5094, #27665, #16893, #36557 ) ) ;
#28052 = CARTESIAN_POINT ( 'NONE',  ( -16.79925329029790149, 0.000000000000000000, 13.49544742625427496 ) ) ;
#28053 = LINE ( 'NONE', #23772, #33963 ) ;
#28054 = ORIENTED_EDGE ( 'NONE', *, *, #41614, .F. ) ;
#28055 = CARTESIAN_POINT ( 'NONE',  ( -10.49509204652727234, -0.3560938001956556742, 0.9466100262968846213 ) ) ;
#28056 = ORIENTED_EDGE ( 'NONE', *, *, #37400, .T. ) ;
#28057 = ADVANCED_FACE ( 'NONE', ( #18367 ), #13300, .F. ) ;
#28058 = PLANE ( 'NONE',  #54642 ) ;
#28059 = EDGE_CURVE ( 'NONE', #35551, #55216, #26329, .T. ) ;
#28060 = DIRECTION ( 'NONE',  ( 0.000000000000000000, -1.000000000000000000, 0.000000000000000000 ) ) ;
#28061 = CARTESIAN_POINT ( 'NONE',  ( -15.99570089885316015, 0.000000000000000000, 3.957260742896541839 ) ) ;
#28062 = ORIENTED_EDGE ( 'NONE', *, *, #52201, .T. ) ;
#28063 = CARTESIAN_POINT ( 'NONE',  ( -14.01701317841955508, 0.000000000000000000, 2.326005055450897085 ) ) ;
#28064 = PLANE ( 'NONE',  #38211 ) ;
#28065 = EDGE_CURVE ( 'NONE', #3615, #19197, #501, .T. ) ;
#28066 = FACE_OUTER_BOUND ( 'NONE', #32761, .T. ) ;
#28067 = LINE ( 'NONE', #32352, #30929 ) ;
#28068 = CARTESIAN_POINT ( 'NONE',  ( -14.80158947260792424, -3.756034771668160577, 8.595664701519920570 ) ) ;
#28069 = CARTESIAN_POINT ( 'NONE',  ( -17.68299507730753817, 0.000000000000000000, 7.637450527518151233 ) ) ;
#28070 = FACE_OUTER_BOUND ( 'NONE', #7969, .T. ) ;
#28071 = FACE_OUTER_BOUND ( 'NONE', #14567, .T. ) ;
#28072 = FACE_OUTER_BOUND ( 'NONE', #22589, .T. ) ;
#28073 = ORIENTED_EDGE ( 'NONE', *, *, #8216, .F. ) ;
#28074 = LINE ( 'NONE', #19262, #55517 ) ;
#28075 = ORIENTED_EDGE ( 'NONE', *, *, #4512, .T. ) ;
#28076 = PRODUCT_DEFINITION_FORMATION_WITH_SPECIFIED_SOURCE ( 'ANY', '', #22381, .NOT_KNOWN. ) ;
#28077 = CARTESIAN_POINT ( 'NONE',  ( -10.89331719411706523, 0.000000000000000000, 5.104964882117939418 ) ) ;
#28078 = LINE ( 'NONE', #32887, #35928 ) ;
#28079 = PLANE ( 'NONE',  #43996 ) ;
#28080 = DIRECTION ( 'NONE',  ( 0.005961354470445682716, -0.6427876096865404731, -0.7660212471507180654 ) ) ;
#28081 = DIRECTION ( 'NONE',  ( -0.5449076811759708816, 0.6444004775717707689, 0.5364919789714475140 ) ) ;
#28082 = CARTESIAN_POINT ( 'NONE',  ( -17.73140113748535285, 0.000000000000000000, 13.85752530597602039 ) ) ;
#28084 = EDGE_CURVE ( 'NONE', #48176, #26974, #32822, .T. ) ;
#28083 = CARTESIAN_POINT ( 'NONE',  ( -17.66155904838128166, 0.000000000000000000, 4.882966845418824420 ) ) ;
#28085 = DIRECTION ( 'NONE',  ( 0.000000000000000000, -0.000000000000000000, -1.000000000000000000 ) ) ;
#28086 =( NAMED_UNIT ( * ) PLANE_ANGLE_UNIT ( ) SI_UNIT ( $, .RADIAN. ) );
#28087 = CARTESIAN_POINT ( 'NONE',  ( -31.72626587586518099, 0.000000000000000000, 9.005490826201270949 ) ) ;
#28088 = DIRECTION ( 'NONE',  ( 0.9999697198139515519, 0.000000000000000000, 0.007781995580013368816 ) ) ;
#28089 = LINE ( 'NONE', #49103, #2228 ) ;
#28090 = EDGE_CURVE ( 'NONE', #37185, #41455, #33125, .T. ) ;
#28091 = LINE ( 'NONE', #15313, #53595 ) ;
#28092 = CARTESIAN_POINT ( 'NONE',  ( -11.58491270165622922, -1.651309408375658760, 1.328609220115083644 ) ) ;
#28093 = ADVANCED_FACE ( 'NONE', ( #20032 ), #37101, .F. ) ;
#28094 = DIRECTION ( 'NONE',  ( -0.9999697198139514409, -0.000000000000000000, -0.007781995580013368816 ) ) ;
#28095 = CARTESIAN_POINT ( 'NONE',  ( -17.66816326098766865, 1.419719901456505395, 6.074237969063971398 ) ) ;
#28096 = DIRECTION ( 'NONE',  ( 0.9999697198139515519, 0.000000000000000000, 0.007781995580013368816 ) ) ;
#28097 = EDGE_CURVE ( 'NONE', #16052, #29890, #32300, .T. ) ;
#28098 = CARTESIAN_POINT ( 'NONE',  ( -11.13209366544781354, 0.000000000000000000, 1.779118040146054014 ) ) ;
#28099 = VERTEX_POINT ( 'NONE', #27759 ) ;
#28100 = ORIENTED_EDGE ( 'NONE', *, *, #36857, .T. ) ;
#28101 = FACE_OUTER_BOUND ( 'NONE', #3090, .T. ) ;
#28102 = FACE_OUTER_BOUND ( 'NONE', #18194, .T. ) ;
#28103 = EDGE_CURVE ( 'NONE', #2289, #34545, #40804, .T. ) ;
#28104 = ORIENTED_EDGE ( 'NONE', *, *, #7256, .F. ) ;
#28105 = DIRECTION ( 'NONE',  ( 0.9999697198139515519, 0.000000000000000000, 0.007781995580013368816 ) ) ;
#28106 = ORIENTED_EDGE ( 'NONE', *, *, #49315, .F. ) ;
#28107 = CARTESIAN_POINT ( 'NONE',  ( -14.46888367232926420, 0.000000000000000000, 12.59025272694991315 ) ) ;
#28108 = ADVANCED_FACE ( 'NONE', ( #50136 ), #54399, .F. ) ;
#28109 = AXIS2_PLACEMENT_3D ( 'NONE', #12721, #503, #39412 ) ;
#28110 = ORIENTED_EDGE ( 'NONE', *, *, #31225, .T. ) ;
#28111 = EDGE_LOOP ( 'NONE', ( #45930, #28795, #33001, #49481 ) ) ;
#28112 = ORIENTED_EDGE ( 'NONE', *, *, #14486, .F. ) ;
#28113 = DIRECTION ( 'NONE',  ( 0.7660212471507180654, -0.6427876096865404731, 0.005961354470445141482 ) ) ;
#28114 = CARTESIAN_POINT ( 'NONE',  ( -19.27977376529886655, 0.000000000000000000, 7.994356096355883068 ) ) ;
#28115 = CARTESIAN_POINT ( 'NONE',  ( -9.808144436391993182, 0.000000000000000000, 10.77986332834118777 ) ) ;
#28116 = EDGE_LOOP ( 'NONE', ( #1239, #21698, #44447, #19935 ) ) ;
#28117 = ORIENTED_EDGE ( 'NONE', *, *, #12449, .F. ) ;
#28118 = DIRECTION ( 'NONE',  ( 0.5449076811759707706, 0.6444004775717708799, -0.5364919789714476250 ) ) ;
#28119 = ORIENTED_EDGE ( 'NONE', *, *, #3320, .T. ) ;
#28120 = DIRECTION ( 'NONE',  ( -0.005002170337468016433, -0.7660444431189770143, 0.6427681459581293666 ) ) ;
#28121 = VERTEX_POINT ( 'NONE', #1877 ) ;
#28122 = LINE ( 'NONE', #15085, #44846 ) ;
#28123 = DIRECTION ( 'NONE',  ( 0.5449076811759707706, 0.6444004775717708799, -0.5364919789714476250 ) ) ;
#28124 = ORIENTED_EDGE ( 'NONE', *, *, #1447, .T. ) ;
#28125 = FACE_OUTER_BOUND ( 'NONE', #26448, .T. ) ;
#28126 = EDGE_CURVE ( 'NONE', #29102, #31757, #37355, .T. ) ;
#28127 = CARTESIAN_POINT ( 'NONE',  ( -16.99924723426068951, 0.000000000000000000, 13.49389102713827171 ) ) ;
#28128 = EDGE_CURVE ( 'NONE', #6316, #30378, #28574, .T. ) ;
#28129 = VERTEX_POINT ( 'NONE', #45898 ) ;
#28130 = LINE ( 'NONE', #28712, #19481 ) ;
#28131 = PLANE ( 'NONE',  #45701 ) ;
#28132 = PLANE ( 'NONE',  #40077 ) ;
#28133 = ORIENTED_EDGE ( 'NONE', *, *, #4015, .F. ) ;
#28134 = ADVANCED_FACE ( 'NONE', ( #7014 ), #41625, .F. ) ;
#28135 = CARTESIAN_POINT ( 'NONE',  ( -14.23769985819993522, 4.495856970884011261, 9.790194479452477339 ) ) ;
#28136 = CARTESIAN_POINT ( 'NONE',  ( -21.93104030566808049, -3.917936722690659401, 11.63069420620037242 ) ) ;
#28137 = FACE_OUTER_BOUND ( 'NONE', #5400, .T. ) ;
#28138 = CARTESIAN_POINT ( 'NONE',  ( -16.81345671998191449, 0.000000000000000000, 3.412238694616132495 ) ) ;
#28139 = EDGE_CURVE ( 'NONE', #50963, #53576, #36271, .T. ) ;
#28140 = DIRECTION ( 'NONE',  ( 0.9999697198139515519, 0.000000000000000000, 0.007781995580013368816 ) ) ;
#28142 = ADVANCED_FACE ( 'NONE', ( #31997 ), #46162, .F. ) ;
#28141 = LINE ( 'NONE', #6301, #33370 ) ;
#28143 = VECTOR ( 'NONE', #22774, 1000.000000000000227 ) ;
#28144 = CARTESIAN_POINT ( 'NONE',  ( -10.33520963186314923, -0.1191753592594177180, 5.947975371940869671 ) ) ;
#28145 = ORIENTED_EDGE ( 'NONE', *, *, #12437, .T. ) ;
#28146 = DIRECTION ( 'NONE',  ( 0.007781995580012663651, -3.146120232559066537E-19, -0.9999697198139514409 ) ) ;
#28147 = DIRECTION ( 'NONE',  ( 0.000000000000000000, -1.000000000000000000, 0.000000000000000000 ) ) ;
#28148 = CARTESIAN_POINT ( 'NONE',  ( -68.37432498243255452, -0.6009960021135252184, -5.589544126886995201 ) ) ;
#28149 = ORIENTED_EDGE ( 'NONE', *, *, #53244, .F. ) ;
#28150 = LINE ( 'NONE', #15939, #42879 ) ;
#28151 = CARTESIAN_POINT ( 'NONE',  ( -16.53317331066696383, 0.000000000000000000, 13.31285208727739899 ) ) ;
#28152 = ADVANCED_FACE ( 'NONE', ( #2458 ), #53847, .T. ) ;
#28153 = CARTESIAN_POINT ( 'NONE',  ( -20.54049170961573267, 0.000000000000000000, 4.660556269540326646 ) ) ;
#28154 = FACE_OUTER_BOUND ( 'NONE', #25911, .T. ) ;
#28155 = EDGE_CURVE ( 'NONE', #27227, #3531, #10434, .T. ) ;
#28156 = CARTESIAN_POINT ( 'NONE',  ( -56.60439204777216560, 6.503221467314357795, 2.370703063681847134 ) ) ;
#28157 = EDGE_LOOP ( 'NONE', ( #41246, #15339, #32213, #23642 ) ) ;
#28158 = ORIENTED_EDGE ( 'NONE', *, *, #3579, .T. ) ;
#28159 = DIRECTION ( 'NONE',  ( 0.007781995580012662783, 0.000000000000000000, -0.9999697198139514409 ) ) ;
#28160 = LINE ( 'NONE', #19079, #42948 ) ;
#28161 = EDGE_CURVE ( 'NONE', #51848, #26799, #49615, .T. ) ;
#28162 = ORIENTED_EDGE ( 'NONE', *, *, #30206, .T. ) ;
#28163 = CARTESIAN_POINT ( 'NONE',  ( -12.27860572412447304, 0.000000000000000000, 3.986188037040617083 ) ) ;
#28164 = VERTEX_POINT ( 'NONE', #28027 ) ;
#28165 = LINE ( 'NONE', #54289, #41050 ) ;
#28166 = ADVANCED_FACE ( 'NONE', ( #15250 ), #10966, .F. ) ;
#28167 = ORIENTED_EDGE ( 'NONE', *, *, #10634, .F. ) ;
#28168 = ORIENTED_EDGE ( 'NONE', *, *, #47067, .F. ) ;
#28169 = DIRECTION ( 'NONE',  ( -0.6427681459581293666, -0.7660444431189770143, -0.005002170337467561935 ) ) ;
#28170 = CARTESIAN_POINT ( 'NONE',  ( -20.96378235145114388, -1.165603555308157846, 4.987177259511585525 ) ) ;
#28171 = DIRECTION ( 'NONE',  ( 0.6427681459581294776, -0.7660444431189769032, 0.005002170337467562802 ) ) ;
#28172 = ORIENTED_EDGE ( 'NONE', *, *, #21055, .F. ) ;
#28174 = DIRECTION ( 'NONE',  ( -0.005002170337468016433, -0.7660444431189770143, 0.6427681459581293666 ) ) ;
#28173 = VECTOR ( 'NONE', #22203, 1000.000000000000114 ) ;
#28175 = ORIENTED_EDGE ( 'NONE', *, *, #20109, .F. ) ;
#28176 = VECTOR ( 'NONE', #37223, 1000.000000000000227 ) ;
#28177 = ORIENTED_EDGE ( 'NONE', *, *, #28418, .F. ) ;
#28178 = ORIENTED_EDGE ( 'NONE', *, *, #33534, .T. ) ;
#28179 = DIRECTION ( 'NONE',  ( 0.007781995580012663651, 0.000000000000000000, -0.9999697198139515519 ) ) ;
#28180 = VERTEX_POINT ( 'NONE', #19779 ) ;
#28181 = FACE_OUTER_BOUND ( 'NONE', #25887, .T. ) ;
#28182 = EDGE_LOOP ( 'NONE', ( #11213, #15536, #11422, #464 ) ) ;
#28183 = DIRECTION ( 'NONE',  ( 0.6427681459581294776, -0.7660444431189769032, 0.005002170337467562802 ) ) ;
#28184 = CARTESIAN_POINT ( 'NONE',  ( -10.27421835998572064, 0.000000000000000000, 10.96090226820206048 ) ) ;
#28185 = VERTEX_POINT ( 'NONE', #42959 ) ;
#28186 = DIRECTION ( 'NONE',  ( -1.000000000000000000, 0.000000000000000000, 0.000000000000000000 ) ) ;
#28187 = EDGE_CURVE ( 'NONE', #32241, #46025, #26466, .T. ) ;
#28188 = ORIENTED_EDGE ( 'NONE', *, *, #16262, .F. ) ;
#28189 = LINE ( 'NONE', #29318, #26352 ) ;
#28190 = DIRECTION ( 'NONE',  ( -0.005002170337468016433, -0.7660444431189770143, 0.6427681459581293666 ) ) ;
#28191 = CARTESIAN_POINT ( 'NONE',  ( -14.10280672071693431, -0.1191753592594197858, 12.40843558753103792 ) ) ;
#28192 = DIRECTION ( 'NONE',  ( -0.7660212471507179544, -0.6427876096865405842, -0.005961354470445141482 ) ) ;
#28193 = CARTESIAN_POINT ( 'NONE',  ( -19.32961685222932147, 0.000000000000000000, 14.39908572644263351 ) ) ;
#28194 = DIRECTION ( 'NONE',  ( 0.5364919789714477361, 0.6444004775717706579, 0.5449076811759711036 ) ) ;
#28195 = DIRECTION ( 'NONE',  ( 0.7660212471507180654, -0.6427876096865404731, 0.005961354470445141482 ) ) ;
#28196 = ORIENTED_EDGE ( 'NONE', *, *, #25360, .F. ) ;
#28197 = EDGE_CURVE ( 'NONE', #52488, #19686, #31003, .T. ) ;
#28198 = EDGE_CURVE ( 'NONE', #11534, #43483, #41890, .T. ) ;
#28199 = EDGE_CURVE ( 'NONE', #39217, #4575, #48322, .T. ) ;
#28200 = VECTOR ( 'NONE', #36337, 1000.000000000000000 ) ;
#28201 = ORIENTED_EDGE ( 'NONE', *, *, #47935, .F. ) ;
#28202 = VECTOR ( 'NONE', #54791, 1000.000000000000000 ) ;
#28203 = CARTESIAN_POINT ( 'NONE',  ( -56.32449333261072155, 3.868143273367939727, 2.183322036886178097 ) ) ;
#28204 = DIRECTION ( 'NONE',  ( 0.000000000000000000, -0.000000000000000000, -1.000000000000000000 ) ) ;
#28205 = LINE ( 'NONE', #50050, #33074 ) ;
#28207 = ADVANCED_FACE ( 'NONE', ( #39560 ), #4903, .F. ) ;
#28206 = LINE ( 'NONE', #37570, #17032 ) ;
#28208 = CARTESIAN_POINT ( 'NONE',  ( -24.54687820731135162, 18.44472334908947175, 4.546935074492525430 ) ) ;
#28209 = ORIENTED_EDGE ( 'NONE', *, *, #11105, .F. ) ;
#28210 = LINE ( 'NONE', #49801, #46742 ) ;
#28211 = DIRECTION ( 'NONE',  ( 0.007781995580012662783, 0.000000000000000000, -0.9999697198139514409 ) ) ;
#28212 = EDGE_LOOP ( 'NONE', ( #5854, #33311, #32505, #3391 ) ) ;
#28213 = DIRECTION ( 'NONE',  ( 0.007781995580012662783, 0.000000000000000000, -0.9999697198139514409 ) ) ;
#28214 = PLANE ( 'NONE',  #13165 ) ;
#28215 = ORIENTED_EDGE ( 'NONE', *, *, #44612, .T. ) ;
#28216 = CARTESIAN_POINT ( 'NONE',  ( -70.56555449637278343, -1.000000000000001332, -8.047023921085740383 ) ) ;
#28217 = CARTESIAN_POINT ( 'NONE',  ( -25.20278734466900517, 0.000000000000000000, 6.670939612111840944 ) ) ;
#28218 = VECTOR ( 'NONE', #5947, 1000.000000000000227 ) ;
#28219 = EDGE_CURVE ( 'NONE', #29871, #42362, #21673, .T. ) ;
#28220 = DIRECTION ( 'NONE',  ( 0.6427681459581294776, -0.7660444431189769032, 0.005002170337467562802 ) ) ;
#28221 = PLANE ( 'NONE',  #51374 ) ;
#28222 = VECTOR ( 'NONE', #36616, 1000.000000000000227 ) ;
#28223 = ADVANCED_FACE ( 'NONE', ( #52337 ), #22228, .F. ) ;
#28224 = CARTESIAN_POINT ( 'NONE',  ( -14.43341085292522052, 0.000000000000000000, 8.032071613151982703 ) ) ;
#28225 = VERTEX_POINT ( 'NONE', #30181 ) ;
#28226 = ORIENTED_EDGE ( 'NONE', *, *, #797, .T. ) ;
#28227 = EDGE_CURVE ( 'NONE', #32666, #16969, #25633, .T. ) ;
#28228 = CARTESIAN_POINT ( 'NONE',  ( -13.07066190154808361, 0.000000000000000000, 12.04713590736729678 ) ) ;
#28229 = DIRECTION ( 'NONE',  ( -0.005002170337468016433, -0.7660444431189770143, 0.6427681459581293666 ) ) ;
#28230 = DIRECTION ( 'NONE',  ( -0.9999697198139514409, -0.000000000000000000, -0.007781995580013368816 ) ) ;
#28231 = CARTESIAN_POINT ( 'NONE',  ( -17.42278257705052980, 0.000000000000000000, 8.208813687390710712 ) ) ;
#28232 = EDGE_CURVE ( 'NONE', #54774, #48671, #17388, .T. ) ;
#28233 = DIRECTION ( 'NONE',  ( 0.005961354470445682716, -0.6427876096865404731, -0.7660212471507180654 ) ) ;
#28234 = DIRECTION ( 'NONE',  ( 0.007781995580012662783, 0.000000000000000000, -0.9999697198139514409 ) ) ;
#28235 = ORIENTED_EDGE ( 'NONE', *, *, #44526, .T. ) ;
#28236 = CARTESIAN_POINT ( 'NONE',  ( -10.27421835998572064, 0.000000000000000000, 10.96090226820206048 ) ) ;
#28237 = CARTESIAN_POINT ( 'NONE',  ( -12.16501668417466853, -0.1191753592594191197, 2.240414692291188725 ) ) ;
#28238 = CARTESIAN_POINT ( 'NONE',  ( -13.53673582514181106, 0.000000000000000000, 12.22817484722816772 ) ) ;
#28239 = EDGE_LOOP ( 'NONE', ( #26783, #6704, #7273, #53473, #36704, #31201, #10036, #43322 ) ) ;
#28240 = DIRECTION ( 'NONE',  ( -0.6427681459581293666, -0.7660444431189770143, -0.005002170337467561935 ) ) ;
#28241 = CARTESIAN_POINT ( 'NONE',  ( -22.02230666951336246, 19.67040017278726438, 4.420763615217817133 ) ) ;
#28242 = PLANE ( 'NONE',  #12100 ) ;
#28243 = ORIENTED_EDGE ( 'NONE', *, *, #14738, .T. ) ;
#28244 = VECTOR ( 'NONE', #36217, 999.9999999999998863 ) ;
#28245 = VECTOR ( 'NONE', #46862, 999.9999999999998863 ) ;
#28246 = CARTESIAN_POINT ( 'NONE',  ( -20.11779259742415249, -3.432230869623158487, 10.12924116631567273 ) ) ;
#28247 = VERTEX_POINT ( 'NONE', #47209 ) ;
#28248 = ORIENTED_EDGE ( 'NONE', *, *, #18901, .T. ) ;
#28249 = ORIENTED_EDGE ( 'NONE', *, *, #18032, .F. ) ;
#28250 = VERTEX_POINT ( 'NONE', #4365 ) ;
#28251 = VECTOR ( 'NONE', #29043, 1000.000000000000227 ) ;
#28252 = EDGE_LOOP ( 'NONE', ( #17131, #25741, #701, #8955 ) ) ;
#28253 = CARTESIAN_POINT ( 'NONE',  ( -16.72078904067797822, 0.000000000000000000, 3.412959855923785923 ) ) ;
#28255 = ADVANCED_FACE ( 'NONE', ( #52594 ), #17687, .F. ) ;
#28254 = ORIENTED_EDGE ( 'NONE', *, *, #53615, .T. ) ;
#28256 = ORIENTED_EDGE ( 'NONE', *, *, #49424, .F. ) ;
#28257 = LINE ( 'NONE', #41602, #10493 ) ;
#28258 = ORIENTED_EDGE ( 'NONE', *, *, #41091, .F. ) ;
#28259 = ADVANCED_FACE ( 'NONE', ( #56037 ), #30757, .F. ) ;
#28260 = EDGE_LOOP ( 'NONE', ( #49832, #7849, #55789, #8522 ) ) ;
#28261 = VECTOR ( 'NONE', #5632, 1000.000000000000227 ) ;
#28262 = ORIENTED_EDGE ( 'NONE', *, *, #6221, .T. ) ;
#28263 = CARTESIAN_POINT ( 'NONE',  ( -13.08408713167409942, -0.1191753592594197858, 1.863930203747758085 ) ) ;
#28264 = CARTESIAN_POINT ( 'NONE',  ( -3.360905869600907092, 1.745854407020028306E-14, 3.600000000000000089 ) ) ;
#28265 = CARTESIAN_POINT ( 'NONE',  ( -56.20083583094844926, 4.876814673940706335, -3.000000000000007105 ) ) ;
#28266 = DIRECTION ( 'NONE',  ( 0.3620778797217453771, -0.000000000000000000, 0.9321478471874541372 ) ) ;
#28267 = ORIENTED_EDGE ( 'NONE', *, *, #37009, .F. ) ;
#28268 = DIRECTION ( 'NONE',  ( 0.007781995580012663651, 0.000000000000000000, -0.9999697198139515519 ) ) ;
#28269 = ORIENTED_EDGE ( 'NONE', *, *, #40352, .T. ) ;
#28270 = EDGE_CURVE ( 'NONE', #19153, #46212, #33403, .T. ) ;
#28271 = ADVANCED_FACE ( 'NONE', ( #11799 ), #17129, .F. ) ;
#28272 = EDGE_CURVE ( 'NONE', #36112, #33164, #51750, .T. ) ;
#28273 = ORIENTED_EDGE ( 'NONE', *, *, #33235, .F. ) ;
#28274 = DIRECTION ( 'NONE',  ( 0.000000000000000000, 0.000000000000000000, 1.000000000000000000 ) ) ;
#28275 = EDGE_CURVE ( 'NONE', #9690, #37705, #8612, .T. ) ;
#28276 = DIRECTION ( 'NONE',  ( 0.9321478471874541372, 0.000000000000000000, -0.3620778797217453771 ) ) ;
#28277 = LINE ( 'NONE', #14955, #9473 ) ;
#28278 = LINE ( 'NONE', #14132, #13965 ) ;
#28279 = CARTESIAN_POINT ( 'NONE',  ( -20.26176469941677993, 0.000000000000000000, 14.76116360616437895 ) ) ;
#28280 = ORIENTED_EDGE ( 'NONE', *, *, #13963, .F. ) ;
#28281 = DIRECTION ( 'NONE',  ( -0.000000000000000000, -1.000000000000000000, -0.000000000000000000 ) ) ;
#28282 = ORIENTED_EDGE ( 'NONE', *, *, #14136, .F. ) ;
#28283 = VECTOR ( 'NONE', #1501, 1000.000000000000227 ) ;
#28284 = VECTOR ( 'NONE', #56023, 1000.000000000000227 ) ;
#28285 = CARTESIAN_POINT ( 'NONE',  ( -15.86710544311044302, 0.000000000000000000, 13.13336954653252953 ) ) ;
#28286 = CARTESIAN_POINT ( 'NONE',  ( -24.96676581047183063, 18.24370688441070953, -4.565775476651154463 ) ) ;
#28287 = CARTESIAN_POINT ( 'NONE',  ( -10.67033082211201567, 0.000000000000000000, 2.152043655171826497 ) ) ;
#28288 = DIRECTION ( 'NONE',  ( 0.007781995580012662783, 0.000000000000000000, -0.9999697198139514409 ) ) ;
#28289 = PLANE ( 'NONE',  #5984 ) ;
#28290 = VECTOR ( 'NONE', #30097, 999.9999999999998863 ) ;
#28291 = ORIENTED_EDGE ( 'NONE', *, *, #11846, .F. ) ;
#28292 = EDGE_CURVE ( 'NONE', #46770, #52665, #38986, .T. ) ;
#28293 = DIRECTION ( 'NONE',  ( -0.1139275668495183524, 0.9934890585767659488, 4.694855797473114533E-16 ) ) ;
#28294 = PLANE ( 'NONE',  #19468 ) ;
#28295 = CARTESIAN_POINT ( 'NONE',  ( -17.82130721938061413, -0.03739765774599677212, 3.742346127740344031 ) ) ;
#28296 = EDGE_CURVE ( 'NONE', #14051, #17689, #8909, .T. ) ;
#28297 = DIRECTION ( 'NONE',  ( -0.005002170337468016433, -0.7660444431189770143, 0.6427681459581293666 ) ) ;
#28298 = VECTOR ( 'NONE', #15537, 1000.000000000000114 ) ;
#28299 = CARTESIAN_POINT ( 'NONE',  ( -16.33317936670417225, 0.000000000000000000, 13.31440848639340224 ) ) ;
#28300 = LINE ( 'NONE', #6199, #50851 ) ;
#28301 = CARTESIAN_POINT ( 'NONE',  ( -12.33850799832341849, 0.000000000000000000, 11.68350162852954632 ) ) ;
#28302 = ADVANCED_FACE ( 'NONE', ( #31599 ), #1181, .F. ) ;
#28303 = AXIS2_PLACEMENT_3D ( 'NONE', #46632, #37554, #33321 ) ;
#28304 = FACE_OUTER_BOUND ( 'NONE', #45041, .T. ) ;
#28305 = CARTESIAN_POINT ( 'NONE',  ( -27.06630483948590893, -0.1191753592594197858, 7.295098399573937797 ) ) ;
#28306 = ORIENTED_EDGE ( 'NONE', *, *, #40884, .T. ) ;
#28307 = VECTOR ( 'NONE', #30765, 1000.000000000000114 ) ;
#28308 = EDGE_LOOP ( 'NONE', ( #36037, #8276, #49644, #23566 ) ) ;
#28309 = ORIENTED_EDGE ( 'NONE', *, *, #30967, .T. ) ;
#28310 = ORIENTED_EDGE ( 'NONE', *, *, #9315, .T. ) ;
#28311 = VERTEX_POINT ( 'NONE', #36142 ) ;
#28312 = VECTOR ( 'NONE', #5063, 1000.000000000000227 ) ;
#28313 = CARTESIAN_POINT ( 'NONE',  ( -17.74404816805336793, 0.000000000000000000, 3.574322630375089460 ) ) ;
#28314 = DIRECTION ( 'NONE',  ( 0.6427681459581294776, -0.7660444431189769032, 0.005002170337467562802 ) ) ;
#28315 = AXIS2_PLACEMENT_3D ( 'NONE', #40407, #31612, #48920 ) ;
#28316 = VECTOR ( 'NONE', #28977, 999.9999999999998863 ) ;
#28317 = ORIENTED_EDGE ( 'NONE', *, *, #41092, .F. ) ;
#28318 = CARTESIAN_POINT ( 'NONE',  ( -57.29829478218162109, -10.27834239552269580, -2.999999999999996891 ) ) ;
#28319 = ORIENTED_EDGE ( 'NONE', *, *, #29314, .F. ) ;
#28320 = ORIENTED_EDGE ( 'NONE', *, *, #25440, .T. ) ;
#28321 = VECTOR ( 'NONE', #36861, 1000.000000000000227 ) ;
#28322 = VECTOR ( 'NONE', #44485, 1000.000000000000227 ) ;
#28323 = CARTESIAN_POINT ( 'NONE',  ( -68.64911863573352946, -9.566881861030363865, 7.932749270814273501 ) ) ;
#28324 = LINE ( 'NONE', #11586, #49097 ) ;
#28325 = CARTESIAN_POINT ( 'NONE',  ( -13.17065887352947762, -0.1191753592594197858, 12.04635770780929427 ) ) ;
#28326 = ORIENTED_EDGE ( 'NONE', *, *, #50659, .T. ) ;
#28327 = DIRECTION ( 'NONE',  ( 0.005002170337468016433, -0.7660444431189770143, -0.6427681459581293666 ) ) ;
#28328 = ADVANCED_FACE ( 'NONE', ( #53705 ), #27901, .F. ) ;
#28329 = CARTESIAN_POINT ( 'NONE',  ( -23.33849165029409889, 0.000000000000000000, 5.946783852668351855 ) ) ;
#28330 = DIRECTION ( 'NONE',  ( 0.005002170337468016433, -0.7660444431189770143, -0.6427681459581293666 ) ) ;
#28331 = EDGE_CURVE ( 'NONE', #36770, #34091, #14541, .T. ) ;
#28332 = ADVANCED_FACE ( 'NONE', ( #22517 ), #23356, .F. ) ;
#28333 = LINE ( 'NONE', #36890, #45433 ) ;
#28334 = CARTESIAN_POINT ( 'NONE',  ( -16.87007711150675959, -1.813211359398158473, 6.210631339198578793 ) ) ;
#28335 = CARTESIAN_POINT ( 'NONE',  ( -11.09304826722767956, 24.43504809471621186, 5.000000000000000888 ) ) ;
#28336 = CARTESIAN_POINT ( 'NONE',  ( -17.74560456716937296, 0.000000000000000000, 3.774316574337878372 ) ) ;
#28337 = CARTESIAN_POINT ( 'NONE',  ( -18.67775241435682432, 0.000000000000000000, 4.136394454059623804 ) ) ;
#28338 = DIRECTION ( 'NONE',  ( -0.6427681459581293666, -0.7660444431189770143, -0.005002170337467561935 ) ) ;
#28339 = EDGE_LOOP ( 'NONE', ( #29823, #23535, #52978, #13474 ) ) ;
#28340 = CARTESIAN_POINT ( 'NONE',  ( -8.834775662789930095, 0.000000000000000000, 5.120984928305981398 ) ) ;
#28341 = ORIENTED_EDGE ( 'NONE', *, *, #48391, .F. ) ;
#28342 = CARTESIAN_POINT ( 'NONE',  ( -13.08330893211609869, 0.000000000000000000, 1.763933231766363630 ) ) ;
#28343 = LINE ( 'NONE', #41434, #44999 ) ;
#28344 = PLANE ( 'NONE',  #6007 ) ;
#28345 = AXIS2_PLACEMENT_3D ( 'NONE', #16024, #11181, #23682 ) ;
#28346 = CARTESIAN_POINT ( 'NONE',  ( -20.63663879154963965, 20.74370688441071664, -4.657437592157546824 ) ) ;
#28347 = DIRECTION ( 'NONE',  ( -0.5449076811759708816, 0.6444004775717707689, 0.5364919789714475140 ) ) ;
#28348 = DIRECTION ( 'NONE',  ( 0.007781995580012663651, -3.146120232559066537E-19, -0.9999697198139514409 ) ) ;
#28349 = SURFACE_STYLE_FILL_AREA ( #55061 ) ;
#28350 = LINE ( 'NONE', #45393, #15120 ) ;
#28351 = VECTOR ( 'NONE', #32242, 1000.000000000000114 ) ;
#28352 = PLANE ( 'NONE',  #52939 ) ;
#28353 = DIRECTION ( 'NONE',  ( 0.6427681459581294776, -0.7660444431189769032, 0.005002170337467562802 ) ) ;
#28354 = LINE ( 'NONE', #45677, #36371 ) ;
#28355 = LINE ( 'NONE', #28092, #24162 ) ;
#28356 = VECTOR ( 'NONE', #39719, 999.9999999999998863 ) ;
#28357 = VECTOR ( 'NONE', #6440, 999.9999999999998863 ) ;
#28358 = PLANE ( 'NONE',  #41807 ) ;
#28359 = CARTESIAN_POINT ( 'NONE',  ( -16.53182346927628643, 3.362543313726509719, 8.821349211107063937 ) ) ;
#28360 = EDGE_CURVE ( 'NONE', #47771, #25044, #10000, .T. ) ;
#28361 = CARTESIAN_POINT ( 'NONE',  ( -17.74560456716937296, 0.000000000000000000, 3.774316574337878372 ) ) ;
#28362 = DIRECTION ( 'NONE',  ( 0.007781995580012662783, 0.000000000000000000, -0.9999697198139514409 ) ) ;
#28363 = ORIENTED_EDGE ( 'NONE', *, *, #12117, .T. ) ;
#28364 = VECTOR ( 'NONE', #14563, 999.9999999999998863 ) ;
#28365 = DIRECTION ( 'NONE',  ( 0.007781995580012662783, 0.000000000000000000, -0.9999697198139514409 ) ) ;
#28366 = VECTOR ( 'NONE', #23540, 1000.000000000000227 ) ;
#28367 = ORIENTED_EDGE ( 'NONE', *, *, #33000, .T. ) ;
#28368 = EDGE_CURVE ( 'NONE', #24940, #26440, #18821, .T. ) ;
#28369 = DIRECTION ( 'NONE',  ( 0.007781995580012663651, 0.000000000000000000, -0.9999697198139515519 ) ) ;
#28370 = CARTESIAN_POINT ( 'NONE',  ( -18.71304404252910558, -0.1191753592594156086, 7.729437476405517593 ) ) ;
#28371 = EDGE_CURVE ( 'NONE', #26525, #55970, #44359, .T. ) ;
#28372 = VERTEX_POINT ( 'NONE', #19069 ) ;
#28373 = EDGE_CURVE ( 'NONE', #26092, #4219, #36566, .T. ) ;
#28374 = AXIS2_PLACEMENT_3D ( 'NONE', #21531, #47070, #29772 ) ;
#28375 = ORIENTED_EDGE ( 'NONE', *, *, #46672, .T. ) ;
#28376 = DIRECTION ( 'NONE',  ( 0.007781995580012663651, 0.000000000000000000, -0.9999697198139515519 ) ) ;
#28377 = AXIS2_PLACEMENT_3D ( 'NONE', #36240, #10107, #27418 ) ;
#28378 = VERTEX_POINT ( 'NONE', #5741 ) ;
#28379 = ORIENTED_EDGE ( 'NONE', *, *, #38145, .F. ) ;
#28380 = ORIENTED_EDGE ( 'NONE', *, *, #45925, .T. ) ;
#28381 = CARTESIAN_POINT ( 'NONE',  ( -16.81190032086591302, 0.000000000000000000, 3.212244750653343583 ) ) ;
#28382 = FACE_OUTER_BOUND ( 'NONE', #53409, .T. ) ;
#28383 = DIRECTION ( 'NONE',  ( 0.007781995580012663651, 0.000000000000000000, -0.9999697198139515519 ) ) ;
#28384 = VECTOR ( 'NONE', #48097, 999.9999999999998863 ) ;
#28385 = VERTEX_POINT ( 'NONE', #52866 ) ;
#28386 = ORIENTED_EDGE ( 'NONE', *, *, #9837, .F. ) ;
#28387 = AXIS2_PLACEMENT_3D ( 'NONE', #3444, #20761, #55386 ) ;
#28388 = LINE ( 'NONE', #55349, #8502 ) ;
#28389 = CARTESIAN_POINT ( 'NONE',  ( -14.47385752816844473, -3.917936722690661178, 8.734071168426410736 ) ) ;
#28390 = ORIENTED_EDGE ( 'NONE', *, *, #20979, .T. ) ;
#28391 = VECTOR ( 'NONE', #602, 999.9999999999998863 ) ;
#28392 = CARTESIAN_POINT ( 'NONE',  ( -15.03495456790438389, -0.1191753592594197858, 12.77051346725278158 ) ) ;
#28393 = ADVANCED_FACE ( 'NONE', ( #18225 ), #40093, .F. ) ;
#28394 = ORIENTED_EDGE ( 'NONE', *, *, #16582, .T. ) ;
#28395 = DIRECTION ( 'NONE',  ( 0.5449076811759707706, 0.6444004775717708799, -0.5364919789714476250 ) ) ;
#28396 = DIRECTION ( 'NONE',  ( 0.9999697198139515519, 0.000000000000000000, 0.007781995580013368816 ) ) ;
#28397 = AXIS2_PLACEMENT_3D ( 'NONE', #39351, #4443, #56119 ) ;
#28398 = VECTOR ( 'NONE', #7206, 999.9999999999998863 ) ;
#28400 = EDGE_LOOP ( 'NONE', ( #33721, #33830, #25586, #48291 ) ) ;
#28399 = ADVANCED_FACE ( 'NONE', ( #39824 ), #45207, .F. ) ;
#28401 = FACE_OUTER_BOUND ( 'NONE', #48321, .T. ) ;
#28402 = EDGE_CURVE ( 'NONE', #20845, #37899, #48633, .T. ) ;
#28403 = EDGE_CURVE ( 'NONE', #24227, #12251, #2011, .T. ) ;
#28404 = AXIS2_PLACEMENT_3D ( 'NONE', #5997, #18782, #27269 ) ;
#28405 = DIRECTION ( 'NONE',  ( 0.005002170337468016433, -0.7660444431189770143, -0.6427681459581293666 ) ) ;
#28406 = AXIS2_PLACEMENT_3D ( 'NONE', #15118, #40927, #44622 ) ;
#28407 = VERTEX_POINT ( 'NONE', #53180 ) ;
#28408 = DIRECTION ( 'NONE',  ( 0.9999697198139515519, 0.000000000000000000, 0.007781995580013368816 ) ) ;
#28409 = PLANE ( 'NONE',  #21231 ) ;
#28410 = DIRECTION ( 'NONE',  ( -0.2426528472758542054, 0.7422098413412800966, -0.6246952433987894571 ) ) ;
#28411 = ORIENTED_EDGE ( 'NONE', *, *, #14823, .F. ) ;
#28412 = CARTESIAN_POINT ( 'NONE',  ( -20.54204810873173415, 0.000000000000000000, 4.860550213503115558 ) ) ;
#28413 = DIRECTION ( 'NONE',  ( 0.5449076811759707706, 0.6444004775717708799, -0.5364919789714476250 ) ) ;
#28414 = DIRECTION ( 'NONE',  ( 0.007781995580012663651, 0.000000000000000000, -0.9999697198139515519 ) ) ;
#28415 = CARTESIAN_POINT ( 'NONE',  ( -17.97681294474074676, -3.108426967578160394, 8.766194593337463203 ) ) ;
#28416 = CARTESIAN_POINT ( 'NONE',  ( -8.024318355659660895, -1.000000000000000000, 6.335291332000425157 ) ) ;
#28417 = CARTESIAN_POINT ( 'NONE',  ( -14.66887761629205222, 0.000000000000000000, 12.58869632783390990 ) ) ;
#28418 = EDGE_CURVE ( 'NONE', #34831, #56081, #49167, .T. ) ;
#28419 = CARTESIAN_POINT ( 'NONE',  ( -22.40634380310664397, 0.000000000000000000, 5.584705972946605534 ) ) ;
#28420 = VECTOR ( 'NONE', #17100, 1000.000000000000000 ) ;
#28421 = ORIENTED_EDGE ( 'NONE', *, *, #53944, .F. ) ;
#28422 = FACE_OUTER_BOUND ( 'NONE', #4458, .T. ) ;
#28423 = CARTESIAN_POINT ( 'NONE',  ( -65.91414241012756747, -5.204170427930421283E-15, -3.032880804699297439 ) ) ;
#28424 = ORIENTED_EDGE ( 'NONE', *, *, #22664, .F. ) ;
#28425 = DIRECTION ( 'NONE',  ( -0.5449076811759708816, 0.6444004775717707689, 0.5364919789714475140 ) ) ;
#28426 = DIRECTION ( 'NONE',  ( -0.9999697198139514409, -0.000000000000000000, -0.007781995580013368816 ) ) ;
#28427 = VECTOR ( 'NONE', #5580, 999.9999999999998863 ) ;
#28428 = CARTESIAN_POINT ( 'NONE',  ( -18.80651470794193258, 0.000000000000000000, 6.890042898350599465 ) ) ;
#28429 = VECTOR ( 'NONE', #24735, 1000.000000000000000 ) ;
#28430 = DIRECTION ( 'NONE',  ( 0.007781995580012663651, 0.000000000000000000, -0.9999697198139515519 ) ) ;
#28431 = DIRECTION ( 'NONE',  ( 0.5364919789714477361, 0.6444004775717706579, 0.5449076811759711036 ) ) ;
#28432 = ORIENTED_EDGE ( 'NONE', *, *, #37169, .T. ) ;
#28433 = VERTEX_POINT ( 'NONE', #26763 ) ;
#28434 = PLANE ( 'NONE',  #49519 ) ;
#28435 = VECTOR ( 'NONE', #53532, 1000.000000000000227 ) ;
#28436 = VECTOR ( 'NONE', #38707, 999.9999999999998863 ) ;
#28437 = DIRECTION ( 'NONE',  ( 0.000000000000000000, -0.000000000000000000, -1.000000000000000000 ) ) ;
#28438 = EDGE_LOOP ( 'NONE', ( #22534, #5258, #38747, #52421 ) ) ;
#28439 = DIRECTION ( 'NONE',  ( -0.005002170337468016433, -0.7660444431189770143, 0.6427681459581293666 ) ) ;
#28440 = ADVANCED_FACE ( 'NONE', ( #5203 ), #27606, .F. ) ;
#28441 = VERTEX_POINT ( 'NONE', #35556 ) ;
#28442 = FACE_OUTER_BOUND ( 'NONE', #22754, .T. ) ;
#28443 = VECTOR ( 'NONE', #44091, 1000.000000000000114 ) ;
#28444 = ORIENTED_EDGE ( 'NONE', *, *, #47737, .F. ) ;
#28445 = AXIS2_PLACEMENT_3D ( 'NONE', #31230, #18755, #14223 ) ;
#28446 = ORIENTED_EDGE ( 'NONE', *, *, #1413, .F. ) ;
#28447 = DIRECTION ( 'NONE',  ( -0.5364919789714478471, 0.6444004775717705469, -0.5449076811759709926 ) ) ;
#28448 = LINE ( 'NONE', #28170, #40476 ) ;
#28449 = DIRECTION ( 'NONE',  ( 0.000000000000000000, -1.000000000000000000, 0.000000000000000000 ) ) ;
#28450 = ADVANCED_FACE ( 'NONE', ( #13976 ), #9744, .F. ) ;
#28451 = ORIENTED_EDGE ( 'NONE', *, *, #5860, .F. ) ;
#28452 = CARTESIAN_POINT ( 'NONE',  ( -29.86197018149027116, 0.000000000000000000, 8.281335066757780083 ) ) ;
#28453 = VERTEX_POINT ( 'NONE', #50839 ) ;
#28454 = EDGE_CURVE ( 'NONE', #42368, #16476, #55123, .T. ) ;
#28455 = EDGE_CURVE ( 'NONE', #5924, #20285, #20171, .T. ) ;
#28456 = ORIENTED_EDGE ( 'NONE', *, *, #5091, .F. ) ;
#28457 = EDGE_LOOP ( 'NONE', ( #55934, #37321, #20709, #25985 ) ) ;
#28458 = LINE ( 'NONE', #31889, #13225 ) ;
#28459 = VECTOR ( 'NONE', #52308, 1000.000000000000227 ) ;
#28460 = ORIENTED_EDGE ( 'NONE', *, *, #15883, .F. ) ;
#28461 = DIRECTION ( 'NONE',  ( -0.005002170337468016433, -0.7660444431189770143, 0.6427681459581293666 ) ) ;
#28462 = ADVANCED_FACE ( 'NONE', ( #11935 ), #42040, .F. ) ;
#28463 = VERTEX_POINT ( 'NONE', #50583 ) ;
#28464 = AXIS2_PLACEMENT_3D ( 'NONE', #34496, #21729, #39322 ) ;
#28465 = DIRECTION ( 'NONE',  ( 0.007781995580012662783, 0.000000000000000000, -0.9999697198139514409 ) ) ;
#28466 = DIRECTION ( 'NONE',  ( 0.007781995580012663651, 0.000000000000000000, -0.9999697198139515519 ) ) ;
#28467 = ORIENTED_EDGE ( 'NONE', *, *, #25998, .F. ) ;
#28468 = EDGE_CURVE ( 'NONE', #16069, #24033, #37813, .T. ) ;
#28469 = CARTESIAN_POINT ( 'NONE',  ( -12.70458494993575194, -0.1191753592594197858, 11.86531876794841978 ) ) ;
#28470 = VECTOR ( 'NONE', #20383, 999.9999999999998863 ) ;
#28471 = ORIENTED_EDGE ( 'NONE', *, *, #32024, .T. ) ;
#28472 = EDGE_CURVE ( 'NONE', #11761, #51416, #19646, .T. ) ;
#28473 = CARTESIAN_POINT ( 'NONE',  ( -2.730566055856384011, -5.007877867457373178, -2.157728989155597077 ) ) ;
#28474 = DIRECTION ( 'NONE',  ( -0.9999697198139514409, -0.000000000000000000, -0.007781995580013368816 ) ) ;
#28475 = DIRECTION ( 'NONE',  ( 0.007781995580012663651, -3.146120232559066537E-19, -0.9999697198139514409 ) ) ;
#28476 = DIRECTION ( 'NONE',  ( 0.005002170337468016433, -0.7660444431189770143, -0.6427681459581293666 ) ) ;
#28477 = PLANE ( 'NONE',  #25107 ) ;
#28478 = VECTOR ( 'NONE', #25589, 1000.000000000000227 ) ;
#28479 = PLANE ( 'NONE',  #53655 ) ;
#28480 = FACE_OUTER_BOUND ( 'NONE', #34551, .T. ) ;
#28481 = ORIENTED_EDGE ( 'NONE', *, *, #29047, .T. ) ;
#28482 = COLOUR_RGB ( '', 0.72549020, 0.75294118, 0.79215686) ;
#28483 = EDGE_CURVE ( 'NONE', #44124, #36489, #33531, .T. ) ;
#28484 = ORIENTED_EDGE ( 'NONE', *, *, #5408, .F. ) ;
#28485 = LINE ( 'NONE', #6631, #15546 ) ;
#28486 = DIRECTION ( 'NONE',  ( -0.5449076811759708816, 0.6444004775717707689, 0.5364919789714475140 ) ) ;
#28487 = LINE ( 'NONE', #11162, #28527 ) ;
#28488 = DIRECTION ( 'NONE',  ( 0.007781995580012662783, 0.000000000000000000, -0.9999697198139514409 ) ) ;
#28489 = EDGE_CURVE ( 'NONE', #15384, #51591, #29263, .T. ) ;
#28490 = VECTOR ( 'NONE', #15510, 999.9999999999998863 ) ;
#28491 = VECTOR ( 'NONE', #26853, 1000.000000000000114 ) ;
#28492 = CARTESIAN_POINT ( 'NONE',  ( -15.88130887279446490, 0.000000000000000000, 3.050160814894388839 ) ) ;
#28493 = EDGE_LOOP ( 'NONE', ( #54944, #34132, #16230, #30742 ) ) ;
#28494 = DIRECTION ( 'NONE',  ( 0.007781995580012663651, -3.146120232559066537E-19, -0.9999697198139514409 ) ) ;
#28495 = CARTESIAN_POINT ( 'NONE',  ( -10.00813838035478298, 0.000000000000000000, 10.77830692922518452 ) ) ;
#28496 = ORIENTED_EDGE ( 'NONE', *, *, #22324, .T. ) ;
#28497 = LINE ( 'NONE', #45815, #21146 ) ;
#28498 = DIRECTION ( 'NONE',  ( 0.007781995580012663651, -3.146120232559066537E-19, -0.9999697198139514409 ) ) ;
#28499 = ORIENTED_EDGE ( 'NONE', *, *, #54259, .F. ) ;
#28500 = PLANE ( 'NONE',  #17104 ) ;
#28501 = DIRECTION ( 'NONE',  ( -0.000000000000000000, -1.000000000000000000, -0.000000000000000000 ) ) ;
#28502 = CARTESIAN_POINT ( 'NONE',  ( -17.37561052637969183, 1.095915999411505526, 3.396243480022655081 ) ) ;
#28503 = CARTESIAN_POINT ( 'NONE',  ( -26.13415699229845757, -0.1191753592594197858, 6.933020519852192365 ) ) ;
#28504 = PLANE ( 'NONE',  #12917 ) ;
#28505 = AXIS2_PLACEMENT_3D ( 'NONE', #37082, #32801, #20301 ) ;
#28506 = ORIENTED_EDGE ( 'NONE', *, *, #28483, .T. ) ;
#28507 = ORIENTED_EDGE ( 'NONE', *, *, #27877, .T. ) ;
#28508 = AXIS2_PLACEMENT_3D ( 'NONE', #37200, #54504, #15603 ) ;
#28509 = DIRECTION ( 'NONE',  ( 0.6427681459581294776, -0.7660444431189769032, 0.005002170337467562802 ) ) ;
#28510 = PLANE ( 'NONE',  #45808 ) ;
#28511 = CARTESIAN_POINT ( 'NONE',  ( -9.496532450088523092, 0.000000000000000000, 4.746502914164204334 ) ) ;
#28512 = VECTOR ( 'NONE', #55369, 1000.000000000000227 ) ;
#28513 = DIRECTION ( 'NONE',  ( 0.007781995580012663651, 0.000000000000000000, -0.9999697198139515519 ) ) ;
#28514 = DIRECTION ( 'NONE',  ( 1.000000000000000000, 0.000000000000000000, 0.000000000000000000 ) ) ;
#28515 = CARTESIAN_POINT ( 'NONE',  ( -17.83139810946674686, -0.1191753592594197858, 13.85674710641801788 ) ) ;
#28516 = ADVANCED_FACE ( 'NONE', ( #7697 ), #46292, .F. ) ;
#28517 = ORIENTED_EDGE ( 'NONE', *, *, #17573, .F. ) ;
#28518 = FACE_OUTER_BOUND ( 'NONE', #52094, .T. ) ;
#28519 = LINE ( 'NONE', #45845, #24139 ) ;
#28520 = DIRECTION ( 'NONE',  ( 0.007781995580012663651, 0.000000000000000000, -0.9999697198139515519 ) ) ;
#28522 = ORIENTED_EDGE ( 'NONE', *, *, #44246, .F. ) ;
#28521 = VECTOR ( 'NONE', #21464, 999.9999999999998863 ) ;
#28523 = VECTOR ( 'NONE', #19234, 999.9999999999998863 ) ;
#28524 = FACE_OUTER_BOUND ( 'NONE', #21924, .T. ) ;
#28525 = CARTESIAN_POINT ( 'NONE',  ( -15.13495153988577968, 0.000000000000000000, 12.76973526769478084 ) ) ;
#28526 = DIRECTION ( 'NONE',  ( 0.5449076811759707706, 0.6444004775717708799, -0.5364919789714476250 ) ) ;
#28527 = VECTOR ( 'NONE', #50637, 1000.000000000000227 ) ;
#28528 = ORIENTED_EDGE ( 'NONE', *, *, #3925, .T. ) ;
#28529 = PLANE ( 'NONE',  #53102 ) ;
#28530 = ORIENTED_EDGE ( 'NONE', *, *, #11804, .T. ) ;
#28531 = ADVANCED_FACE ( 'NONE', ( #54275 ), #55379, .F. ) ;
#28532 = VECTOR ( 'NONE', #50081, 1000.000000000000227 ) ;
#28533 = ORIENTED_EDGE ( 'NONE', *, *, #21854, .T. ) ;
#28534 = ORIENTED_EDGE ( 'NONE', *, *, #20247, .F. ) ;
#28535 = AXIS2_PLACEMENT_3D ( 'NONE', #17984, #52880, #39836 ) ;
#28536 = ORIENTED_EDGE ( 'NONE', *, *, #39003, .F. ) ;
#28537 = ORIENTED_EDGE ( 'NONE', *, *, #18661, .F. ) ;
#28538 = CARTESIAN_POINT ( 'NONE',  ( -23.33849165029409889, 0.000000000000000000, 5.946783852668351855 ) ) ;
#28539 = ORIENTED_EDGE ( 'NONE', *, *, #15191, .F. ) ;
#28540 = ORIENTED_EDGE ( 'NONE', *, *, #43243, .F. ) ;
#28541 = CARTESIAN_POINT ( 'NONE',  ( -14.96433427924230841, -0.1191753592594198830, 3.695958034714191154 ) ) ;
#28542 = EDGE_CURVE ( 'NONE', #23008, #38521, #7398, .T. ) ;
#28543 = ORIENTED_EDGE ( 'NONE', *, *, #44378, .F. ) ;
#28544 = ORIENTED_EDGE ( 'NONE', *, *, #22469, .F. ) ;
#28545 = EDGE_CURVE ( 'NONE', #39497, #349, #28150, .T. ) ;
#28546 = EDGE_LOOP ( 'NONE', ( #45601, #27625, #29896, #3974 ) ) ;
#28547 = AXIS2_PLACEMENT_3D ( 'NONE', #48560, #16861, #31536 ) ;
#28548 = LINE ( 'NONE', #45877, #42899 ) ;
#28549 = VECTOR ( 'NONE', #14651, 999.9999999999998863 ) ;
#28550 = FACE_OUTER_BOUND ( 'NONE', #49643, .T. ) ;
#28551 = CARTESIAN_POINT ( 'NONE',  ( -18.67619601524082285, 0.000000000000000000, 3.936400510096834893 ) ) ;
#28552 = DIRECTION ( 'NONE',  ( -0.005002170337468016433, -0.7660444431189770143, 0.6427681459581293666 ) ) ;
#28553 = CARTESIAN_POINT ( 'NONE',  ( -11.77243710274829525, -0.1191753592594197858, 11.50324088822667612 ) ) ;
#28554 = VECTOR ( 'NONE', #40161, 1000.000000000000227 ) ;
#28555 = EDGE_LOOP ( 'NONE', ( #22621, #17078, #47132, #5754 ) ) ;
#28556 = ADVANCED_FACE ( 'NONE', ( #33276 ), #45459, .F. ) ;
#28557 = ORIENTED_EDGE ( 'NONE', *, *, #32555, .T. ) ;
#28558 = CARTESIAN_POINT ( 'NONE',  ( -12.70458494993575194, -0.1191753592594197858, 11.86531876794841978 ) ) ;
#28559 = LINE ( 'NONE', #20616, #52064 ) ;
#28560 = VECTOR ( 'NONE', #10569, 1000.000000000000000 ) ;
#28561 = CARTESIAN_POINT ( 'NONE',  ( -27.56453817542467633, 16.74388231021177020, -4.674278956779107652 ) ) ;
#28562 = ADVANCED_FACE ( 'NONE', ( #32972 ), #41216, .F. ) ;
#28563 = VECTOR ( 'NONE', #28465, 1000.000000000000227 ) ;
#28564 = AXIS2_PLACEMENT_3D ( 'NONE', #35021, #17122, #51744 ) ;
#28565 = FACE_OUTER_BOUND ( 'NONE', #27374, .T. ) ;
#28566 = VECTOR ( 'NONE', #3995, 1000.000000000000114 ) ;
#28567 = CARTESIAN_POINT ( 'NONE',  ( 3.004435629306332345, -1.000000000000000000, -3.312607213261892003 ) ) ;
#28568 = AXIS2_PLACEMENT_3D ( 'NONE', #21509, #12970, #47616 ) ;
#28569 = CARTESIAN_POINT ( 'NONE',  ( -12.18513505871164604, -0.1191753592594185784, 4.825582615095539651 ) ) ;
#28570 = ORIENTED_EDGE ( 'NONE', *, *, #35584, .F. ) ;
#28571 = LINE ( 'NONE', #7011, #11127 ) ;
#28572 = ORIENTED_EDGE ( 'NONE', *, *, #15048, .T. ) ;
#28573 = VECTOR ( 'NONE', #30398, 1000.000000000000000 ) ;
#28574 = LINE ( 'NONE', #6185, #10220 ) ;
#28575 = CARTESIAN_POINT ( 'NONE',  ( -12.60458797795435615, 0.000000000000000000, 11.86609696750642229 ) ) ;
#28576 = DIRECTION ( 'NONE',  ( -0.8531650599175527594, 0.4028455766673922356, 0.3313982828793700652 ) ) ;
#28577 = LINE ( 'NONE', #45902, #54029 ) ;
#28578 = LINE ( 'NONE', #2996, #1463 ) ;
#28579 = VECTOR ( 'NONE', #30709, 999.9999999999998863 ) ;
#28580 = AXIS2_PLACEMENT_3D ( 'NONE', #16327, #12071, #46727 ) ;
#28581 = ORIENTED_EDGE ( 'NONE', *, *, #16630, .F. ) ;
#28582 = LINE ( 'NONE', #23496, #13058 ) ;
#28583 = FACE_OUTER_BOUND ( 'NONE', #50924, .T. ) ;
#28584 = CARTESIAN_POINT ( 'NONE',  ( -27.99923088623136636, 0.000000000000000000, 7.757173251277078130 ) ) ;
#28585 = EDGE_CURVE ( 'NONE', #40214, #20884, #32685, .T. ) ;
#28586 = DIRECTION ( 'NONE',  ( 0.5364919789714477361, 0.6444004775717706579, 0.5449076811759711036 ) ) ;
#28587 = CARTESIAN_POINT ( 'NONE',  ( -10.00813838035478298, 0.000000000000000000, 10.77830692922518452 ) ) ;
#28588 = EDGE_CURVE ( 'NONE', #13341, #6886, #28995, .T. ) ;
#28589 = DIRECTION ( 'NONE',  ( -0.9999697198139514409, -0.000000000000000000, -0.007781995580013368816 ) ) ;
#28590 = LINE ( 'NONE', #38505, #52837 ) ;
#28591 = VECTOR ( 'NONE', #7276, 999.9999999999998863 ) ;
#28592 = CARTESIAN_POINT ( 'NONE',  ( -28.93137873341882127, 0.000000000000000000, 8.119251130998824451 ) ) ;
#28593 = AXIS2_PLACEMENT_3D ( 'NONE', #3708, #25310, #17077 ) ;
#28594 = EDGE_CURVE ( 'NONE', #20073, #52488, #46038, .T. ) ;
#28595 = DIRECTION ( 'NONE',  ( -0.3620778797217456546, 0.000000000000000000, -0.9321478471874540261 ) ) ;
#28596 = ORIENTED_EDGE ( 'NONE', *, *, #53760, .F. ) ;
#28597 = VECTOR ( 'NONE', #1033, 999.9999999999998863 ) ;
#28598 = ADVANCED_FACE ( 'NONE', ( #2841 ), #39182, .F. ) ;
#28599 = EDGE_CURVE ( 'NONE', #41034, #15196, #39487, .T. ) ;
#28600 = EDGE_CURVE ( 'NONE', #12202, #46860, #12791, .T. ) ;
#28601 = ORIENTED_EDGE ( 'NONE', *, *, #11451, .F. ) ;
#28602 = VECTOR ( 'NONE', #21078, 1000.000000000000227 ) ;
#28603 = ORIENTED_EDGE ( 'NONE', *, *, #10419, .T. ) ;
#28604 = EDGE_LOOP ( 'NONE', ( #36800, #43090, #7349, #45046 ) ) ;
#28605 = AXIS2_PLACEMENT_3D ( 'NONE', #320, #12834, #47184 ) ;
#28606 = VECTOR ( 'NONE', #3608, 999.9999999999998863 ) ;
#28607 = ORIENTED_EDGE ( 'NONE', *, *, #41769, .T. ) ;
#28608 = ORIENTED_EDGE ( 'NONE', *, *, #35224, .T. ) ;
#28609 = CARTESIAN_POINT ( 'NONE',  ( -16.87359065091598254, 2.714935509636508204, 3.149586712851912829 ) ) ;
#28610 = CARTESIAN_POINT ( 'NONE',  ( -14.41616653189352348, 0.000000000000000000, 5.816213393605395687 ) ) ;
#28611 = CARTESIAN_POINT ( 'NONE',  ( -17.74482636761137044, -0.1191753592594197858, 3.674319602356483916 ) ) ;
#28612 = VECTOR ( 'NONE', #45141, 1000.000000000000000 ) ;
#28613 = VECTOR ( 'NONE', #8733, 999.9999999999998863 ) ;
#28614 = ORIENTED_EDGE ( 'NONE', *, *, #17855, .F. ) ;
#28615 = DIRECTION ( 'NONE',  ( -0.5449076811759708816, 0.6444004775717707689, 0.5364919789714475140 ) ) ;
#28616 = EDGE_CURVE ( 'NONE', #46025, #37342, #34641, .T. ) ;
#28617 = ORIENTED_EDGE ( 'NONE', *, *, #27194, .F. ) ;
#28618 = ORIENTED_EDGE ( 'NONE', *, *, #8160, .F. ) ;
#28619 = VECTOR ( 'NONE', #15734, 1000.000000000000227 ) ;
#28620 = ADVANCED_FACE ( 'NONE', ( #22154 ), #21611, .F. ) ;
#28621 = AXIS2_PLACEMENT_3D ( 'NONE', #2641, #12000, #38129 ) ;
#28622 = CARTESIAN_POINT ( 'NONE',  ( -66.67378107351682104, -8.735535983216148992, 1.704803601108932920 ) ) ;
#28623 = ADVANCED_FACE ( 'NONE', ( #26146 ), #43200, .F. ) ;
#28624 = LINE ( 'NONE', #33171, #24598 ) ;
#28625 = CARTESIAN_POINT ( 'NONE',  ( -17.23272844799286929, 0.000000000000000000, 9.487614955574981579 ) ) ;
#28626 = ORIENTED_EDGE ( 'NONE', *, *, #54748, .F. ) ;
#28627 = CARTESIAN_POINT ( 'NONE',  ( -69.43545830293986398, -9.790829293527439248, 7.501778215771295777 ) ) ;
#28628 = EDGE_LOOP ( 'NONE', ( #52831, #8370, #7801, #46656 ) ) ;
#28629 = ADVANCED_FACE ( 'NONE', ( #17912 ), #43454, .F. ) ;
#28630 = DIRECTION ( 'NONE',  ( 0.007781995580012662783, 0.000000000000000000, -0.9999697198139514409 ) ) ;
#28631 = DIRECTION ( 'NONE',  ( 0.5364919789714477361, 0.6444004775717706579, 0.5449076811759711036 ) ) ;
#28632 = ADVANCED_FACE ( 'NONE', ( #4298 ), #17066, .F. ) ;
#28633 = VECTOR ( 'NONE', #916, 1000.000000000000227 ) ;
#28634 = LINE ( 'NONE', #11010, #6463 ) ;
#28635 = CARTESIAN_POINT ( 'NONE',  ( -14.94916102560700821, 0.000000000000000000, 2.688082935172642962 ) ) ;
#28636 = CARTESIAN_POINT ( 'NONE',  ( -11.64304826722767672, 25.38767603887909985, 3.000000000000000000 ) ) ;
#28637 = LINE ( 'NONE', #45129, #42889 ) ;
#28639 = VECTOR ( 'NONE', #8257, 1000.000000000000227 ) ;
#28638 = LINE ( 'NONE', #28337, #49365 ) ;
#28640 = LINE ( 'NONE', #38557, #18502 ) ;
#28641 = CARTESIAN_POINT ( 'NONE',  ( -14.93495759592298988, 0.000000000000000000, 12.77129166681078409 ) ) ;
#28642 = ORIENTED_EDGE ( 'NONE', *, *, #28126, .T. ) ;
#28643 = DIRECTION ( 'NONE',  ( 0.007781995580012663651, -3.146120232559066537E-19, -0.9999697198139514409 ) ) ;
#28644 = ORIENTED_EDGE ( 'NONE', *, *, #39697, .T. ) ;
#28645 = VECTOR ( 'NONE', #26014, 1000.000000000000114 ) ;
#28646 = PLANE ( 'NONE',  #41061 ) ;
#28647 = LINE ( 'NONE', #49917, #31378 ) ;
#28648 = PLANE ( 'NONE',  #17802 ) ;
#28649 = AXIS2_PLACEMENT_3D ( 'NONE', #36073, #576, #13368 ) ;
#28650 = LINE ( 'NONE', #7080, #2370 ) ;
#28651 = DIRECTION ( 'NONE',  ( 0.7660212471507180654, -0.6427876096865404731, 0.005961354470445141482 ) ) ;
#28652 = AXIS2_PLACEMENT_3D ( 'NONE', #36320, #45136, #6497 ) ;
#28654 = AXIS2_PLACEMENT_3D ( 'NONE', #25995, #21451, #20861 ) ;
#28653 = DIRECTION ( 'NONE',  ( 0.007781995580012663651, 0.000000000000000000, -0.9999697198139515519 ) ) ;
#28655 = ORIENTED_EDGE ( 'NONE', *, *, #30891, .T. ) ;
#28656 = DIRECTION ( 'NONE',  ( 0.9999697198139515519, 0.000000000000000000, 0.007781995580013368816 ) ) ;
#28657 = LINE ( 'NONE', #15859, #33895 ) ;
#28658 = LINE ( 'NONE', #27533, #35819 ) ;
#28659 = VECTOR ( 'NONE', #2451, 1000.000000000000227 ) ;
#28660 = LINE ( 'NONE', #45978, #33648 ) ;
#28662 = VECTOR ( 'NONE', #16337, 999.9999999999998863 ) ;
#28661 = CARTESIAN_POINT ( 'NONE',  ( -20.54204810873173415, 0.000000000000000000, 4.860550213503115558 ) ) ;
#28663 = VECTOR ( 'NONE', #11840, 999.9999999999998863 ) ;
#28664 = DIRECTION ( 'NONE',  ( 0.007781995580012663651, 0.000000000000000000, -0.9999697198139515519 ) ) ;
#28665 = PLANE ( 'NONE',  #1247 ) ;
#28666 = DIRECTION ( 'NONE',  ( 0.9999697198139515519, 0.000000000000000000, 0.007781995580013368816 ) ) ;
#28667 = DIRECTION ( 'NONE',  ( -0.7660212471507179544, -0.6427876096865405842, -0.005961354470445141482 ) ) ;
#28668 = ORIENTED_EDGE ( 'NONE', *, *, #1443, .F. ) ;
#28669 = VECTOR ( 'NONE', #6823, 999.9999999999998863 ) ;
#28671 = DIRECTION ( 'NONE',  ( -0.9932609354084158682, -0.1139014070068027212, -0.02142857142857160571 ) ) ;
#28670 = VECTOR ( 'NONE', #21800, 999.9999999999998863 ) ;
#28672 = EDGE_LOOP ( 'NONE', ( #28990, #27091, #51471, #25880 ) ) ;
#28673 = FACE_OUTER_BOUND ( 'NONE', #45304, .T. ) ;
#28674 = DIRECTION ( 'NONE',  ( 0.5449076811759707706, 0.6444004775717708799, -0.5364919789714476250 ) ) ;
#28675 = ADVANCED_FACE ( 'NONE', ( #46887 ), #21015, .F. ) ;
#28676 = ADVANCED_FACE ( 'NONE', ( #30694 ), #38649, .F. ) ;
#28677 = ORIENTED_EDGE ( 'NONE', *, *, #1630, .T. ) ;
#28678 = EDGE_LOOP ( 'NONE', ( #24482, #23366, #22802, #45313 ) ) ;
#28679 = PLANE ( 'NONE',  #22937 ) ;
#28680 = EDGE_CURVE ( 'NONE', #682, #24541, #16685, .T. ) ;
#28681 = VECTOR ( 'NONE', #29433, 999.9999999999998863 ) ;
#28682 = VERTEX_POINT ( 'NONE', #51962 ) ;
#28683 = EDGE_LOOP ( 'NONE', ( #21824, #11767, #45182, #32692 ) ) ;
#28684 = ORIENTED_EDGE ( 'NONE', *, *, #46592, .T. ) ;
#28685 = CARTESIAN_POINT ( 'NONE',  ( -17.21991457958245775, 0.000000000000000000, 7.841060383248950494 ) ) ;
#28686 = LINE ( 'NONE', #37463, #54125 ) ;
#28687 = VECTOR ( 'NONE', #47731, 999.9999999999998863 ) ;
#28688 = LINE ( 'NONE', #6824, #11290 ) ;
#28689 = AXIS2_PLACEMENT_3D ( 'NONE', #28946, #7345, #24659 ) ;
#28690 = ORIENTED_EDGE ( 'NONE', *, *, #38855, .F. ) ;
#28691 = VERTEX_POINT ( 'NONE', #17613 ) ;
#28692 = EDGE_CURVE ( 'NONE', #45599, #53284, #42884, .T. ) ;
#28693 = VECTOR ( 'NONE', #34571, 1000.000000000000000 ) ;
#28694 = DIRECTION ( 'NONE',  ( 0.005961354470445682716, -0.6427876096865404731, -0.7660212471507180654 ) ) ;
#28695 = PLANE ( 'NONE',  #37238 ) ;
#28696 = ORIENTED_EDGE ( 'NONE', *, *, #25928, .F. ) ;
#28697 = FACE_OUTER_BOUND ( 'NONE', #8430, .T. ) ;
#28698 = ORIENTED_EDGE ( 'NONE', *, *, #54787, .T. ) ;
#28699 = CARTESIAN_POINT ( 'NONE',  ( -14.01545677930355183, 0.000000000000000000, 2.126011111488108174 ) ) ;
#28700 = CARTESIAN_POINT ( 'NONE',  ( -15.78478530592635920, -3.270328918600659218, 8.180445300800458952 ) ) ;
#28701 = VECTOR ( 'NONE', #36252, 999.9999999999998863 ) ;
#28702 = EDGE_LOOP ( 'NONE', ( #18405, #52901, #46051, #52339 ) ) ;
#28703 = ADVANCED_FACE ( 'NONE', ( #29576 ), #3991, .F. ) ;
#28704 = VECTOR ( 'NONE', #17439, 999.9999999999998863 ) ;
#28705 = DIRECTION ( 'NONE',  ( 0.005002170337468016433, -0.7660444431189770143, -0.6427681459581293666 ) ) ;
#28706 = EDGE_CURVE ( 'NONE', #18997, #32684, #26399, .T. ) ;
#28707 = AXIS2_PLACEMENT_3D ( 'NONE', #21573, #26645, #30654 ) ;
#28708 = FACE_OUTER_BOUND ( 'NONE', #28555, .T. ) ;
#28709 = VECTOR ( 'NONE', #55455, 1000.000000000000000 ) ;
#28711 = EDGE_CURVE ( 'NONE', #21327, #37913, #34111, .T. ) ;
#28710 = ORIENTED_EDGE ( 'NONE', *, *, #2937, .T. ) ;
#28712 = CARTESIAN_POINT ( 'NONE',  ( -23.33693525117809386, 0.000000000000000000, 5.746789908705562944 ) ) ;
#28713 = CARTESIAN_POINT ( 'NONE',  ( 2.072287782118878319, 0.000000000000000000, -2.950529333540147015 ) ) ;
#28714 = CARTESIAN_POINT ( 'NONE',  ( -16.06709938707323460, 0.000000000000000000, 13.13181314741652628 ) ) ;
#28715 = ADVANCED_FACE ( 'NONE', ( #47733 ), #26990, .F. ) ;
#28716 = ORIENTED_EDGE ( 'NONE', *, *, #46368, .T. ) ;
#28717 = DIRECTION ( 'NONE',  ( 0.007781995580012662783, 0.000000000000000000, -0.9999697198139514409 ) ) ;
#28718 = CARTESIAN_POINT ( 'NONE',  ( -19.62794756868486346, -0.1191753592594171213, 5.875657136580680451 ) ) ;
#28719 = ADVANCED_FACE ( 'NONE', ( #32079 ), #44852, .F. ) ;
#28720 = LINE ( 'NONE', #2298, #53926 ) ;
#28721 = CARTESIAN_POINT ( 'NONE',  ( -29.86274838104827367, -0.1191753592594197858, 8.381332038739175871 ) ) ;
#28722 = DIRECTION ( 'NONE',  ( 0.007781995580012663651, -3.146120232559066537E-19, -0.9999697198139514409 ) ) ;
#28723 = PLANE ( 'NONE',  #25221 ) ;
#28724 = VECTOR ( 'NONE', #27888, 1000.000000000000227 ) ;
#28725 = DIRECTION ( 'NONE',  ( 0.000000000000000000, 1.000000000000000000, 0.000000000000000000 ) ) ;
#28726 = ORIENTED_EDGE ( 'NONE', *, *, #24328, .F. ) ;
#28727 = CARTESIAN_POINT ( 'NONE',  ( -13.00944197295985916, 0.000000000000000000, 4.180506556583391209 ) ) ;
#28728 = CARTESIAN_POINT ( 'NONE',  ( -67.26768186997090027, -3.935216494285589413E-12, -4.549856479222408545 ) ) ;
#28729 = VERTEX_POINT ( 'NONE', #10207 ) ;
#28730 = CARTESIAN_POINT ( 'NONE',  ( -13.08330893211609869, 0.000000000000000000, 1.763933231766363630 ) ) ;
#28731 = CARTESIAN_POINT ( 'NONE',  ( -58.00000000000000711, -9.333333333333333925, -3.692809041582062246 ) ) ;
#28732 = VECTOR ( 'NONE', #33142, 999.9999999999998863 ) ;
#28733 = CARTESIAN_POINT ( 'NONE',  ( -18.69005161448685115, -0.1191753592594169547, 4.774959850343403645 ) ) ;
#28734 = CARTESIAN_POINT ( 'NONE',  ( -17.89488364610653903, -0.8417996532631562001, 3.805443821891801193 ) ) ;
#28735 = PLANE ( 'NONE',  #35665 ) ;
#28736 = ORIENTED_EDGE ( 'NONE', *, *, #47286, .T. ) ;
#28737 = VECTOR ( 'NONE', #30186, 1000.000000000000227 ) ;
#28738 = ORIENTED_EDGE ( 'NONE', *, *, #49513, .T. ) ;
#28739 = DIRECTION ( 'NONE',  ( -0.000000000000000000, -1.000000000000000000, -0.000000000000000000 ) ) ;
#28740 = LINE ( 'NONE', #46596, #44734 ) ;
#28741 = EDGE_CURVE ( 'NONE', #52604, #17849, #48559, .T. ) ;
#28742 = CARTESIAN_POINT ( 'NONE',  ( -9.031895553247439423, 0.000000000000000000, 4.750118825932213795 ) ) ;
#28743 = AXIS2_PLACEMENT_3D ( 'NONE', #39103, #46795, #12139 ) ;
#28744 = ORIENTED_EDGE ( 'NONE', *, *, #20282, .F. ) ;
#28745 = DIRECTION ( 'NONE',  ( -0.7660212471507179544, -0.6427876096865405842, -0.005961354470445141482 ) ) ;
#28746 = ORIENTED_EDGE ( 'NONE', *, *, #1471, .T. ) ;
#28747 = CARTESIAN_POINT ( 'NONE',  ( -25.20200914511100265, -0.1191753592594197858, 6.570942640130446932 ) ) ;
#28748 = ADVANCED_FACE ( 'NONE', ( #23553 ), #53383, .F. ) ;
#28749 = EDGE_CURVE ( 'NONE', #50088, #27679, #5668, .T. ) ;
#28750 = VECTOR ( 'NONE', #6873, 1000.000000000000227 ) ;
#28751 = VERTEX_POINT ( 'NONE', #9675 ) ;
#28752 = ORIENTED_EDGE ( 'NONE', *, *, #40228, .T. ) ;
#28753 = FACE_OUTER_BOUND ( 'NONE', #36989, .T. ) ;
#28754 = CARTESIAN_POINT ( 'NONE',  ( -15.88130887279446490, 0.000000000000000000, 3.050160814894388839 ) ) ;
#28755 = CARTESIAN_POINT ( 'NONE',  ( -18.83646877814363663, -0.8417996532631553119, 5.380192537759650229 ) ) ;
#28756 = ORIENTED_EDGE ( 'NONE', *, *, #38532, .T. ) ;
#28757 = DIRECTION ( 'NONE',  ( 0.005002170337468016433, -0.7660444431189770143, -0.6427681459581293666 ) ) ;
#28758 = ORIENTED_EDGE ( 'NONE', *, *, #29681, .F. ) ;
#28759 = EDGE_CURVE ( 'NONE', #46034, #31630, #44301, .T. ) ;
#28760 = VERTEX_POINT ( 'NONE', #1110 ) ;
#28761 = ORIENTED_EDGE ( 'NONE', *, *, #2052, .T. ) ;
#28762 = DIRECTION ( 'NONE',  ( 0.5449076811759707706, 0.6444004775717708799, -0.5364919789714476250 ) ) ;
#28763 = DIRECTION ( 'NONE',  ( -0.9321478471874540261, 0.000000000000000000, 0.3620778797217457656 ) ) ;
#28764 = EDGE_LOOP ( 'NONE', ( #4176, #28756, #26026, #25393 ) ) ;
#28765 = FACE_OUTER_BOUND ( 'NONE', #22358, .T. ) ;
#28766 = ORIENTED_EDGE ( 'NONE', *, *, #18218, .T. ) ;
#28767 = DIRECTION ( 'NONE',  ( 0.6427681459581294776, -0.7660444431189769032, 0.005002170337467562802 ) ) ;
#28768 = FACE_OUTER_BOUND ( 'NONE', #46843, .T. ) ;
#28769 = ORIENTED_EDGE ( 'NONE', *, *, #39714, .T. ) ;
#28770 = VECTOR ( 'NONE', #31878, 999.9999999999998863 ) ;
#28771 = DIRECTION ( 'NONE',  ( 0.2426528472758542054, 0.7422098413412800966, 0.6246952433987894571 ) ) ;
#28772 = ORIENTED_EDGE ( 'NONE', *, *, #13636, .T. ) ;
#28773 = EDGE_CURVE ( 'NONE', #17943, #2828, #45146, .T. ) ;
#28774 = VECTOR ( 'NONE', #8979, 999.9999999999998863 ) ;
#28775 = LINE ( 'NONE', #24773, #30089 ) ;
#28776 = LINE ( 'NONE', #41268, #46537 ) ;
#28777 = DIRECTION ( 'NONE',  ( -0.005002170337468016433, -0.7660444431189770143, 0.6427681459581293666 ) ) ;
#28778 = DIRECTION ( 'NONE',  ( -0.5449076811759708816, 0.6444004775717707689, 0.5364919789714475140 ) ) ;
#28779 = CARTESIAN_POINT ( 'NONE',  ( -15.87975247367846166, 0.000000000000000000, 2.850166870931599927 ) ) ;
#28780 = DIRECTION ( 'NONE',  ( 0.005961354470445682716, -0.6427876096865404731, -0.7660212471507180654 ) ) ;
#28781 = ORIENTED_EDGE ( 'NONE', *, *, #44059, .F. ) ;
#28782 = B_SPLINE_CURVE_WITH_KNOTS ( 'NONE', 3,
 ( #968, #18292, #40738, #27377 ),
 .UNSPECIFIED., .F., .F.,
 ( 4, 4 ),
 ( 0.000000000000000000, 0.0003538173816227488952 ),
 .UNSPECIFIED. ) ;
#28783 = EDGE_LOOP ( 'NONE', ( #16473, #51532, #41354, #35073 ) ) ;
#28784 = VECTOR ( 'NONE', #54142, 1000.000000000000114 ) ;
#28785 = DIRECTION ( 'NONE',  ( 0.000000000000000000, -1.000000000000000000, 0.000000000000000000 ) ) ;
#28786 = EDGE_CURVE ( 'NONE', #27546, #38691, #18446, .T. ) ;
#28787 = CARTESIAN_POINT ( 'NONE',  ( -24.27063949748155380, 0.000000000000000000, 6.308861732390097288 ) ) ;
#28788 = LINE ( 'NONE', #1318, #44946 ) ;
#28789 = CARTESIAN_POINT ( 'NONE',  ( -18.36514955148751582, 0.6102101463440047224, 3.796110601923448069 ) ) ;
#28790 = DIRECTION ( 'NONE',  ( -0.7660212471507179544, -0.6427876096865405842, -0.005961354470445141482 ) ) ;
#28791 = DIRECTION ( 'NONE',  ( 0.000000000000000000, -1.000000000000000000, 0.000000000000000000 ) ) ;
#28792 = ORIENTED_EDGE ( 'NONE', *, *, #17936, .T. ) ;
#28793 = CARTESIAN_POINT ( 'NONE',  ( -13.73672976910459909, 0.000000000000000000, 12.22661844811216270 ) ) ;
#28794 = DIRECTION ( 'NONE',  ( -0.5364919789714478471, 0.6444004775717705469, -0.5449076811759709926 ) ) ;
#28795 = ORIENTED_EDGE ( 'NONE', *, *, #4093, .T. ) ;
#28796 = DIRECTION ( 'NONE',  ( 0.9999697198139515519, 0.000000000000000000, 0.007781995580013368816 ) ) ;
#28797 = LINE ( 'NONE', #3506, #54013 ) ;
#28798 = VERTEX_POINT ( 'NONE', #44011 ) ;
#28799 = EDGE_CURVE ( 'NONE', #15255, #31, #49394, .T. ) ;
#28800 = CARTESIAN_POINT ( 'NONE',  ( -67.27906308014451042, 1.999999999999999556, 2.024546322512588148 ) ) ;
#28801 = LINE ( 'NONE', #41826, #38719 ) ;
#28802 = DIRECTION ( 'NONE',  ( -0.5364919789714478471, 0.6444004775717705469, -0.5449076811759709926 ) ) ;
#28803 = EDGE_CURVE ( 'NONE', #22744, #24469, #1687, .T. ) ;
#28804 = EDGE_CURVE ( 'NONE', #49949, #39181, #48846, .T. ) ;
#28805 = LINE ( 'NONE', #28503, #17819 ) ;
#28806 = LINE ( 'NONE', #32760, #44640 ) ;
#28807 = VERTEX_POINT ( 'NONE', #49102 ) ;
#28808 = VERTEX_POINT ( 'NONE', #27245 ) ;
#28809 = CARTESIAN_POINT ( 'NONE',  ( -16.81345671998191449, 0.000000000000000000, 3.412238694616132495 ) ) ;
#28810 = CARTESIAN_POINT ( 'NONE',  ( -31.72782227498118601, 0.000000000000000000, 9.205484770164058972 ) ) ;
#28811 = DIRECTION ( 'NONE',  ( 0.9999697198139515519, 0.000000000000000000, 0.007781995580013368816 ) ) ;
#28812 = EDGE_CURVE ( 'NONE', #46187, #42035, #53640, .T. ) ;
#28813 = CARTESIAN_POINT ( 'NONE',  ( -30.79567442779373110, 0.000000000000000000, 8.843406890442315316 ) ) ;
#28814 = CARTESIAN_POINT ( 'NONE',  ( -16.71591784297447703, 1.419719901456506728, 3.129665398755458572 ) ) ;
#28815 = EDGE_CURVE ( 'NONE', #41698, #18658, #5971, .T. ) ;
#28816 = FACE_OUTER_BOUND ( 'NONE', #22545, .T. ) ;
#28817 = ORIENTED_EDGE ( 'NONE', *, *, #50789, .T. ) ;
#28818 = PLANE ( 'NONE',  #18386 ) ;
#28819 = ADVANCED_FACE ( 'NONE', ( #44557 ), #22995, .F. ) ;
#28821 = VECTOR ( 'NONE', #52741, 999.9999999999998863 ) ;
#28820 = LINE ( 'NONE', #7225, #29582 ) ;
#28822 = FACE_OUTER_BOUND ( 'NONE', #40633, .T. ) ;
#28823 = EDGE_LOOP ( 'NONE', ( #32458, #1965, #52851, #40119 ) ) ;
#28824 = LINE ( 'NONE', #16577, #51953 ) ;
#28825 = CARTESIAN_POINT ( 'NONE',  ( -18.22828877115104618, -0.1191753592594170102, 5.147885465369180125 ) ) ;
#28826 = PLANE ( 'NONE',  #35717 ) ;
#28827 = EDGE_CURVE ( 'NONE', #5706, #24756, #35236, .T. ) ;
#28828 = EDGE_LOOP ( 'NONE', ( #38962, #46769, #55424, #56150 ) ) ;
#28829 = VECTOR ( 'NONE', #46647, 999.9999999999998863 ) ;
#28830 = EDGE_CURVE ( 'NONE', #45510, #52648, #30941, .T. ) ;
#28831 = CARTESIAN_POINT ( 'NONE',  ( -19.05158305253015527, 3.038739411681507185, 9.268692036737574469 ) ) ;
#28832 = EDGE_LOOP ( 'NONE', ( #51588, #54786, #36786, #26492 ) ) ;
#28833 = EDGE_CURVE ( 'NONE', #13341, #49603, #844, .T. ) ;
#28834 = ORIENTED_EDGE ( 'NONE', *, *, #36107, .T. ) ;
#28835 = ORIENTED_EDGE ( 'NONE', *, *, #19334, .T. ) ;
#28836 = ORIENTED_EDGE ( 'NONE', *, *, #4885, .F. ) ;
#28837 = ORIENTED_EDGE ( 'NONE', *, *, #49744, .F. ) ;
#28838 = DIRECTION ( 'NONE',  ( 0.9999697198139515519, 0.000000000000000000, 0.007781995580013368816 ) ) ;
#28839 = EDGE_LOOP ( 'NONE', ( #20144, #155, #32359, #8041 ) ) ;
#28840 = ORIENTED_EDGE ( 'NONE', *, *, #18204, .T. ) ;
#28841 = DIRECTION ( 'NONE',  ( 0.000000000000000000, -0.000000000000000000, -1.000000000000000000 ) ) ;
#28842 = ORIENTED_EDGE ( 'NONE', *, *, #14757, .F. ) ;
#28843 = ORIENTED_EDGE ( 'NONE', *, *, #45431, .F. ) ;
#28844 = PLANE ( 'NONE',  #240 ) ;
#28845 = DIRECTION ( 'NONE',  ( -0.5449076811759708816, 0.6444004775717707689, 0.5364919789714475140 ) ) ;
#28846 = FACE_OUTER_BOUND ( 'NONE', #45694, .T. ) ;
#28847 = CARTESIAN_POINT ( 'NONE',  ( -20.79233874698950757, 1.257817950434006571, 7.022065141322721082 ) ) ;
#28848 = ORIENTED_EDGE ( 'NONE', *, *, #23016, .F. ) ;
#28849 = DIRECTION ( 'NONE',  ( -0.6427681459581293666, -0.7660444431189770143, -0.005002170337467561935 ) ) ;
#28850 = ORIENTED_EDGE ( 'NONE', *, *, #14953, .F. ) ;
#28851 = ORIENTED_EDGE ( 'NONE', *, *, #41292, .F. ) ;
#28852 = PLANE ( 'NONE',  #51196 ) ;
#28853 = EDGE_CURVE ( 'NONE', #26568, #19155, #6791, .T. ) ;
#28854 = CARTESIAN_POINT ( 'NONE',  ( -30.79411802867772607, 0.000000000000000000, 8.643412946479525516 ) ) ;
#28855 = CARTESIAN_POINT ( 'NONE',  ( -29.31353752332232077, 15.73409706589058388, -4.735829944523183954 ) ) ;
#28856 = DIRECTION ( 'NONE',  ( -0.005961354470445682716, -0.6427876096865404731, 0.7660212471507180654 ) ) ;
#28857 = CARTESIAN_POINT ( 'NONE',  ( 1.086233639165236964, 0.000000000000000000, 2.796443541562362078 ) ) ;
#28858 = CARTESIAN_POINT ( 'NONE',  ( -15.44046739010452818, -0.1191753592594188005, 5.169580935977237779 ) ) ;
#28859 = ORIENTED_EDGE ( 'NONE', *, *, #21713, .F. ) ;
#28860 = LINE ( 'NONE', #41623, #12022 ) ;
#28861 = ORIENTED_EDGE ( 'NONE', *, *, #22476, .T. ) ;
#28862 = EDGE_CURVE ( 'NONE', #54123, #15809, #37742, .T. ) ;
#28863 = VECTOR ( 'NONE', #5526, 1000.000000000000227 ) ;
#28864 = CARTESIAN_POINT ( 'NONE',  ( -6.110905869600904872, 1.712176620043476140E-14, -4.599999999999999645 ) ) ;
#28865 = FACE_OUTER_BOUND ( 'NONE', #48810, .T. ) ;
#28866 = CARTESIAN_POINT ( 'NONE',  ( -8.409922665610809034, 0.000000000000000000, 10.23674650875856962 ) ) ;
#28867 = DIRECTION ( 'NONE',  ( -0.005002170337468016433, -0.7660444431189770143, 0.6427681459581293666 ) ) ;
#28868 = EDGE_CURVE ( 'NONE', #24781, #20661, #11033, .T. ) ;
#28869 = EDGE_CURVE ( 'NONE', #54798, #30130, #6506, .T. ) ;
#28870 = CARTESIAN_POINT ( 'NONE',  ( -21.47341775636118655, -0.1191753592594197858, 5.122631121243466090 ) ) ;
#28871 = ORIENTED_EDGE ( 'NONE', *, *, #16339, .F. ) ;
#28872 = ORIENTED_EDGE ( 'NONE', *, *, #53075, .F. ) ;
#28873 = LINE ( 'NONE', #7275, #43899 ) ;
#28874 = CARTESIAN_POINT ( 'NONE',  ( 2.072287782118878319, 0.000000000000000000, -2.950529333540147015 ) ) ;
#28875 = CARTESIAN_POINT ( 'NONE',  ( -20.54049170961573267, 0.000000000000000000, 4.660556269540326646 ) ) ;
#28876 = LINE ( 'NONE', #37676, #30074 ) ;
#28877 = EDGE_CURVE ( 'NONE', #35256, #50946, #24648, .T. ) ;
#28878 = DIRECTION ( 'NONE',  ( 0.000000000000000000, 0.000000000000000000, -1.000000000000000000 ) ) ;
#28879 = CARTESIAN_POINT ( 'NONE',  ( -9.214449502844235695, 0.000000000000000000, 3.271369869658160567 ) ) ;
#28880 = CARTESIAN_POINT ( 'NONE',  ( -14.94838282604903057, -0.1191753592594194527, 2.588085963191248506 ) ) ;
#28881 = ADVANCED_FACE ( 'NONE', ( #37430 ), #49926, .F. ) ;
#28882 = CARTESIAN_POINT ( 'NONE',  ( -67.38882915104511540, -9.422359167723826090, 6.206396125462540603 ) ) ;
#28883 = CARTESIAN_POINT ( 'NONE',  ( -21.96455318448683514, 19.88593911322026742, 4.412914703902076852 ) ) ;
#28884 = EDGE_LOOP ( 'NONE', ( #8742, #44113, #32164, #33440, #13010 ) ) ;
#28885 = ADVANCED_FACE ( 'NONE', ( #2524 ), #28352, .F. ) ;
#28886 = ORIENTED_EDGE ( 'NONE', *, *, #28472, .T. ) ;
#28887 = EDGE_CURVE ( 'NONE', #13455, #10554, #23816, .T. ) ;
#28888 = ORIENTED_EDGE ( 'NONE', *, *, #50493, .T. ) ;
#28889 = EDGE_LOOP ( 'NONE', ( #40130, #8925, #52996, #50944 ) ) ;
#28890 = VERTEX_POINT ( 'NONE', #41443 ) ;
#28891 = ORIENTED_EDGE ( 'NONE', *, *, #22396, .F. ) ;
#28892 = LINE ( 'NONE', #16366, #41394 ) ;
#28893 = FACE_OUTER_BOUND ( 'NONE', #39438, .T. ) ;
#28894 = DIRECTION ( 'NONE',  ( 0.005002170337468016433, -0.7660444431189770143, -0.6427681459581293666 ) ) ;
#28895 = VECTOR ( 'NONE', #25363, 999.9999999999998863 ) ;
#28896 = ORIENTED_EDGE ( 'NONE', *, *, #20832, .F. ) ;
#28897 = CARTESIAN_POINT ( 'NONE',  ( -24.26986129792355129, -0.1191753592594197858, 6.208864760408702388 ) ) ;
#28898 = VERTEX_POINT ( 'NONE', #45675 ) ;
#28899 = LINE ( 'NONE', #46195, #24965 ) ;
#28900 = ORIENTED_EDGE ( 'NONE', *, *, #9773, .T. ) ;
#28901 = CARTESIAN_POINT ( 'NONE',  ( -68.39955523751335420, -8.932958699260208135, 6.466593069173195651 ) ) ;
#28902 = DIRECTION ( 'NONE',  ( -0.005961354470445682716, -0.6427876096865404731, 0.7660212471507180654 ) ) ;
#28903 = CARTESIAN_POINT ( 'NONE',  ( -11.56765945739309487, 0.2864062442990042978, 1.166065645416680008 ) ) ;
#28904 = ORIENTED_EDGE ( 'NONE', *, *, #8754, .T. ) ;
#28905 = CARTESIAN_POINT ( 'NONE',  ( -19.06984000643095456, 0.000000000000000000, 6.718667626403617810 ) ) ;
#28906 = ADVANCED_FACE ( 'NONE', ( #33206 ), #41147, .F. ) ;
#28907 = VERTEX_POINT ( 'NONE', #20400 ) ;
#28908 = DIRECTION ( 'NONE',  ( 0.5449076811759707706, 0.6444004775717708799, -0.5364919789714476250 ) ) ;
#28909 = EDGE_CURVE ( 'NONE', #8945, #16356, #49295, .T. ) ;
#28910 = LINE ( 'NONE', #46204, #10324 ) ;
#28911 = LINE ( 'NONE', #28068, #26934 ) ;
#28912 = EDGE_CURVE ( 'NONE', #21622, #25987, #11325, .T. ) ;
#28913 = FACE_OUTER_BOUND ( 'NONE', #28702, .T. ) ;
#28914 = LINE ( 'NONE', #45957, #17474 ) ;
#28915 = DIRECTION ( 'NONE',  ( -0.5449076811759708816, 0.6444004775717707689, 0.5364919789714475140 ) ) ;
#28916 = EDGE_CURVE ( 'NONE', #50409, #53549, #20100, .T. ) ;
#28917 = PLANE ( 'NONE',  #11252 ) ;
#28918 = CARTESIAN_POINT ( 'NONE',  ( -10.22162059191334116, 0.000000000000000000, 4.202202027191447087 ) ) ;
#28919 = ORIENTED_EDGE ( 'NONE', *, *, #33018, .T. ) ;
#28920 = DIRECTION ( 'NONE',  ( 0.3535533905932738974, -0.6123724356957929160, -0.7071067811865487940 ) ) ;
#28921 = ORIENTED_EDGE ( 'NONE', *, *, #13098, .F. ) ;
#28922 = EDGE_CURVE ( 'NONE', #21908, #11209, #28657, .T. ) ;
#28923 = EDGE_CURVE ( 'NONE', #21327, #12775, #7086, .T. ) ;
#28924 = ADVANCED_FACE ( 'NONE', ( #41690 ), #50519, .F. ) ;
#28925 = DIRECTION ( 'NONE',  ( 0.005002170337468016433, -0.7660444431189770143, -0.6427681459581293666 ) ) ;
#28926 = CARTESIAN_POINT ( 'NONE',  ( -15.56998309669674718, 0.000000000000000000, 8.961896740978279041 ) ) ;
#28927 = DIRECTION ( 'NONE',  ( 0.5449076811759707706, 0.6444004775717708799, -0.5364919789714476250 ) ) ;
#28928 = DIRECTION ( 'NONE',  ( -0.7660212471507179544, -0.6427876096865405842, -0.005961354470445141482 ) ) ;
#28929 = DIRECTION ( 'NONE',  ( -0.005961354470445682716, -0.6427876096865404731, 0.7660212471507180654 ) ) ;
#28930 = CARTESIAN_POINT ( 'NONE',  ( -18.63760471526975593, 0.9340140483890051470, 3.891610400377997436 ) ) ;
#28931 = CARTESIAN_POINT ( 'NONE',  ( 0.000000000000000000, 0.000000000000000000, 0.000000000000000000 ) ) ;
#28932 = ORIENTED_EDGE ( 'NONE', *, *, #28909, .T. ) ;
#28933 = DIRECTION ( 'NONE',  ( -0.5364919789714478471, 0.6444004775717705469, -0.5449076811759709926 ) ) ;
#28934 = DIRECTION ( 'NONE',  ( 0.005961354470445682716, -0.6427876096865404731, -0.7660212471507180654 ) ) ;
#28935 = LINE ( 'NONE', #41966, #20396 ) ;
#28936 = DIRECTION ( 'NONE',  ( 0.007781995580012662783, 0.000000000000000000, -0.9999697198139514409 ) ) ;
#28937 = LINE ( 'NONE', #2527, #570 ) ;
#28938 = DIRECTION ( 'NONE',  ( -0.5364919789714478471, 0.6444004775717705469, -0.5449076811759709926 ) ) ;
#28939 = ADVANCED_FACE ( 'NONE', ( #42276 ), #15043, .F. ) ;
#28940 = CARTESIAN_POINT ( 'NONE',  ( -17.32134905586179130, -3.432230869623160263, 9.043007527150438207 ) ) ;
#28941 = PLANE ( 'NONE',  #27746 ) ;
#28942 = LINE ( 'NONE', #20959, #22003 ) ;
#28943 = ORIENTED_EDGE ( 'NONE', *, *, #30548, .F. ) ;
#28944 = EDGE_CURVE ( 'NONE', #42380, #18980, #49684, .T. ) ;
#28945 = LINE ( 'NONE', #46238, #23999 ) ;
#28946 = CARTESIAN_POINT ( 'NONE',  ( -10.27421835998572064, 0.000000000000000000, 10.96090226820206048 ) ) ;
#28947 = ORIENTED_EDGE ( 'NONE', *, *, #39668, .F. ) ;
#28948 = EDGE_CURVE ( 'NONE', #43321, #41488, #34579, .T. ) ;
#28949 = DIRECTION ( 'NONE',  ( 0.7660212471507180654, -0.6427876096865404731, 0.005961354470445141482 ) ) ;
#28950 = CARTESIAN_POINT ( 'NONE',  ( -16.28333627977372089, 0.000000000000000000, 6.909678856306649131 ) ) ;
#28951 = ADVANCED_FACE ( 'NONE', ( #30339 ), #56172, .F. ) ;
#28952 = VERTEX_POINT ( 'NONE', #38274 ) ;
#28953 = VERTEX_POINT ( 'NONE', #51895 ) ;
#28954 = DIRECTION ( 'NONE',  ( 0.6427681459581294776, -0.7660444431189769032, 0.005002170337467562802 ) ) ;
#28955 = ORIENTED_EDGE ( 'NONE', *, *, #53470, .F. ) ;
#28956 = VERTEX_POINT ( 'NONE', #42811 ) ;
#28957 = ORIENTED_EDGE ( 'NONE', *, *, #2887, .F. ) ;
#28958 = FACE_OUTER_BOUND ( 'NONE', #42446, .T. ) ;
#28959 = CARTESIAN_POINT ( 'NONE',  ( -17.74404816805336793, 0.000000000000000000, 3.574322630375089460 ) ) ;
#28960 = FACE_OUTER_BOUND ( 'NONE', #6601, .T. ) ;
#28961 = ORIENTED_EDGE ( 'NONE', *, *, #10498, .T. ) ;
#28962 = ORIENTED_EDGE ( 'NONE', *, *, #37666, .T. ) ;
#28963 = LINE ( 'NONE', #20726, #19390 ) ;
#28964 = DIRECTION ( 'NONE',  ( 0.005961354470445682716, -0.6427876096865404731, -0.7660212471507180654 ) ) ;
#28965 = ORIENTED_EDGE ( 'NONE', *, *, #9412, .T. ) ;
#28966 = CARTESIAN_POINT ( 'NONE',  ( 2.072287782118878319, 0.000000000000000000, -2.950529333540147015 ) ) ;
#28967 = ORIENTED_EDGE ( 'NONE', *, *, #9718, .F. ) ;
#28968 = LINE ( 'NONE', #26312, #52099 ) ;
#28969 = CARTESIAN_POINT ( 'NONE',  ( -16.85955541371576771, 3.200641362704007786, 8.682942744200573770 ) ) ;
#28970 = EDGE_LOOP ( 'NONE', ( #43543, #29040, #29063, #1541, #47384 ) ) ;
#28971 = PLANE ( 'NONE',  #13731 ) ;
#28972 = EDGE_CURVE ( 'NONE', #16128, #2673, #21243, .T. ) ;
#28973 = CARTESIAN_POINT ( 'NONE',  ( -11.85736786543846932, -1.975113310420660184, 1.424109018569633234 ) ) ;
#28974 = VERTEX_POINT ( 'NONE', #7932 ) ;
#28975 = DIRECTION ( 'NONE',  ( 0.6427681459581294776, -0.7660444431189769032, 0.005002170337467562802 ) ) ;
#28976 = SURFACE_STYLE_FILL_AREA ( #11661 ) ;
#28977 = DIRECTION ( 'NONE',  ( 0.9999697198139515519, 0.000000000000000000, 0.007781995580013368816 ) ) ;
#28978 = ORIENTED_EDGE ( 'NONE', *, *, #8767, .F. ) ;
#28979 = ADVANCED_FACE ( 'NONE', ( #201 ), #25499, .F. ) ;
#28980 = EDGE_CURVE ( 'NONE', #39017, #43351, #55597, .T. ) ;
#28981 = ADVANCED_FACE ( 'NONE', ( #47938 ), #13012, .F. ) ;
#28982 = PLANE ( 'NONE',  #26507 ) ;
#28983 = DIRECTION ( 'NONE',  ( -0.005002170337468016433, -0.7660444431189770143, 0.6427681459581293666 ) ) ;
#28984 = CARTESIAN_POINT ( 'NONE',  ( -17.26532721389163072, 0.000000000000000000, 13.67648636611514590 ) ) ;
#28985 = LINE ( 'NONE', #28415, #2327 ) ;
#28986 = EDGE_CURVE ( 'NONE', #29764, #47771, #43398, .T. ) ;
#28987 = DIRECTION ( 'NONE',  ( 0.000000000000000000, 1.000000000000000000, 0.000000000000000000 ) ) ;
#28988 = DIRECTION ( 'NONE',  ( 0.000000000000000000, -0.000000000000000000, -1.000000000000000000 ) ) ;
#28989 = CARTESIAN_POINT ( 'NONE',  ( -28.93137873341882127, 0.000000000000000000, 8.119251130998824451 ) ) ;
#28990 = ORIENTED_EDGE ( 'NONE', *, *, #8329, .F. ) ;
#28991 = FACE_OUTER_BOUND ( 'NONE', #34565, .T. ) ;
#28992 = DIRECTION ( 'NONE',  ( -0.5364919789714478471, 0.6444004775717705469, -0.5449076811759709926 ) ) ;
#28993 = LINE ( 'NONE', #3437, #13297 ) ;
#28994 = ORIENTED_EDGE ( 'NONE', *, *, #8740, .F. ) ;
#28995 = LINE ( 'NONE', #49991, #37447 ) ;
#28996 = DIRECTION ( 'NONE',  ( 0.5364919789714477361, 0.6444004775717706579, 0.5449076811759711036 ) ) ;
#28997 = DIRECTION ( 'NONE',  ( 0.9999697198139515519, 0.000000000000000000, 0.007781995580013368816 ) ) ;
#28998 = DIRECTION ( 'NONE',  ( -0.6427681459581293666, -0.7660444431189770143, -0.005002170337467561935 ) ) ;
#28999 = EDGE_CURVE ( 'NONE', #46991, #51210, #30636, .T. ) ;
#29000 = CARTESIAN_POINT ( 'NONE',  ( -20.56670277481199349, 0.4483081953215036219, 5.605877047346789155 ) ) ;
#29001 = ORIENTED_EDGE ( 'NONE', *, *, #9500, .T. ) ;
#29002 = ORIENTED_EDGE ( 'NONE', *, *, #15690, .F. ) ;
#29003 = EDGE_CURVE ( 'NONE', #32478, #21588, #26338, .T. ) ;
#29004 = DIRECTION ( 'NONE',  ( -0.7660212471507179544, -0.6427876096865405842, -0.005961354470445141482 ) ) ;
#29005 = DIRECTION ( 'NONE',  ( 0.9999697198139515519, 0.000000000000000000, 0.007781995580013368816 ) ) ;
#29006 = ADVANCED_FACE ( 'NONE', ( #38012 ), #55901, .F. ) ;
#29007 = ORIENTED_EDGE ( 'NONE', *, *, #38025, .F. ) ;
#29008 = CARTESIAN_POINT ( 'NONE',  ( -12.72599829993386322, 0.000000000000000000, 1.766713905726021938 ) ) ;
#29009 = VERTEX_POINT ( 'NONE', #8191 ) ;
#29010 = CARTESIAN_POINT ( 'NONE',  ( -12.40227819300294954, -2.622721114510660367, 1.615108615478732190 ) ) ;
#29011 = EDGE_CURVE ( 'NONE', #53934, #3513, #33679, .T. ) ;
#29012 = VERTEX_POINT ( 'NONE', #17851 ) ;
#29013 = VERTEX_POINT ( 'NONE', #35718 ) ;
#29014 = VERTEX_POINT ( 'NONE', #35180 ) ;
#29015 = LINE ( 'NONE', #45480, #38380 ) ;
#29016 = DIRECTION ( 'NONE',  ( 0.5364919789714477361, 0.6444004775717706579, 0.5449076811759711036 ) ) ;
#29017 = LINE ( 'NONE', #46313, #41174 ) ;
#29018 = EDGE_LOOP ( 'NONE', ( #33307, #19921, #42369, #48235 ) ) ;
#29019 = DIRECTION ( 'NONE',  ( 0.6427681459581294776, -0.7660444431189769032, 0.005002170337467562802 ) ) ;
#29020 = VERTEX_POINT ( 'NONE', #52474 ) ;
#29021 = EDGE_LOOP ( 'NONE', ( #34287, #44805, #8491, #36303 ) ) ;
#29022 = ORIENTED_EDGE ( 'NONE', *, *, #1647, .T. ) ;
#29023 = LINE ( 'NONE', #12560, #22261 ) ;
#29024 = FACE_OUTER_BOUND ( 'NONE', #35030, .T. ) ;
#29025 = VERTEX_POINT ( 'NONE', #53033 ) ;
#29026 = DIRECTION ( 'NONE',  ( 0.3313982828793700097, 0.4028455766673915694, 0.8531650599175529814 ) ) ;
#29027 = VERTEX_POINT ( 'NONE', #14150 ) ;
#29028 = CARTESIAN_POINT ( 'NONE',  ( 2.072287782118878319, 0.000000000000000000, -2.950529333540147015 ) ) ;
#29029 = DIRECTION ( 'NONE',  ( 0.8660254037844380415, 0.5000000000000011102, 0.000000000000000000 ) ) ;
#29030 = ORIENTED_EDGE ( 'NONE', *, *, #22495, .T. ) ;
#29031 = FACE_OUTER_BOUND ( 'NONE', #6235, .T. ) ;
#29032 = ORIENTED_EDGE ( 'NONE', *, *, #5251, .F. ) ;
#29033 = VECTOR ( 'NONE', #15293, 999.9999999999998863 ) ;
#29034 = LINE ( 'NONE', #11981, #45516 ) ;
#29035 = CARTESIAN_POINT ( 'NONE',  ( -14.14290141849938465, 0.000000000000000000, 4.710343796484107948 ) ) ;
#29036 = DIRECTION ( 'NONE',  ( 0.000000000000000000, -0.000000000000000000, -1.000000000000000000 ) ) ;
#29037 = LINE ( 'NONE', #46336, #2127 ) ;
#29038 = CARTESIAN_POINT ( 'NONE',  ( -20.69024277472754392, 2.229229656569007290, 8.576659702205136071 ) ) ;
#29039 = FACE_OUTER_BOUND ( 'NONE', #9379, .T. ) ;
#29040 = ORIENTED_EDGE ( 'NONE', *, *, #9376, .T. ) ;
#29041 = ADVANCED_FACE ( 'NONE', ( #22927 ), #53577, .F. ) ;
#29042 = EDGE_LOOP ( 'NONE', ( #52300, #11934, #55421, #1407 ) ) ;
#29043 = DIRECTION ( 'NONE',  ( 0.007781995580012663651, -3.146120232559066537E-19, -0.9999697198139514409 ) ) ;
#29044 = DIRECTION ( 'NONE',  ( 0.6427681459581294776, -0.7660444431189769032, 0.005002170337467562802 ) ) ;
#29045 = DIRECTION ( 'NONE',  ( -0.9999697198139514409, -0.000000000000000000, -0.007781995580013368816 ) ) ;
#29046 = ADVANCED_FACE ( 'NONE', ( #31475 ), #13838, .F. ) ;
#29047 = EDGE_CURVE ( 'NONE', #18224, #34917, #31164, .T. ) ;
#29048 = CARTESIAN_POINT ( 'NONE',  ( -12.33850799832341849, 0.000000000000000000, 11.68350162852954632 ) ) ;
#29049 = DIRECTION ( 'NONE',  ( 0.7660212471507180654, -0.6427876096865404731, 0.005961354470445141482 ) ) ;
#29050 = CARTESIAN_POINT ( 'NONE',  ( -19.06696595292567054, 0.000000000000000000, 6.349357923145855231 ) ) ;
#29051 = ORIENTED_EDGE ( 'NONE', *, *, #3553, .F. ) ;
#29052 = CARTESIAN_POINT ( 'NONE',  ( -20.54126990917373519, -0.1191753592594197858, 4.760553241521720658 ) ) ;
#29053 = DIRECTION ( 'NONE',  ( 0.000000000000000000, -1.000000000000000000, 0.000000000000000000 ) ) ;
#29054 = VERTEX_POINT ( 'NONE', #48489 ) ;
#29055 = CARTESIAN_POINT ( 'NONE',  ( -15.18422100874571434, -5.375054281893165253, 2.607895842203279191 ) ) ;
#29056 = FACE_OUTER_BOUND ( 'NONE', #42054, .T. ) ;
#29057 = ORIENTED_EDGE ( 'NONE', *, *, #6811, .T. ) ;
#29058 = CARTESIAN_POINT ( 'NONE',  ( -70.75814845257580998, 2.000000000000000000, 8.563005977519216216 ) ) ;
#29059 = DIRECTION ( 'NONE',  ( -0.5449076811759708816, 0.6444004775717707689, 0.5364919789714475140 ) ) ;
#29060 = PLANE ( 'NONE',  #6898 ) ;
#29061 = CARTESIAN_POINT ( 'NONE',  ( -13.96302584907357236, 0.000000000000000000, 7.297068118404461678 ) ) ;
#29062 = PLANE ( 'NONE',  #2918 ) ;
#29063 = ORIENTED_EDGE ( 'NONE', *, *, #18230, .T. ) ;
#29064 = ORIENTED_EDGE ( 'NONE', *, *, #36544, .T. ) ;
#29065 = PLANE ( 'NONE',  #16738 ) ;
#29066 = PLANE ( 'NONE',  #33141 ) ;
#29067 = DIRECTION ( 'NONE',  ( 0.9999697198139515519, 0.000000000000000000, 0.007781995580013368816 ) ) ;
#29068 = DIRECTION ( 'NONE',  ( -0.5364919789714478471, 0.6444004775717705469, -0.5449076811759709926 ) ) ;
#29069 = CARTESIAN_POINT ( 'NONE',  ( -10.74029228357944987, 0.000000000000000000, 11.14194120806293320 ) ) ;
#29070 = CARTESIAN_POINT ( 'NONE',  ( -16.81345671998191449, 0.000000000000000000, 3.412238694616132495 ) ) ;
#29071 = ORIENTED_EDGE ( 'NONE', *, *, #15048, .F. ) ;
#29072 = CARTESIAN_POINT ( 'NONE',  ( -12.58558820878208451, 4.819660872929013351, 1.416829184615139736 ) ) ;
#29073 = ADVANCED_FACE ( 'NONE', ( #35429 ), #4766, .F. ) ;
#29074 = VECTOR ( 'NONE', #12396, 999.9999999999998863 ) ;
#29075 = LINE ( 'NONE', #16293, #53216 ) ;
#29076 = CARTESIAN_POINT ( 'NONE',  ( -12.73905091307099546, 0.000000000000000000, 3.443946662719867824 ) ) ;
#29077 = EDGE_LOOP ( 'NONE', ( #4398, #16741, #50396, #25585 ) ) ;
#29078 = EDGE_CURVE ( 'NONE', #46919, #38778, #48190, .T. ) ;
#29079 = CARTESIAN_POINT ( 'NONE',  ( -11.64304826723200570, 25.38767603887662716, -5.000000000092198249 ) ) ;
#29080 = CARTESIAN_POINT ( 'NONE',  ( -15.86710544311044302, 0.000000000000000000, 13.13336954653252953 ) ) ;
#29081 = FACE_OUTER_BOUND ( 'NONE', #18564, .T. ) ;
#29082 = EDGE_LOOP ( 'NONE', ( #978, #21335, #31461, #21467, #54957 ) ) ;
#29083 = LINE ( 'NONE', #54107, #44048 ) ;
#29084 = EDGE_CURVE ( 'NONE', #49698, #9775, #44243, .T. ) ;
#29085 = ORIENTED_EDGE ( 'NONE', *, *, #40217, .T. ) ;
#29086 = ORIENTED_EDGE ( 'NONE', *, *, #558, .T. ) ;
#29087 = ORIENTED_EDGE ( 'NONE', *, *, #51435, .F. ) ;
#29088 = ORIENTED_EDGE ( 'NONE', *, *, #51854, .T. ) ;
#29089 = CARTESIAN_POINT ( 'NONE',  ( -14.20280369269832832, 0.000000000000000000, 12.40765738797303719 ) ) ;
#29090 = ORIENTED_EDGE ( 'NONE', *, *, #14445, .T. ) ;
#29091 = VECTOR ( 'NONE', #28589, 1000.000000000000227 ) ;
#29092 = ORIENTED_EDGE ( 'NONE', *, *, #28139, .T. ) ;
#29093 = CARTESIAN_POINT ( 'NONE',  ( -14.66887761629205222, 0.000000000000000000, 12.58869632783390990 ) ) ;
#29094 = ORIENTED_EDGE ( 'NONE', *, *, #46890, .F. ) ;
#29095 = EDGE_LOOP ( 'NONE', ( #48963, #49236, #26579, #1839 ) ) ;
#29096 = CARTESIAN_POINT ( 'NONE',  ( -16.76798113924479239, -2.784623065533159636, 7.765225900080996446 ) ) ;
#29097 = LINE ( 'NONE', #6995, #35776 ) ;
#29098 = DIRECTION ( 'NONE',  ( -0.5449076811759708816, 0.6444004775717707689, 0.5364919789714475140 ) ) ;
#29099 = FACE_OUTER_BOUND ( 'NONE', #47013, .T. ) ;
#29100 = EDGE_CURVE ( 'NONE', #52840, #46950, #43943, .T. ) ;
#29101 = DIRECTION ( 'NONE',  ( 0.7660212471507180654, -0.6427876096865404731, 0.005961354470445141482 ) ) ;
#29102 = VERTEX_POINT ( 'NONE', #5066 ) ;
#29103 = ORIENTED_EDGE ( 'NONE', *, *, #47699, .F. ) ;
#29104 = VECTOR ( 'NONE', #15913, 1000.000000000000227 ) ;
#29105 = DIRECTION ( 'NONE',  ( 0.007781995580012663651, 0.000000000000000000, -0.9999697198139515519 ) ) ;
#29106 = LINE ( 'NONE', #2697, #46624 ) ;
#29107 = PRODUCT_DEFINITION_CONTEXT ( 'detailed design', #16258, 'design' ) ;
#29108 = EDGE_CURVE ( 'NONE', #43993, #36408, #9608, .T. ) ;
#29109 = EDGE_CURVE ( 'NONE', #23095, #45238, #26931, .T. ) ;
#29110 = VECTOR ( 'NONE', #3921, 999.9999999999998863 ) ;
#29111 = FACE_OUTER_BOUND ( 'NONE', #48866, .T. ) ;
#29112 = CARTESIAN_POINT ( 'NONE',  ( -58.00000000000000711, -9.000000000000000000, 7.102951435054649637E-15 ) ) ;
#29113 = CARTESIAN_POINT ( 'NONE',  ( -15.88130887279446490, 0.000000000000000000, 3.050160814894388839 ) ) ;
#29114 = PLANE ( 'NONE',  #40453 ) ;
#29115 = VERTEX_POINT ( 'NONE', #36025 ) ;
#29116 = DIRECTION ( 'NONE',  ( -0.6427681459581293666, -0.7660444431189770143, -0.005002170337467561935 ) ) ;
#29117 = DIRECTION ( 'NONE',  ( -0.9999697198139514409, -0.000000000000000000, -0.007781995580013368816 ) ) ;
#29118 = ORIENTED_EDGE ( 'NONE', *, *, #24192, .T. ) ;
#29119 = FACE_OUTER_BOUND ( 'NONE', #42996, .T. ) ;
#29120 = CARTESIAN_POINT ( 'NONE',  ( -13.23662005285947174, 0.000000000000000000, 7.672053246082242595 ) ) ;
#29121 = PLANE ( 'NONE',  #9993 ) ;
#29122 = DIRECTION ( 'NONE',  ( 0.000000000000000000, -0.000000000000000000, -1.000000000000000000 ) ) ;
#29124 = DIRECTION ( 'NONE',  ( 0.007781995580012662783, 0.000000000000000000, -0.9999697198139514409 ) ) ;
#29123 = B_SPLINE_CURVE_WITH_KNOTS ( 'NONE', 3,
 ( #54014, #23623, #41227, #10849 ),
 .UNSPECIFIED., .F., .F.,
 ( 4, 4 ),
 ( 0.0002015054463949536242, 0.0003537000219815807046 ),
 .UNSPECIFIED. ) ;
#29125 = EDGE_CURVE ( 'NONE', #55742, #32296, #786, .T. ) ;
#29126 = ORIENTED_EDGE ( 'NONE', *, *, #26524, .T. ) ;
#29127 = ORIENTED_EDGE ( 'NONE', *, *, #30206, .F. ) ;
#29128 = CARTESIAN_POINT ( 'NONE',  ( -15.52954537527145185, -5.698858183938162902, 12.06693170300650308 ) ) ;
#29129 = FACE_OUTER_BOUND ( 'NONE', #34096, .T. ) ;
#29130 = CARTESIAN_POINT ( 'NONE',  ( -20.82430447243409333, -2.622721114510657703, 9.075130952061487122 ) ) ;
#29131 = VECTOR ( 'NONE', #205, 999.9999999999998863 ) ;
#29132 = VECTOR ( 'NONE', #20674, 1000.000000000000000 ) ;
#29133 = DIRECTION ( 'NONE',  ( 0.007781995580012663651, -3.146120232559066537E-19, -0.9999697198139514409 ) ) ;
#29134 = DIRECTION ( 'NONE',  ( 0.6427681459581294776, -0.7660444431189769032, 0.005002170337467562802 ) ) ;
#29135 = CARTESIAN_POINT ( 'NONE',  ( -12.97875704852626022, 25.16498697016756836, -3.499616475124794679 ) ) ;
#29136 = CARTESIAN_POINT ( 'NONE',  ( -23.33693525117809386, 0.000000000000000000, 5.746789908705562944 ) ) ;
#29137 = DIRECTION ( 'NONE',  ( 0.007781995580012662783, 0.000000000000000000, -0.9999697198139514409 ) ) ;
#29138 = LINE ( 'NONE', #51301, #7447 ) ;
#29139 = ORIENTED_EDGE ( 'NONE', *, *, #31628, .T. ) ;
#29140 = CARTESIAN_POINT ( 'NONE',  ( 2.072287782118878319, 0.000000000000000000, -2.950529333540147015 ) ) ;
#29141 = EDGE_LOOP ( 'NONE', ( #16430, #11414, #11955 ) ) ;
#29142 = ADVANCED_FACE ( 'NONE', ( #44494 ), #31736, .F. ) ;
#29143 = AXIS2_PLACEMENT_3D ( 'NONE', #28966, #49433, #46015 ) ;
#29144 = ORIENTED_EDGE ( 'NONE', *, *, #47487, .F. ) ;
#29145 = VERTEX_POINT ( 'NONE', #27463 ) ;
#29146 = ORIENTED_EDGE ( 'NONE', *, *, #13639, .F. ) ;
#29147 = VERTEX_POINT ( 'NONE', #52732 ) ;
#29148 = DIRECTION ( 'NONE',  ( -0.5364919789714478471, 0.6444004775717705469, -0.5449076811759709926 ) ) ;
#29149 = DIRECTION ( 'NONE',  ( -0.005002170337468016433, -0.7660444431189770143, 0.6427681459581293666 ) ) ;
#29150 = LINE ( 'NONE', #51004, #13088 ) ;
#29151 = ADVANCED_FACE ( 'NONE', ( #22652 ), #39963, .F. ) ;
#29152 = ORIENTED_EDGE ( 'NONE', *, *, #19914, .T. ) ;
#29153 = VERTEX_POINT ( 'NONE', #45611 ) ;
#29154 = ORIENTED_EDGE ( 'NONE', *, *, #27082, .T. ) ;
#29155 = FACE_OUTER_BOUND ( 'NONE', #46664, .T. ) ;
#29156 = EDGE_CURVE ( 'NONE', #12964, #17849, #46171, .T. ) ;
#29157 = EDGE_LOOP ( 'NONE', ( #51149, #11912, #22253, #20258 ) ) ;
#29158 = EDGE_CURVE ( 'NONE', #31213, #10988, #54995, .T. ) ;
#29159 = CARTESIAN_POINT ( 'NONE',  ( -66.37927290664002555, -9.306589109140311677, 3.533109812937361927 ) ) ;
#29160 = CARTESIAN_POINT ( 'NONE',  ( -10.19678563399013527, -0.07627425201977861002, 0.7424042488757021108 ) ) ;
#29161 = CARTESIAN_POINT ( 'NONE',  ( -14.15439763252051364, 0.000000000000000000, 6.187582609515166254 ) ) ;
#29162 = EDGE_CURVE ( 'NONE', #280, #2618, #44755, .T. ) ;
#29163 = VERTEX_POINT ( 'NONE', #24325 ) ;
#29164 = DIRECTION ( 'NONE',  ( 0.005002170337468016433, -0.7660444431189770143, -0.6427681459581293666 ) ) ;
#29165 = EDGE_LOOP ( 'NONE', ( #937, #31502, #24348, #22538 ) ) ;
#29166 = AXIS2_PLACEMENT_3D ( 'NONE', #14431, #10147, #40559 ) ;
#29167 = VECTOR ( 'NONE', #28194, 999.9999999999998863 ) ;
#29168 = DIRECTION ( 'NONE',  ( 0.9321478471874541372, 0.000000000000000000, -0.3620778797217453771 ) ) ;
#29169 = EDGE_CURVE ( 'NONE', #20216, #15750, #6725, .T. ) ;
#29170 = PLANE ( 'NONE',  #16636 ) ;
#29171 = EDGE_CURVE ( 'NONE', #19445, #51083, #15792, .T. ) ;
#29172 = CARTESIAN_POINT ( 'NONE',  ( -13.97320440870542413, 0.000000000000000000, 8.604991172140545430 ) ) ;
#29173 = AXIS2_PLACEMENT_3D ( 'NONE', #3855, #38215, #25441 ) ;
#29174 = DIRECTION ( 'NONE',  ( 0.9999697198139515519, 0.000000000000000000, 0.007781995580013368816 ) ) ;
#29175 = FACE_OUTER_BOUND ( 'NONE', #34467, .T. ) ;
#29176 = CARTESIAN_POINT ( 'NONE',  ( -22.40478740399063895, 0.000000000000000000, 5.384712028983816623 ) ) ;
#29177 = DIRECTION ( 'NONE',  ( 0.7660212471507180654, -0.6427876096865404731, 0.005961354470445141482 ) ) ;
#29178 = DIRECTION ( 'NONE',  ( 0.5449076811759707706, 0.6444004775717708799, -0.5364919789714476250 ) ) ;
#29179 = EDGE_LOOP ( 'NONE', ( #50799, #37379, #40971, #49700 ) ) ;
#29180 = CARTESIAN_POINT ( 'NONE',  ( -14.93495759592298988, 0.000000000000000000, 12.77129166681078409 ) ) ;
#29181 = ORIENTED_EDGE ( 'NONE', *, *, #11319, .F. ) ;
#29182 = EDGE_CURVE ( 'NONE', #29459, #13435, #28033, .T. ) ;
#29183 = LINE ( 'NONE', #51618, #27443 ) ;
#29184 = CARTESIAN_POINT ( 'NONE',  ( -27.06552663992790997, 0.000000000000000000, 7.195101427592543786 ) ) ;
#29185 = DIRECTION ( 'NONE',  ( 0.7660212471507180654, -0.6427876096865404731, 0.005961354470445141482 ) ) ;
#29186 = VECTOR ( 'NONE', #2749, 1000.000000000000227 ) ;
#29187 = DIRECTION ( 'NONE',  ( -0.6427681459581293666, -0.7660444431189770143, -0.005002170337467561935 ) ) ;
#29188 = DIRECTION ( 'NONE',  ( 0.9999697198139515519, 0.000000000000000000, 0.007781995580013368816 ) ) ;
#29189 = AXIS2_PLACEMENT_3D ( 'NONE', #16975, #55566, #38540 ) ;
#29190 = EDGE_CURVE ( 'NONE', #52307, #52077, #37363, .T. ) ;
#29191 = PLANE ( 'NONE',  #42015 ) ;
#29192 = EDGE_LOOP ( 'NONE', ( #3877, #1391, #52383, #15754 ) ) ;
#29193 = CARTESIAN_POINT ( 'NONE',  ( -10.78547626117782521, -0.1191753592594183703, 4.097810943884039325 ) ) ;
#29194 = DIRECTION ( 'NONE',  ( 0.007781995580012663651, 0.000000000000000000, -0.9999697198139515519 ) ) ;
#29195 = LINE ( 'NONE', #12162, #10408 ) ;
#29196 = FACE_OUTER_BOUND ( 'NONE', #45627, .T. ) ;
#29197 = DIRECTION ( 'NONE',  ( 0.005961354470445682716, -0.6427876096865404731, -0.7660212471507180654 ) ) ;
#29198 = CARTESIAN_POINT ( 'NONE',  ( -15.40103151951671734, 0.000000000000000000, 12.95233060667165681 ) ) ;
#29199 = CARTESIAN_POINT ( 'NONE',  ( -12.98732645422466092, 1.419719901456506728, 1.681353879868476842 ) ) ;
#29200 = DIRECTION ( 'NONE',  ( -0.005961354470445682716, -0.6427876096865404731, 0.7660212471507180654 ) ) ;
#29201 = EDGE_LOOP ( 'NONE', ( #52517, #41518, #39440, #1014 ) ) ;
#29202 = LINE ( 'NONE', #55073, #33082 ) ;
#29203 = LINE ( 'NONE', #3648, #55000 ) ;
#29204 = ORIENTED_EDGE ( 'NONE', *, *, #27983, .F. ) ;
#29205 = AXIS2_PLACEMENT_3D ( 'NONE', #43939, #38859, #52189 ) ;
#29206 = VERTEX_POINT ( 'NONE', #45340 ) ;
#29207 = FACE_OUTER_BOUND ( 'NONE', #40544, .T. ) ;
#29208 = VECTOR ( 'NONE', #21259, 1000.000000000000227 ) ;
#29209 = VECTOR ( 'NONE', #10572, 1000.000000000000000 ) ;
#29210 = ORIENTED_EDGE ( 'NONE', *, *, #52981, .T. ) ;
#29211 = EDGE_CURVE ( 'NONE', #39021, #56226, #28873, .T. ) ;
#29212 = ORIENTED_EDGE ( 'NONE', *, *, #45969, .T. ) ;
#29213 = PLANE ( 'NONE',  #54652 ) ;
#29214 = AXIS2_PLACEMENT_3D ( 'NONE', #5003, #8989, #39659 ) ;
#29215 = ORIENTED_EDGE ( 'NONE', *, *, #7986, .F. ) ;
#29216 = ORIENTED_EDGE ( 'NONE', *, *, #27490, .T. ) ;
#29217 = VECTOR ( 'NONE', #18500, 1000.000000000000114 ) ;
#29218 = ORIENTED_EDGE ( 'NONE', *, *, #48105, .F. ) ;
#29219 = DIRECTION ( 'NONE',  ( 0.9999697198139515519, 0.000000000000000000, 0.007781995580013368816 ) ) ;
#29220 = DIRECTION ( 'NONE',  ( 0.007781995580012663651, -3.146120232559066537E-19, -0.9999697198139514409 ) ) ;
#29221 = LINE ( 'NONE', #20977, #31245 ) ;
#29222 = EDGE_CURVE ( 'NONE', #12684, #11612, #16089, .T. ) ;
#29223 = EDGE_CURVE ( 'NONE', #10342, #20845, #2999, .T. ) ;
#29224 = VERTEX_POINT ( 'NONE', #50718 ) ;
#29225 = VECTOR ( 'NONE', #30803, 1000.000000000000227 ) ;
#29226 = EDGE_LOOP ( 'NONE', ( #21900, #47742, #38980 ) ) ;
#29227 = ADVANCED_FACE ( 'NONE', ( #37107 ), #45090, .T. ) ;
#29228 = CARTESIAN_POINT ( 'NONE',  ( -12.64689790204744746, -0.1191753592594185784, 4.452657000069766724 ) ) ;
#29229 = CARTESIAN_POINT ( 'NONE',  ( -18.67775241435682432, 0.000000000000000000, 4.136394454059623804 ) ) ;
#29230 = ORIENTED_EDGE ( 'NONE', *, *, #40399, .F. ) ;
#29231 = PLANE ( 'NONE',  #46365 ) ;
#29232 = ORIENTED_EDGE ( 'NONE', *, *, #33888, .F. ) ;
#29233 = CARTESIAN_POINT ( 'NONE',  ( 2.072287782118878319, 0.000000000000000000, -2.950529333540147015 ) ) ;
#29234 = CARTESIAN_POINT ( 'NONE',  ( -16.99924723426068951, 0.000000000000000000, 13.49389102713827171 ) ) ;
#29235 = ORIENTED_EDGE ( 'NONE', *, *, #9792, .F. ) ;
#29236 = CARTESIAN_POINT ( 'NONE',  ( -17.74560456716937296, 0.000000000000000000, 3.774316574337878372 ) ) ;
#29237 = EDGE_CURVE ( 'NONE', #50606, #25455, #6192, .T. ) ;
#29238 = VECTOR ( 'NONE', #9524, 1000.000000000000000 ) ;
#29239 = EDGE_CURVE ( 'NONE', #39009, #28807, #28582, .T. ) ;
#29240 = LINE ( 'NONE', #49723, #52657 ) ;
#29241 = VERTEX_POINT ( 'NONE', #54158 ) ;
#29242 = PLANE ( 'NONE',  #6797 ) ;
#29243 = DIRECTION ( 'NONE',  ( 0.9999697198139515519, 0.000000000000000000, 0.007781995580013368816 ) ) ;
#29244 = AXIS2_PLACEMENT_3D ( 'NONE', #23084, #19084, #23376 ) ;
#29245 = CARTESIAN_POINT ( 'NONE',  ( -14.94916102560700821, 0.000000000000000000, 2.688082935172642962 ) ) ;
#29246 = ORIENTED_EDGE ( 'NONE', *, *, #32424, .T. ) ;
#29247 = AXIS2_PLACEMENT_3D ( 'NONE', #19284, #1953, #36625 ) ;
#29248 = EDGE_CURVE ( 'NONE', #36041, #17041, #40812, .T. ) ;
#29249 = VECTOR ( 'NONE', #18671, 1000.000000000000227 ) ;
#29250 = DIRECTION ( 'NONE',  ( 0.000000000000000000, -1.000000000000000000, 0.000000000000000000 ) ) ;
#29251 = CARTESIAN_POINT ( 'NONE',  ( -12.60458797795435615, 0.000000000000000000, 11.86609696750642229 ) ) ;
#29252 = LINE ( 'NONE', #51419, #10417 ) ;
#29253 = LINE ( 'NONE', #33797, #38619 ) ;
#29254 = PLANE ( 'NONE',  #48516 ) ;
#29255 = DIRECTION ( 'NONE',  ( -0.5449076811759708816, 0.6444004775717707689, 0.5364919789714475140 ) ) ;
#29256 = AXIS2_PLACEMENT_3D ( 'NONE', #4096, #26229, #43540 ) ;
#29257 = CARTESIAN_POINT ( 'NONE',  ( -18.39746900504187010, 0.000000000000000000, 14.03700784672088808 ) ) ;
#29258 = VECTOR ( 'NONE', #36901, 1000.000000000000227 ) ;
#29259 = ORIENTED_EDGE ( 'NONE', *, *, #5132, .F. ) ;
#29260 = LINE ( 'NONE', #37502, #23506 ) ;
#29261 = PLANE ( 'NONE',  #34171 ) ;
#29262 = EDGE_LOOP ( 'NONE', ( #26930, #20947, #19534, #1453 ) ) ;
#29263 = LINE ( 'NONE', #6870, #11185 ) ;
#29264 = CARTESIAN_POINT ( 'NONE',  ( -10.37421533196711465, -0.1191753592594197858, 10.96012406864405975 ) ) ;
#29265 = DIRECTION ( 'NONE',  ( -0.9999697198139514409, -0.000000000000000000, -0.007781995580013368816 ) ) ;
#29266 = AXIS2_PLACEMENT_3D ( 'NONE', #28336, #11596, #23532 ) ;
#29267 = VECTOR ( 'NONE', #18847, 1000.000000000000114 ) ;
#29268 = CARTESIAN_POINT ( 'NONE',  ( -30.79567442779373110, 0.000000000000000000, 8.843406890442315316 ) ) ;
#29269 = LINE ( 'NONE', #29000, #52874 ) ;
#29270 = ORIENTED_EDGE ( 'NONE', *, *, #2194, .T. ) ;
#29271 = ORIENTED_EDGE ( 'NONE', *, *, #35746, .T. ) ;
#29272 = PLANE ( 'NONE',  #35911 ) ;
#29273 = CARTESIAN_POINT ( 'NONE',  ( -9.110551994824897193, -1.000000000000000000, 3.538847790438064411 ) ) ;
#29274 = EDGE_CURVE ( 'NONE', #44937, #1477, #41377, .T. ) ;
#29275 = VECTOR ( 'NONE', #38537, 1000.000000000000227 ) ;
#29276 = FACE_OUTER_BOUND ( 'NONE', #7047, .T. ) ;
#29277 = ORIENTED_EDGE ( 'NONE', *, *, #20451, .T. ) ;
#29278 = CARTESIAN_POINT ( 'NONE',  ( -27.06708303904391144, 0.000000000000000000, 7.395095371555332697 ) ) ;
#29279 = EDGE_CURVE ( 'NONE', #17736, #13096, #32571, .T. ) ;
#29280 = VECTOR ( 'NONE', #15575, 999.9999999999998863 ) ;
#29281 = ORIENTED_EDGE ( 'NONE', *, *, #28980, .F. ) ;
#29282 = CARTESIAN_POINT ( 'NONE',  ( -11.55387398669053312, -2.137015261443158565, 4.677054874402827522 ) ) ;
#29283 = EDGE_LOOP ( 'NONE', ( #33149, #16027, #23214, #914 ) ) ;
#29284 = VERTEX_POINT ( 'NONE', #36541 ) ;
#29285 = VERTEX_POINT ( 'NONE', #54407 ) ;
#29286 = EDGE_CURVE ( 'NONE', #41600, #50762, #14974, .T. ) ;
#29287 = LINE ( 'NONE', #19671, #17558 ) ;
#29288 = VECTOR ( 'NONE', #11418, 1000.000000000000227 ) ;
#29289 = DIRECTION ( 'NONE',  ( 0.000000000000000000, -1.000000000000000000, 0.000000000000000000 ) ) ;
#29290 = DIRECTION ( 'NONE',  ( -0.7660212471507179544, -0.6427876096865405842, -0.005961354470445141482 ) ) ;
#29291 = EDGE_CURVE ( 'NONE', #20189, #54113, #32831, .T. ) ;
#29292 = EDGE_CURVE ( 'NONE', #29930, #6164, #47584, .T. ) ;
#29293 = ADVANCED_FACE ( 'NONE', ( #42204 ), #7554, .F. ) ;
#29294 = VECTOR ( 'NONE', #13676, 1000.000000000000114 ) ;
#29295 = AXIS2_PLACEMENT_3D ( 'NONE', #13899, #7471, #5397 ) ;
#29296 = DIRECTION ( 'NONE',  ( 0.9999697198139515519, 0.000000000000000000, 0.007781995580013368816 ) ) ;
#29297 = EDGE_LOOP ( 'NONE', ( #43356, #33410, #49834, #17285 ) ) ;
#29298 = EDGE_CURVE ( 'NONE', #51007, #48125, #3310, .T. ) ;
#29299 = ADVANCED_BREP_SHAPE_REPRESENTATION ( '', ( #3992, #2610 ), #48882 ) ;
#29300 = ORIENTED_EDGE ( 'NONE', *, *, #34492, .T. ) ;
#29301 = VECTOR ( 'NONE', #3170, 999.9999999999998863 ) ;
#29302 = ORIENTED_EDGE ( 'NONE', *, *, #23423, .T. ) ;
#29303 = DIRECTION ( 'NONE',  ( 0.5449076811759707706, 0.6444004775717708799, -0.5364919789714476250 ) ) ;
#29304 = VECTOR ( 'NONE', #34716, 1000.000000000000227 ) ;
#29305 = PLANE ( 'NONE',  #4988 ) ;
#29306 = ORIENTED_EDGE ( 'NONE', *, *, #24418, .F. ) ;
#29307 = DIRECTION ( 'NONE',  ( -0.005002170337468016433, -0.7660444431189770143, 0.6427681459581293666 ) ) ;
#29308 = ORIENTED_EDGE ( 'NONE', *, *, #2735, .T. ) ;
#29309 = FACE_OUTER_BOUND ( 'NONE', #42238, .T. ) ;
#29310 = DIRECTION ( 'NONE',  ( -0.005961354470445682716, -0.6427876096865404731, 0.7660212471507180654 ) ) ;
#29311 = VERTEX_POINT ( 'NONE', #34515 ) ;
#29313 = VECTOR ( 'NONE', #7669, 1000.000000000000227 ) ;
#29312 = DIRECTION ( 'NONE',  ( 0.007781995580012663651, 0.000000000000000000, -0.9999697198139515519 ) ) ;
#29314 = EDGE_CURVE ( 'NONE', #41229, #26160, #12087, .T. ) ;
#29315 = EDGE_LOOP ( 'NONE', ( #21941, #46766, #17731, #32193 ) ) ;
#29316 = AXIS2_PLACEMENT_3D ( 'NONE', #31820, #4861, #1444 ) ;
#29317 = ADVANCED_FACE ( 'NONE', ( #8705 ), #43045, .F. ) ;
#29318 = CARTESIAN_POINT ( 'NONE',  ( -19.48141096923159665, 1.905425754524007198, 7.575691008948671978 ) ) ;
#29319 = DIRECTION ( 'NONE',  ( 0.007781995580012663651, -3.146120232559066537E-19, -0.9999697198139514409 ) ) ;
#29320 = ORIENTED_EDGE ( 'NONE', *, *, #19770, .T. ) ;
#29321 = LINE ( 'NONE', #21376, #44047 ) ;
#29322 = EDGE_CURVE ( 'NONE', #12293, #30283, #29731, .T. ) ;
#29323 = CARTESIAN_POINT ( 'NONE',  ( 2.072287782118878319, 0.000000000000000000, -2.950529333540147015 ) ) ;
#29324 = PLANE ( 'NONE',  #43676 ) ;
#29325 = ORIENTED_EDGE ( 'NONE', *, *, #3309, .T. ) ;
#29326 = VECTOR ( 'NONE', #43011, 1000.000000000000114 ) ;
#29328 = ORIENTED_EDGE ( 'NONE', *, *, #9788, .F. ) ;
#29327 = ADVANCED_FACE ( 'NONE', ( #34801 ), #3847, .F. ) ;
#29329 = DIRECTION ( 'NONE',  ( -2.683102249366423030E-17, 4.694855797473116505E-16, -1.000000000000000000 ) ) ;
#29330 = CARTESIAN_POINT ( 'NONE',  ( -9.808144436391993182, 0.000000000000000000, 10.77986332834118777 ) ) ;
#29331 = VECTOR ( 'NONE', #10013, 1000.000000000000000 ) ;
#29332 = LINE ( 'NONE', #50351, #5961 ) ;
#29333 = LINE ( 'NONE', #19705, #16733 ) ;
#29334 = EDGE_CURVE ( 'NONE', #24768, #36870, #20885, .T. ) ;
#29335 = LINE ( 'NONE', #16266, #22470 ) ;
#29336 = FACE_OUTER_BOUND ( 'NONE', #11285, .T. ) ;
#29337 = ORIENTED_EDGE ( 'NONE', *, *, #31451, .F. ) ;
#29338 = DIRECTION ( 'NONE',  ( -0.005002170337468016433, -0.7660444431189770143, 0.6427681459581293666 ) ) ;
#29339 = CARTESIAN_POINT ( 'NONE',  ( 3.520599301005862269, 0.000000000000000000, 0.7780620552096689790 ) ) ;
#29340 = ORIENTED_EDGE ( 'NONE', *, *, #47121, .F. ) ;
#29341 = VECTOR ( 'NONE', #22607, 1000.000000000000227 ) ;
#29342 = LINE ( 'NONE', #54904, #6880 ) ;
#29343 = VERTEX_POINT ( 'NONE', #43342 ) ;
#29344 = VECTOR ( 'NONE', #14035, 999.9999999999998863 ) ;
#29345 = AXIS2_PLACEMENT_3D ( 'NONE', #35177, #51625, #17256 ) ;
#29346 = FACE_OUTER_BOUND ( 'NONE', #22952, .T. ) ;
#29347 = CARTESIAN_POINT ( 'NONE',  ( -14.99525971934085788, 3.200641362704007786, 7.958786984757082017 ) ) ;
#29348 = LINE ( 'NONE', #22157, #21414 ) ;
#29349 = CARTESIAN_POINT ( 'NONE',  ( -26.21622229497770817, 17.48042152905857449, -4.621141326338904065 ) ) ;
#29350 = CARTESIAN_POINT ( 'NONE',  ( -67.57167971728060252, 1.999999999999992673, -7.559434449104583287 ) ) ;
#29351 = VERTEX_POINT ( 'NONE', #33964 ) ;
#29352 = AXIS2_PLACEMENT_3D ( 'NONE', #38016, #42282, #16416 ) ;
#29353 = AXIS2_PLACEMENT_3D ( 'NONE', #13903, #40024, #23290 ) ;
#29354 = EDGE_LOOP ( 'NONE', ( #11580, #54042, #5762, #52983 ) ) ;
#29355 = CARTESIAN_POINT ( 'NONE',  ( -15.99883398164889847, 2.229229656569006401, 2.825298075309216284 ) ) ;
#29356 = LINE ( 'NONE', #3516, #2274 ) ;
#29357 = CARTESIAN_POINT ( 'NONE',  ( -1.086233639165236964, 0.000000000000000000, -2.796443541562362078 ) ) ;
#29358 = LINE ( 'NONE', #50381, #35138 ) ;
#29359 = DIRECTION ( 'NONE',  ( 0.007781995580012663651, 0.000000000000000000, -0.9999697198139515519 ) ) ;
#29360 = CARTESIAN_POINT ( 'NONE',  ( -13.50126300573776739, 0.000000000000000000, 7.669993733430236382 ) ) ;
#29361 = ORIENTED_EDGE ( 'NONE', *, *, #2698, .F. ) ;
#29362 = LINE ( 'NONE', #21109, #14746 ) ;
#29363 = DIRECTION ( 'NONE',  ( -0.005002170337468016433, -0.7660444431189770143, 0.6427681459581293666 ) ) ;
#29364 = DIRECTION ( 'NONE',  ( 0.5364919789714477361, 0.6444004775717706579, 0.5449076811759711036 ) ) ;
#29365 = ORIENTED_EDGE ( 'NONE', *, *, #54492, .F. ) ;
#29366 = VECTOR ( 'NONE', #6088, 999.9999999999998863 ) ;
#29367 = DIRECTION ( 'NONE',  ( 0.9999697198139515519, 0.000000000000000000, 0.007781995580013368816 ) ) ;
#29368 = PLANE ( 'NONE',  #48570 ) ;
#29369 = VECTOR ( 'NONE', #10485, 999.9999999999998863 ) ;
#29370 = LINE ( 'NONE', #3794, #32937 ) ;
#29371 = EDGE_CURVE ( 'NONE', #16343, #54122, #39060, .T. ) ;
#29372 = EDGE_CURVE ( 'NONE', #30427, #34934, #38498, .T. ) ;
#29373 = EDGE_LOOP ( 'NONE', ( #17274, #19746, #35818, #53938 ) ) ;
#29374 = CARTESIAN_POINT ( 'NONE',  ( -14.01623497886155256, -0.1191753592594197858, 2.226008083469502630 ) ) ;
#29375 = VECTOR ( 'NONE', #32559, 999.9999999999998863 ) ;
#29376 = ORIENTED_EDGE ( 'NONE', *, *, #28912, .T. ) ;
#29377 = ADVANCED_FACE ( 'NONE', ( #29424 ), #20636, .F. ) ;
#29378 = ORIENTED_EDGE ( 'NONE', *, *, #10065, .F. ) ;
#29379 = VERTEX_POINT ( 'NONE', #47283 ) ;
#29380 = EDGE_LOOP ( 'NONE', ( #54916, #29094, #39931, #5421 ) ) ;
#29381 = VECTOR ( 'NONE', #7168, 1000.000000000000227 ) ;
#29382 = LINE ( 'NONE', #37327, #48362 ) ;
#29383 = ORIENTED_EDGE ( 'NONE', *, *, #19957, .F. ) ;
#29384 = CARTESIAN_POINT ( 'NONE',  ( -8.140418508869350589, -9.937499621474987777, 6.380388574284866721 ) ) ;
#29385 = VECTOR ( 'NONE', #29243, 999.9999999999998863 ) ;
#29386 = ORIENTED_EDGE ( 'NONE', *, *, #14772, .T. ) ;
#29387 = DIRECTION ( 'NONE',  ( 0.5449076811759707706, 0.6444004775717708799, -0.5364919789714476250 ) ) ;
#29388 = ORIENTED_EDGE ( 'NONE', *, *, #4519, .F. ) ;
#29389 = ORIENTED_EDGE ( 'NONE', *, *, #11525, .F. ) ;
#29390 = VECTOR ( 'NONE', #14077, 1000.000000000000227 ) ;
#29391 = VECTOR ( 'NONE', #37047, 999.9999999999998863 ) ;
#29392 = LINE ( 'NONE', #35080, #29326 ) ;
#29393 = LINE ( 'NONE', #37632, #368 ) ;
#29394 = DIRECTION ( 'NONE',  ( -0.6427681459581293666, -0.7660444431189770143, -0.005002170337467561935 ) ) ;
#29395 = DIRECTION ( 'NONE',  ( 0.005961354470445682716, -0.6427876096865404731, -0.7660212471507180654 ) ) ;
#29396 =( NAMED_UNIT ( * ) SI_UNIT ( $, .STERADIAN. ) SOLID_ANGLE_UNIT ( ) );
#29397 = ORIENTED_EDGE ( 'NONE', *, *, #6963, .T. ) ;
#29398 = ORIENTED_EDGE ( 'NONE', *, *, #25281, .F. ) ;
#29399 = DIRECTION ( 'NONE',  ( 0.000000000000000000, 0.000000000000000000, -1.000000000000000000 ) ) ;
#29400 = PLANE ( 'NONE',  #15778 ) ;
#29401 = EDGE_CURVE ( 'NONE', #37529, #25528, #16633, .T. ) ;
#29402 = DIRECTION ( 'NONE',  ( 0.007781995580012663651, 0.000000000000000000, -0.9999697198139515519 ) ) ;
#29403 = AXIS2_PLACEMENT_3D ( 'NONE', #49851, #2436, #19758 ) ;
#29404 = DIRECTION ( 'NONE',  ( 0.005002170337468016433, -0.7660444431189770143, -0.6427681459581293666 ) ) ;
#29405 = VECTOR ( 'NONE', #12556, 999.9999999999998863 ) ;
#29406 = EDGE_CURVE ( 'NONE', #30427, #2840, #24879, .T. ) ;
#29407 = FACE_OUTER_BOUND ( 'NONE', #36931, .T. ) ;
#29408 = LINE ( 'NONE', #43328, #10542 ) ;
#29409 = ORIENTED_EDGE ( 'NONE', *, *, #14316, .T. ) ;
#29410 = DIRECTION ( 'NONE',  ( -0.1139275668495183524, 0.9934890585767659488, 4.694855797473114533E-16 ) ) ;
#29411 = EDGE_CURVE ( 'NONE', #32655, #54876, #42488, .T. ) ;
#29412 = CARTESIAN_POINT ( 'NONE',  ( 5.523400311179926803, 0.000000000000000000, -2.340279943148938724 ) ) ;
#29413 = VECTOR ( 'NONE', #47264, 999.9999999999998863 ) ;
#29414 = ORIENTED_EDGE ( 'NONE', *, *, #45300, .F. ) ;
#29415 = CARTESIAN_POINT ( 'NONE',  ( -13.08486533123210194, 0.000000000000000000, 1.963927175729152541 ) ) ;
#29416 = FACE_OUTER_BOUND ( 'NONE', #23715, .T. ) ;
#29417 = DIRECTION ( 'NONE',  ( 0.6427681459581294776, -0.7660444431189769032, 0.005002170337467562802 ) ) ;
#29418 = EDGE_CURVE ( 'NONE', #53080, #51439, #3576, .T. ) ;
#29419 = PLANE ( 'NONE',  #35940 ) ;
#29420 = PLANE ( 'NONE',  #30465 ) ;
#29421 = EDGE_LOOP ( 'NONE', ( #18190, #10245, #5740, #34413 ) ) ;
#29422 = VERTEX_POINT ( 'NONE', #12402 ) ;
#29423 = VECTOR ( 'NONE', #24678, 999.9999999999998863 ) ;
#29424 = FACE_OUTER_BOUND ( 'NONE', #6053, .T. ) ;
#29425 = PLANE ( 'NONE',  #54896 ) ;
#29426 = CARTESIAN_POINT ( 'NONE',  ( -14.62478263637216180, 0.000000000000000000, 6.922586104262684614 ) ) ;
#29427 = VECTOR ( 'NONE', #46646, 1000.000000000000227 ) ;
#29428 = LINE ( 'NONE', #54687, #2843 ) ;
#29429 = PLANE ( 'NONE',  #49370 ) ;
#29430 = CARTESIAN_POINT ( 'NONE',  ( -7.547956548905578877, -7.259220043554206470, -0.2864909223855121034 ) ) ;
#29431 = PLANE ( 'NONE',  #13851 ) ;
#29432 = VECTOR ( 'NONE', #14367, 999.9999999999998863 ) ;
#29433 = DIRECTION ( 'NONE',  ( 0.9999697198139515519, 0.000000000000000000, 0.007781995580013368816 ) ) ;
#29434 = VECTOR ( 'NONE', #25117, 1000.000000000000000 ) ;
#29435 = DIRECTION ( 'NONE',  ( -0.005961354470445682716, -0.6427876096865404731, 0.7660212471507180654 ) ) ;
#29436 = DIRECTION ( 'NONE',  ( 0.005002170337468016433, -0.7660444431189770143, -0.6427681459581293666 ) ) ;
#29437 = EDGE_LOOP ( 'NONE', ( #53605, #7808, #44361, #47773 ) ) ;
#29438 = LINE ( 'NONE', #29744, #14126 ) ;
#29439 = EDGE_CURVE ( 'NONE', #17024, #9917, #47028, .T. ) ;
#29440 = EDGE_LOOP ( 'NONE', ( #19311, #27726, #46286, #52035 ) ) ;
#29441 = ORIENTED_EDGE ( 'NONE', *, *, #49205, .F. ) ;
#29442 = EDGE_CURVE ( 'NONE', #5827, #43300, #16939, .T. ) ;
#29443 = ADVANCED_FACE ( 'NONE', ( #52666 ), #23153, .F. ) ;
#29444 = VECTOR ( 'NONE', #4497, 1000.000000000000227 ) ;
#29445 = EDGE_LOOP ( 'NONE', ( #40708, #27629, #51576, #29818 ) ) ;
#29446 = ORIENTED_EDGE ( 'NONE', *, *, #51446, .F. ) ;
#29447 = EDGE_LOOP ( 'NONE', ( #39059, #10858, #55155, #15155 ) ) ;
#29448 = AXIS2_PLACEMENT_3D ( 'NONE', #43164, #51095, #4270 ) ;
#29449 = ORIENTED_EDGE ( 'NONE', *, *, #53243, .T. ) ;
#29450 = CARTESIAN_POINT ( 'NONE',  ( -18.12044783821180260, 0.000000000000000000, 4.140731527135287138 ) ) ;
#29451 = CARTESIAN_POINT ( 'NONE',  ( 4.530337070483293260, 0.000000000000000000, 2.076476591771610369 ) ) ;
#29452 = DIRECTION ( 'NONE',  ( 0.005961354470445682716, -0.6427876096865404731, -0.7660212471507180654 ) ) ;
#29453 = VECTOR ( 'NONE', #46028, 1000.000000000000000 ) ;
#29454 = ORIENTED_EDGE ( 'NONE', *, *, #8882, .F. ) ;
#29455 = DIRECTION ( 'NONE',  ( -0.5449076811759708816, 0.6444004775717707689, 0.5364919789714475140 ) ) ;
#29456 = VERTEX_POINT ( 'NONE', #35954 ) ;
#29457 = AXIS2_PLACEMENT_3D ( 'NONE', #5949, #23795, #45956 ) ;
#29458 = CARTESIAN_POINT ( 'NONE',  ( -65.54186449640286583, -11.22366718957837683, 5.111569279459596160 ) ) ;
#29459 = VERTEX_POINT ( 'NONE', #40481 ) ;
#29460 = EDGE_CURVE ( 'NONE', #24424, #52991, #724, .T. ) ;
#29461 = VECTOR ( 'NONE', #6613, 999.9999999999998863 ) ;
#29462 = VECTOR ( 'NONE', #17966, 1000.000000000000227 ) ;
#29463 = CARTESIAN_POINT ( 'NONE',  ( -67.34857948837910158, -8.812463414701275255, -4.340774506263340271 ) ) ;
#29464 = AXIS2_PLACEMENT_3D ( 'NONE', #38690, #51715, #12825 ) ;
#29465 = DIRECTION ( 'NONE',  ( 0.2426528472758541499, 0.7422098413412800966, 0.6246952433987894571 ) ) ;
#29466 = CARTESIAN_POINT ( 'NONE',  ( -68.63714112026566738, -10.92288908917430312, -7.487543234984625151 ) ) ;
#29467 = ORIENTED_EDGE ( 'NONE', *, *, #6950, .F. ) ;
#29468 = CARTESIAN_POINT ( 'NONE',  ( -10.27421835998572064, 0.000000000000000000, 10.96090226820206048 ) ) ;
#29469 = EDGE_LOOP ( 'NONE', ( #42388, #15425, #24142, #47926 ) ) ;
#29470 = VECTOR ( 'NONE', #13618, 1000.000000000000114 ) ;
#29471 = CARTESIAN_POINT ( 'NONE',  ( -13.92222681985565202, -5.536956232915666298, 2.112528921847934615 ) ) ;
#29472 = DIRECTION ( 'NONE',  ( 0.6427681459581294776, -0.7660444431189769032, 0.005002170337467562802 ) ) ;
#29473 = VECTOR ( 'NONE', #7490, 999.9999999999998863 ) ;
#29474 = DIRECTION ( 'NONE',  ( -0.005002170337468016433, -0.7660444431189770143, 0.6427681459581293666 ) ) ;
#29475 = AXIS2_PLACEMENT_3D ( 'NONE', #25167, #50702, #42473 ) ;
#29476 = LINE ( 'NONE', #46485, #35879 ) ;
#29477 = DIRECTION ( 'NONE',  ( 0.000000000000000000, -1.000000000000000000, 0.000000000000000000 ) ) ;
#29478 = LINE ( 'NONE', #25228, #38501 ) ;
#29479 = LINE ( 'NONE', #11851, #27504 ) ;
#29480 = CARTESIAN_POINT ( 'NONE',  ( -70.57579075201010710, -8.781267840485488918, 8.554889286408839055 ) ) ;
#29481 = EDGE_LOOP ( 'NONE', ( #17997, #5377, #6852, #29325 ) ) ;
#29482 = DIRECTION ( 'NONE',  ( 0.000000000000000000, -0.000000000000000000, -1.000000000000000000 ) ) ;
#29483 = ORIENTED_EDGE ( 'NONE', *, *, #10651, .T. ) ;
#29484 = CARTESIAN_POINT ( 'NONE',  ( -17.89735928879674631, 0.000000000000000000, 9.482442644690969757 ) ) ;
#29485 = CARTESIAN_POINT ( 'NONE',  ( -28.93137873341882127, 0.000000000000000000, 8.119251130998824451 ) ) ;
#29486 = LINE ( 'NONE', #11316, #11420 ) ;
#29487 = EDGE_CURVE ( 'NONE', #5703, #33009, #22853, .T. ) ;
#29488 = DIRECTION ( 'NONE',  ( 0.5364919789714477361, 0.6444004775717706579, 0.5449076811759711036 ) ) ;
#29489 = DIRECTION ( 'NONE',  ( 0.5364919789714477361, 0.6444004775717706579, 0.5449076811759711036 ) ) ;
#29490 = VECTOR ( 'NONE', #24267, 999.9999999999998863 ) ;
#29491 = CARTESIAN_POINT ( 'NONE',  ( -16.79925329029790149, 0.000000000000000000, 13.49544742625427496 ) ) ;
#29492 = SHAPE_DEFINITION_REPRESENTATION ( #5148, #51076 ) ;
#29493 = VECTOR ( 'NONE', #35681, 1000.000000000000114 ) ;
#29494 = ORIENTED_EDGE ( 'NONE', *, *, #21110, .F. ) ;
#29495 = CARTESIAN_POINT ( 'NONE',  ( -23.32622135384906770, 18.90220053346460460, -4.657437592157546824 ) ) ;
#29496 = CARTESIAN_POINT ( 'NONE',  ( -20.93015866917345846, 18.84219229648318716, 4.398249846736207225 ) ) ;
#29497 = DIRECTION ( 'NONE',  ( 0.9999697198139515519, 0.000000000000000000, 0.007781995580013368816 ) ) ;
#29498 = CARTESIAN_POINT ( 'NONE',  ( -13.83644591565411375, -1.003701604285657911, 2.223843262371220320 ) ) ;
#29499 = AXIS2_PLACEMENT_3D ( 'NONE', #42477, #32366, #45137 ) ;
#29500 = ADVANCED_FACE ( 'NONE', ( #17778 ), #47875, .F. ) ;
#29501 = LINE ( 'NONE', #2780, #9196 ) ;
#29502 = VECTOR ( 'NONE', #41813, 999.9999999999998863 ) ;
#29503 = DIRECTION ( 'NONE',  ( -0.6427681459581293666, -0.7660444431189770143, -0.005002170337467561935 ) ) ;
#29504 = ADVANCED_FACE ( 'NONE', ( #9820 ), #44431, .F. ) ;
#29505 = FACE_OUTER_BOUND ( 'NONE', #16238, .T. ) ;
#29506 = EDGE_CURVE ( 'NONE', #28751, #9630, #9230, .T. ) ;
#29507 = LINE ( 'NONE', #38581, #9312 ) ;
#29508 = ORIENTED_EDGE ( 'NONE', *, *, #46961, .F. ) ;
#29509 = DIRECTION ( 'NONE',  ( 0.5449076811759707706, 0.6444004775717708799, -0.5364919789714476250 ) ) ;
#29510 = VECTOR ( 'NONE', #9131, 999.9999999999998863 ) ;
#29511 = DIRECTION ( 'NONE',  ( 0.5364919789714477361, 0.6444004775717706579, 0.5449076811759711036 ) ) ;
#29512 = VECTOR ( 'NONE', #54310, 1000.000000000000000 ) ;
#29513 = VERTEX_POINT ( 'NONE', #39343 ) ;
#29514 = VECTOR ( 'NONE', #29265, 1000.000000000000227 ) ;
#29515 = ORIENTED_EDGE ( 'NONE', *, *, #3314, .T. ) ;
#29516 = CARTESIAN_POINT ( 'NONE',  ( -11.07315700445993478, 0.000000000000000000, 7.519563802190774027 ) ) ;
#29517 = ADVANCED_FACE ( 'NONE', ( #52119 ), #979, .F. ) ;
#29518 = AXIS2_PLACEMENT_3D ( 'NONE', #2161, #53851, #10969 ) ;
#29519 = ORIENTED_EDGE ( 'NONE', *, *, #27019, .F. ) ;
#29520 = AXIS2_PLACEMENT_3D ( 'NONE', #29615, #8020, #21049 ) ;
#29521 = EDGE_CURVE ( 'NONE', #25319, #41949, #13236, .T. ) ;
#29522 = LINE ( 'NONE', #33490, #1194 ) ;
#29523 = ADVANCED_FACE ( 'NONE', ( #52956 ), #14072, .F. ) ;
#29524 = VECTOR ( 'NONE', #4569, 1000.000000000000227 ) ;
#29525 = EDGE_LOOP ( 'NONE', ( #6038, #36565, #35910, #49198 ) ) ;
#29526 = VECTOR ( 'NONE', #36389, 1000.000000000000000 ) ;
#29527 = ORIENTED_EDGE ( 'NONE', *, *, #37514, .F. ) ;
#29528 = VERTEX_POINT ( 'NONE', #44175 ) ;
#29529 = PLANE ( 'NONE',  #40257 ) ;
#29530 = CARTESIAN_POINT ( 'NONE',  ( -16.40135577234480735, -0.1191753592594181482, 9.224755848276627646 ) ) ;
#29531 = CARTESIAN_POINT ( 'NONE',  ( -19.44046948079687454, 4.657758921906512306, 4.084663383300955353 ) ) ;
#29532 = EDGE_CURVE ( 'NONE', #11534, #28953, #22017, .T. ) ;
#29533 = EDGE_LOOP ( 'NONE', ( #39672, #23002, #31814, #49434 ) ) ;
#29534 = EDGE_LOOP ( 'NONE', ( #29259, #46247, #26802 ) ) ;
#29535 = VECTOR ( 'NONE', #13634, 1000.000000000000227 ) ;
#29536 = EDGE_CURVE ( 'NONE', #485, #53740, #18605, .T. ) ;
#29537 = PLANE ( 'NONE',  #4892 ) ;
#29538 = LINE ( 'NONE', #7367, #35459 ) ;
#29539 = VECTOR ( 'NONE', #33630, 999.9999999999998863 ) ;
#29540 = ORIENTED_EDGE ( 'NONE', *, *, #45979, .T. ) ;
#29541 = CARTESIAN_POINT ( 'NONE',  ( -15.24161218666607809, -4.889348428825665671, 2.645685084382324970 ) ) ;
#29542 = CARTESIAN_POINT ( 'NONE',  ( -10.19862816387108140, 0.000000000000000000, 1.247724401129331806 ) ) ;
#29543 = VERTEX_POINT ( 'NONE', #14362 ) ;
#29544 = VECTOR ( 'NONE', #7207, 999.9999999999998863 ) ;
#29545 = DIRECTION ( 'NONE',  ( 0.7660212471507180654, -0.6427876096865404731, 0.005961354470445141482 ) ) ;
#29546 = CARTESIAN_POINT ( 'NONE',  ( -12.29297599165088783, 0.000000000000000000, 5.832736553329440632 ) ) ;
#29547 = ORIENTED_EDGE ( 'NONE', *, *, #52184, .T. ) ;
#29548 = CARTESIAN_POINT ( 'NONE',  ( -14.67944861483846708, 2.876837460659008361, 2.292141912774824153 ) ) ;
#29549 = VECTOR ( 'NONE', #14810, 999.9999999999998863 ) ;
#29550 = CARTESIAN_POINT ( 'NONE',  ( -21.25413238913553471, -1.489407457353157049, 7.382129924272583743 ) ) ;
#29551 = AXIS2_PLACEMENT_3D ( 'NONE', #39536, #30157, #17360 ) ;
#29552 = VECTOR ( 'NONE', #41852, 1000.000000000000227 ) ;
#29553 = ORIENTED_EDGE ( 'NONE', *, *, #18873, .F. ) ;
#29554 = FACE_OUTER_BOUND ( 'NONE', #50269, .T. ) ;
#29555 = FACE_OUTER_BOUND ( 'NONE', #38561, .T. ) ;
#29556 = LINE ( 'NONE', #34624, #44792 ) ;
#29557 = DIRECTION ( 'NONE',  ( 0.007781995580012662783, 0.000000000000000000, -0.9999697198139514409 ) ) ;
#29558 = EDGE_LOOP ( 'NONE', ( #23777, #34513, #1034, #42676 ) ) ;
#29559 = VECTOR ( 'NONE', #55821, 999.9999999999998863 ) ;
#29560 = AXIS2_PLACEMENT_3D ( 'NONE', #11530, #28266, #49600 ) ;
#29561 = DIRECTION ( 'NONE',  ( -0.9999697198139514409, -0.000000000000000000, -0.007781995580013368816 ) ) ;
#29562 = DIRECTION ( 'NONE',  ( 0.6246952433987893460, 0.7422098413412802076, -0.2426528472758539279 ) ) ;
#29563 = LINE ( 'NONE', #51947, #38487 ) ;
#29564 = VECTOR ( 'NONE', #7219, 1000.000000000000227 ) ;
#29565 = EDGE_CURVE ( 'NONE', #6357, #34966, #48978, .T. ) ;
#29566 = LINE ( 'NONE', #42337, #13258 ) ;
#29567 = CARTESIAN_POINT ( 'NONE',  ( -13.49132319083263987, 0.000000000000000000, 6.392748864361969652 ) ) ;
#29568 = DIRECTION ( 'NONE',  ( -0.5364919789714478471, 0.6444004775717705469, -0.5449076811759709926 ) ) ;
#29569 = AXIS2_PLACEMENT_3D ( 'NONE', #36487, #2110, #54360 ) ;
#29570 = VECTOR ( 'NONE', #26547, 999.9999999999998863 ) ;
#29571 = CARTESIAN_POINT ( 'NONE',  ( -13.93871576664203182, 0.000000000000000000, 4.173274733047372287 ) ) ;
#29572 = VERTEX_POINT ( 'NONE', #432 ) ;
#29573 =( NAMED_UNIT ( * ) SI_UNIT ( $, .STERADIAN. ) SOLID_ANGLE_UNIT ( ) );
#29574 = CARTESIAN_POINT ( 'NONE',  ( -13.86960054602229953, 0.000000000000000000, 8.605797441356008548 ) ) ;
#29575 = ORIENTED_EDGE ( 'NONE', *, *, #20247, .T. ) ;
#29576 = FACE_OUTER_BOUND ( 'NONE', #11004, .T. ) ;
#29577 = DIRECTION ( 'NONE',  ( 0.000000000000000000, -0.000000000000000000, -1.000000000000000000 ) ) ;
#29578 = DIRECTION ( 'NONE',  ( 0.007781995580012663651, -3.146120232559066537E-19, -0.9999697198139514409 ) ) ;
#29579 = DIRECTION ( 'NONE',  ( 0.007781995580012663651, -3.146120232559066537E-19, -0.9999697198139514409 ) ) ;
#29580 = EDGE_CURVE ( 'NONE', #49166, #24915, #10077, .T. ) ;
#29581 = DIRECTION ( 'NONE',  ( -1.000000000000000000, 0.000000000000000000, 0.000000000000000000 ) ) ;
#29582 = VECTOR ( 'NONE', #51223, 999.9999999999998863 ) ;
#29583 = ORIENTED_EDGE ( 'NONE', *, *, #40021, .F. ) ;
#29584 = ORIENTED_EDGE ( 'NONE', *, *, #135, .F. ) ;
#29585 = DIRECTION ( 'NONE',  ( -0.5364919789714478471, 0.6444004775717705469, -0.5449076811759709926 ) ) ;
#29586 = CARTESIAN_POINT ( 'NONE',  ( -25.83906152351308450, 17.72030577168507648, -4.604772726025884388 ) ) ;
#29587 = ORIENTED_EDGE ( 'NONE', *, *, #34237, .F. ) ;
#29588 = VECTOR ( 'NONE', #30554, 1000.000000000000114 ) ;
#29589 = CARTESIAN_POINT ( 'NONE',  ( -14.51694170343292178, -0.1191753592594181482, 5.915432166028785410 ) ) ;
#29590 = ORIENTED_EDGE ( 'NONE', *, *, #2163, .T. ) ;
#29591 = EDGE_CURVE ( 'NONE', #23572, #36955, #43875, .T. ) ;
#29592 = LINE ( 'NONE', #37240, #5042 ) ;
#29593 = VECTOR ( 'NONE', #27829, 1000.000000000000227 ) ;
#29594 = ORIENTED_EDGE ( 'NONE', *, *, #45485, .F. ) ;
#29595 = CARTESIAN_POINT ( 'NONE',  ( -17.46532115785441519, 0.000000000000000000, 13.67492996699914265 ) ) ;
#29596 = EDGE_CURVE ( 'NONE', #55560, #2, #4989, .T. ) ;
#29597 = VECTOR ( 'NONE', #45968, 999.9999999999998863 ) ;
#29598 = VECTOR ( 'NONE', #12637, 999.9999999999998863 ) ;
#29599 = ORIENTED_EDGE ( 'NONE', *, *, #38878, .F. ) ;
#29600 = ORIENTED_EDGE ( 'NONE', *, *, #9461, .F. ) ;
#29601 = ORIENTED_EDGE ( 'NONE', *, *, #26172, .T. ) ;
#29602 = DIRECTION ( 'NONE',  ( 0.007781995580012663651, 0.000000000000000000, -0.9999697198139515519 ) ) ;
#29603 = PLANE ( 'NONE',  #39587 ) ;
#29604 = LINE ( 'NONE', #42629, #53855 ) ;
#29605 = AXIS2_PLACEMENT_3D ( 'NONE', #28265, #32802, #54964 ) ;
#29606 = EDGE_CURVE ( 'NONE', #41331, #34820, #48415, .T. ) ;
#29607 = AXIS2_PLACEMENT_3D ( 'NONE', #54965, #33637, #20863 ) ;
#29608 = CARTESIAN_POINT ( 'NONE',  ( -20.54049170961573267, 0.000000000000000000, 4.660556269540326646 ) ) ;
#29609 = VERTEX_POINT ( 'NONE', #19722 ) ;
#29610 = VECTOR ( 'NONE', #29016, 999.9999999999998863 ) ;
#29611 = ORIENTED_EDGE ( 'NONE', *, *, #11801, .F. ) ;
#29612 = ADVANCED_FACE ( 'NONE', ( #54607 ), #24517, .F. ) ;
#29613 = AXIS2_PLACEMENT_3D ( 'NONE', #19718, #20256, #19975 ) ;
#29614 = ORIENTED_EDGE ( 'NONE', *, *, #51878, .F. ) ;
#29615 = CARTESIAN_POINT ( 'NONE',  ( -11.67244013076689946, 0.000000000000000000, 11.50401908778467863 ) ) ;
#29616 = CARTESIAN_POINT ( 'NONE',  ( -22.40556560354864146, -0.1191753592594197858, 5.484709000965211523 ) ) ;
#29617 = EDGE_LOOP ( 'NONE', ( #45363, #56204, #19080, #21515 ) ) ;
#29618 = CARTESIAN_POINT ( 'NONE',  ( 2.072287782118878319, 0.000000000000000000, -2.950529333540147015 ) ) ;
#29619 = EDGE_LOOP ( 'NONE', ( #27728, #37934, #43221, #11906, #9321 ) ) ;
#29620 = DIRECTION ( 'NONE',  ( -0.5449076811759708816, 0.6444004775717707689, 0.5364919789714475140 ) ) ;
#29621 = CARTESIAN_POINT ( 'NONE',  ( 2.072287782118878319, 0.000000000000000000, -2.950529333540147015 ) ) ;
#29622 = ORIENTED_EDGE ( 'NONE', *, *, #34451, .F. ) ;
#29623 = PLANE ( 'NONE',  #44006 ) ;
#29624 = ORIENTED_EDGE ( 'NONE', *, *, #56114, .F. ) ;
#29625 = AXIS2_PLACEMENT_3D ( 'NONE', #47414, #51674, #21005 ) ;
#29626 = LINE ( 'NONE', #30161, #972 ) ;
#29627 = CARTESIAN_POINT ( 'NONE',  ( 1.086233639165236964, 0.000000000000000000, 2.796443541562362078 ) ) ;
#29628 = ORIENTED_EDGE ( 'NONE', *, *, #30079, .T. ) ;
#29629 = LINE ( 'NONE', #38706, #12325 ) ;
#29630 = PLANE ( 'NONE',  #301 ) ;
#29631 = DIRECTION ( 'NONE',  ( 0.9999697198139515519, 0.000000000000000000, 0.007781995580013368816 ) ) ;
#29632 = DIRECTION ( 'NONE',  ( -0.7660212471507179544, -0.6427876096865405842, -0.005961354470445141482 ) ) ;
#29633 = VECTOR ( 'NONE', #48248, 1000.000000000000000 ) ;
#29634 = ORIENTED_EDGE ( 'NONE', *, *, #32325, .T. ) ;
#29635 = ADVANCED_FACE ( 'NONE', ( #2094 ), #37298, .F. ) ;
#29636 = ORIENTED_EDGE ( 'NONE', *, *, #16339, .T. ) ;
#29637 = CARTESIAN_POINT ( 'NONE',  ( -17.22123223397174030, 0.000000000000000000, 8.010376142543925937 ) ) ;
#29638 = VECTOR ( 'NONE', #5473, 1000.000000000000227 ) ;
#29639 = LINE ( 'NONE', #46944, #26727 ) ;
#29640 = EDGE_CURVE ( 'NONE', #50295, #44275, #6657, .T. ) ;
#29641 = DIRECTION ( 'NONE',  ( -0.5449076811759708816, 0.6444004775717707689, 0.5364919789714475140 ) ) ;
#29642 = FACE_OUTER_BOUND ( 'NONE', #5996, .T. ) ;
#29643 = DIRECTION ( 'NONE',  ( -0.6427681459581293666, -0.7660444431189770143, -0.005002170337467561935 ) ) ;
#29644 = AXIS2_PLACEMENT_3D ( 'NONE', #3060, #16401, #8184 ) ;
#29645 = EDGE_CURVE ( 'NONE', #24756, #1435, #7216, .T. ) ;
#29646 = PLANE ( 'NONE',  #23150 ) ;
#29647 = ORIENTED_EDGE ( 'NONE', *, *, #26524, .F. ) ;
#29648 = EDGE_CURVE ( 'NONE', #40648, #42565, #2924, .T. ) ;
#29649 = CARTESIAN_POINT ( 'NONE',  ( -21.63461151687438999, 4.495856970884011261, 4.942108183378046249 ) ) ;
#29650 = LINE ( 'NONE', #3766, #14187 ) ;
#29651 = EDGE_LOOP ( 'NONE', ( #15439, #7704, #51645, #47074, #48447 ) ) ;
#29652 = DIRECTION ( 'NONE',  ( 0.9999697198139515519, 0.000000000000000000, 0.007781995580013368816 ) ) ;
#29653 = ORIENTED_EDGE ( 'NONE', *, *, #38954, .T. ) ;
#29654 = EDGE_CURVE ( 'NONE', #1287, #46991, #15440, .T. ) ;
#29655 = ADVANCED_FACE ( 'NONE', ( #36214 ), #27693, .F. ) ;
#29656 = EDGE_CURVE ( 'NONE', #12179, #28185, #27974, .T. ) ;
#29657 = FACE_OUTER_BOUND ( 'NONE', #19477, .T. ) ;
#29658 = DIRECTION ( 'NONE',  ( 0.9999697198139515519, 0.000000000000000000, 0.007781995580013368816 ) ) ;
#29659 = VECTOR ( 'NONE', #47336, 1000.000000000000227 ) ;
#29660 = CARTESIAN_POINT ( 'NONE',  ( -63.56784591066751489, 8.775889882925216767, 3.000000000000000000 ) ) ;
#29661 = FACE_OUTER_BOUND ( 'NONE', #30766, .T. ) ;
#29662 = AXIS2_PLACEMENT_3D ( 'NONE', #28959, #30366, #30901 ) ;
#29663 = CARTESIAN_POINT ( 'NONE',  ( -68.27148781930287669, 0.1328899438206843642, -4.676733487538881739 ) ) ;
#29664 = ORIENTED_EDGE ( 'NONE', *, *, #19165, .F. ) ;
#29665 = AXIS2_PLACEMENT_3D ( 'NONE', #29268, #3149, #45749 ) ;
#29666 = ORIENTED_EDGE ( 'NONE', *, *, #18011, .T. ) ;
#29667 = CARTESIAN_POINT ( 'NONE',  ( -9.949673132908477768, 0.000000000000000000, 3.265648189365135234 ) ) ;
#29668 = CARTESIAN_POINT ( 'NONE',  ( -10.47421230394850866, 0.000000000000000000, 10.95934586908605723 ) ) ;
#29669 = CARTESIAN_POINT ( 'NONE',  ( -12.52887840947635745, 0.000000000000000000, 2.137580008099788209 ) ) ;
#29670 = DIRECTION ( 'NONE',  ( 0.000000000000000000, -1.000000000000000000, 0.000000000000000000 ) ) ;
#29671 = DIRECTION ( 'NONE',  ( -0.005002170337468016433, -0.7660444431189770143, 0.6427681459581293666 ) ) ;
#29672 = EDGE_CURVE ( 'NONE', #16268, #46898, #32234, .T. ) ;
#29673 = DIRECTION ( 'NONE',  ( -0.005961354470445682716, -0.6427876096865404731, 0.7660212471507180654 ) ) ;
#29674 = VERTEX_POINT ( 'NONE', #11487 ) ;
#29675 = CARTESIAN_POINT ( 'NONE',  ( -17.39535969638698276, 0.000000000000000000, 4.685032414108041721 ) ) ;
#29676 = AXIS2_PLACEMENT_3D ( 'NONE', #1454, #47774, #30976 ) ;
#29677 = EDGE_CURVE ( 'NONE', #41065, #25334, #15197, .T. ) ;
#29678 = CARTESIAN_POINT ( 'NONE',  ( -18.16819014657557574, 0.000000000000000000, 10.27551562292821963 ) ) ;
#29679 = CARTESIAN_POINT ( 'NONE',  ( -17.73140113748535285, 0.000000000000000000, 13.85752530597602039 ) ) ;
#29680 = ORIENTED_EDGE ( 'NONE', *, *, #16450, .T. ) ;
#29681 = EDGE_CURVE ( 'NONE', #54483, #46200, #40751, .T. ) ;
#29682 = DIRECTION ( 'NONE',  ( 0.9999697198139515519, 0.000000000000000000, 0.007781995580013368816 ) ) ;
#29683 = DIRECTION ( 'NONE',  ( 0.9999697198139515519, 0.000000000000000000, 0.007781995580013368816 ) ) ;
#29684 = CARTESIAN_POINT ( 'NONE',  ( -16.33317936670417225, 0.000000000000000000, 13.31440848639340224 ) ) ;
#29685 = ORIENTED_EDGE ( 'NONE', *, *, #52157, .F. ) ;
#29686 = EDGE_CURVE ( 'NONE', #41830, #55275, #50072, .T. ) ;
#29687 = CARTESIAN_POINT ( 'NONE',  ( -17.74560456716937296, 0.000000000000000000, 3.774316574337878372 ) ) ;
#29688 = VECTOR ( 'NONE', #6141, 999.9999999999998863 ) ;
#29689 = ORIENTED_EDGE ( 'NONE', *, *, #27315, .T. ) ;
#29690 = ORIENTED_EDGE ( 'NONE', *, *, #26736, .T. ) ;
#29691 = VECTOR ( 'NONE', #51205, 999.9999999999998863 ) ;
#29692 = VERTEX_POINT ( 'NONE', #41574 ) ;
#29693 = ORIENTED_EDGE ( 'NONE', *, *, #718, .T. ) ;
#29694 = LINE ( 'NONE', #46987, #324 ) ;
#29695 = ORIENTED_EDGE ( 'NONE', *, *, #40018, .F. ) ;
#29696 = CARTESIAN_POINT ( 'NONE',  ( -12.80458192191714595, 0.000000000000000000, 11.86454056839041726 ) ) ;
#29697 = AXIS2_PLACEMENT_3D ( 'NONE', #2372, #28790, #36746 ) ;
#29698 = ORIENTED_EDGE ( 'NONE', *, *, #6218, .F. ) ;
#29699 = CARTESIAN_POINT ( 'NONE',  ( -21.06965149344186372, 20.49370688441071664, 4.356723378946029790 ) ) ;
#29700 = ORIENTED_EDGE ( 'NONE', *, *, #25780, .T. ) ;
#29701 = ORIENTED_EDGE ( 'NONE', *, *, #36719, .F. ) ;
#29702 = LINE ( 'NONE', #56087, #3002 ) ;
#29703 = LINE ( 'NONE', #25409, #43173 ) ;
#29704 = DIRECTION ( 'NONE',  ( -0.5449076811759708816, 0.6444004775717707689, 0.5364919789714475140 ) ) ;
#29705 = LINE ( 'NONE', #33389, #37788 ) ;
#29706 = EDGE_LOOP ( 'NONE', ( #31673, #53599, #54243, #24021 ) ) ;
#29707 = VERTEX_POINT ( 'NONE', #54348 ) ;
#29708 = DIRECTION ( 'NONE',  ( -0.000000000000000000, -1.000000000000000000, -0.000000000000000000 ) ) ;
#29709 = CARTESIAN_POINT ( 'NONE',  ( -26.13337879274045505, 0.000000000000000000, 6.833023547870798353 ) ) ;
#29710 = PRODUCT_DEFINITION_CONTEXT ( 'detailed design', #32927, 'design' ) ;
#29711 = LINE ( 'NONE', #25165, #20639 ) ;
#29712 = PLANE ( 'NONE',  #4184 ) ;
#29713 = CARTESIAN_POINT ( 'NONE',  ( -14.94916102560700821, 0.000000000000000000, 2.688082935172642962 ) ) ;
#29714 = DIRECTION ( 'NONE',  ( 0.007781995580012663651, -3.146120232559066537E-19, -0.9999697198139514409 ) ) ;
#29715 = EDGE_LOOP ( 'NONE', ( #23455, #22948, #17216, #4017 ) ) ;
#29716 = CARTESIAN_POINT ( 'NONE',  ( -13.13740128043607669, -0.1191753592594177180, 7.772828417621633790 ) ) ;
#29717 = LINE ( 'NONE', #53630, #15862 ) ;
#29718 = ORIENTED_EDGE ( 'NONE', *, *, #36324, .T. ) ;
#29719 = EDGE_CURVE ( 'NONE', #27017, #54363, #1817, .T. ) ;
#29720 = EDGE_CURVE ( 'NONE', #21115, #37239, #6385, .T. ) ;
#29721 = DIRECTION ( 'NONE',  ( 0.007781995580012663651, -3.146120232559066537E-19, -0.9999697198139514409 ) ) ;
#29722 = DIRECTION ( 'NONE',  ( 0.9999697198139515519, 0.000000000000000000, 0.007781995580013368816 ) ) ;
#29723 = FACE_OUTER_BOUND ( 'NONE', #52066, .T. ) ;
#29724 = FACE_OUTER_BOUND ( 'NONE', #20479, .T. ) ;
#29725 = ADVANCED_FACE ( 'NONE', ( #2657 ), #31935, .F. ) ;
#29726 = DIRECTION ( 'NONE',  ( -0.005002170337468016433, -0.7660444431189770143, 0.6427681459581293666 ) ) ;
#29727 = VECTOR ( 'NONE', #43047, 999.9999999999998863 ) ;
#29728 = VERTEX_POINT ( 'NONE', #45020 ) ;
#29729 =( BOUNDED_CURVE ( )  B_SPLINE_CURVE ( 3, ( #33512, #54506, #46020, #3115 ),
 .UNSPECIFIED., .F., .F. ) 
 B_SPLINE_CURVE_WITH_KNOTS ( ( 4, 4 ),
 ( 1.527237336719642125, 1.527316689203489508 ),
 .UNSPECIFIED. ) 
 CURVE ( )  GEOMETRIC_REPRESENTATION_ITEM ( )  RATIONAL_B_SPLINE_CURVE ( ( 1.000000000000000000, 0.9999999994752652999, 0.9999999994752652999, 1.000000000000000000 ) ) 
 REPRESENTATION_ITEM ( '' )  );
#29730 = ORIENTED_EDGE ( 'NONE', *, *, #28128, .T. ) ;
#29731 = LINE ( 'NONE', #46744, #48445 ) ;
#29732 = FACE_OUTER_BOUND ( 'NONE', #23841, .T. ) ;
#29733 = CARTESIAN_POINT ( 'NONE',  ( -26.26580391614848864, 17.49370688441070953, -4.622528711259356271 ) ) ;
#29734 = VECTOR ( 'NONE', #4607, 1000.000000000000227 ) ;
#29735 = DIRECTION ( 'NONE',  ( -0.9983709377222390602, -0.05705673239519638146, 0.000000000000000000 ) ) ;
#29736 = CARTESIAN_POINT ( 'NONE',  ( -15.64335043210865450, -1.489407457353158160, 2.910209779635662741 ) ) ;
#29737 = CARTESIAN_POINT ( 'NONE',  ( -16.81190032086591302, 0.000000000000000000, 3.212244750653343583 ) ) ;
#29738 = CARTESIAN_POINT ( 'NONE',  ( -10.27421835998572064, 0.000000000000000000, 10.96090226820206048 ) ) ;
#29739 = DIRECTION ( 'NONE',  ( 0.005961354470445682716, -0.6427876096865404731, -0.7660212471507180654 ) ) ;
#29740 = CARTESIAN_POINT ( 'NONE',  ( -68.90235146048875947, -9.595921133603816600, 8.251517284182451561 ) ) ;
#29741 = EDGE_CURVE ( 'NONE', #11699, #32747, #54088, .T. ) ;
#29742 = PLANE ( 'NONE',  #21065 ) ;
#29743 = EDGE_LOOP ( 'NONE', ( #55888, #26039, #10143, #29527 ) ) ;
#29744 = CARTESIAN_POINT ( 'NONE',  ( -11.77243710274829525, -0.1191753592594197858, 11.50324088822667612 ) ) ;
#29745 = ORIENTED_EDGE ( 'NONE', *, *, #276, .T. ) ;
#29746 = EDGE_CURVE ( 'NONE', #33250, #23017, #21433, .T. ) ;
#29747 = EDGE_LOOP ( 'NONE', ( #4173, #815, #18445, #48617 ) ) ;
#29748 = EDGE_CURVE ( 'NONE', #41698, #17269, #38737, .T. ) ;
#29749 = EDGE_LOOP ( 'NONE', ( #50046, #11065, #48106, #22609 ) ) ;
#29750 = ORIENTED_EDGE ( 'NONE', *, *, #49770, .F. ) ;
#29751 = ORIENTED_EDGE ( 'NONE', *, *, #18939, .T. ) ;
#29752 = ORIENTED_EDGE ( 'NONE', *, *, #19920, .F. ) ;
#29753 = CARTESIAN_POINT ( 'NONE',  ( -18.86354292863559579, 0.000000000000000000, 14.21804678658176080 ) ) ;
#29754 = DIRECTION ( 'NONE',  ( -0.5364919789714478471, 0.6444004775717705469, -0.5449076811759709926 ) ) ;
#29755 = DIRECTION ( 'NONE',  ( 0.9999697198139515519, 0.000000000000000000, 0.007781995580013368816 ) ) ;
#29756 = ORIENTED_EDGE ( 'NONE', *, *, #30217, .F. ) ;
#29757 = DIRECTION ( 'NONE',  ( 0.007781995580012663651, -3.146120232559066537E-19, -0.9999697198139514409 ) ) ;
#29758 = ORIENTED_EDGE ( 'NONE', *, *, #43366, .T. ) ;
#29759 = DIRECTION ( 'NONE',  ( 0.005002170337468016433, -0.7660444431189770143, -0.6427681459581293666 ) ) ;
#29760 = ORIENTED_EDGE ( 'NONE', *, *, #16499, .T. ) ;
#29761 = CARTESIAN_POINT ( 'NONE',  ( -17.93139508144814442, 0.000000000000000000, 13.85596890686001537 ) ) ;
#29762 = CARTESIAN_POINT ( 'NONE',  ( -15.35693653959682692, 0.000000000000000000, 7.286220383100434184 ) ) ;
#29763 = LINE ( 'NONE', #47059, #12336 ) ;
#29764 = VERTEX_POINT ( 'NONE', #42425 ) ;
#29765 = PLANE ( 'NONE',  #26474 ) ;
#29766 = EDGE_LOOP ( 'NONE', ( #55017, #12602, #47435, #18706 ) ) ;
#29767 = VECTOR ( 'NONE', #27524, 1000.000000000000114 ) ;
#29768 = PLANE ( 'NONE',  #40967 ) ;
#29769 = DIRECTION ( 'NONE',  ( 0.5364919789714477361, 0.6444004775717706579, 0.5449076811759711036 ) ) ;
#29770 = CARTESIAN_POINT ( 'NONE',  ( -25.83279121425626812, 17.74370688441070953, 4.604227610039242968 ) ) ;
#29771 = DIRECTION ( 'NONE',  ( -0.5449076811759708816, 0.6444004775717707689, 0.5364919789714475140 ) ) ;
#29772 = DIRECTION ( 'NONE',  ( -0.005002170337468016433, -0.7660444431189770143, 0.6427681459581293666 ) ) ;
#29773 = DIRECTION ( 'NONE',  ( 0.007781995580012663651, 0.000000000000000000, -0.9999697198139515519 ) ) ;
#29774 = CARTESIAN_POINT ( 'NONE',  ( -14.69598771881120136, 0.000000000000000000, 2.490047132166154586 ) ) ;
#29775 = CARTESIAN_POINT ( 'NONE',  ( -68.07298578174265913, -11.51392150788243818, -6.094799798532272384 ) ) ;
#29776 = ORIENTED_EDGE ( 'NONE', *, *, #26404, .F. ) ;
#29777 = CARTESIAN_POINT ( 'NONE',  ( 2.072287782118878319, 0.000000000000000000, -2.950529333540147015 ) ) ;
#29778 = VERTEX_POINT ( 'NONE', #29667 ) ;
#29779 = EDGE_CURVE ( 'NONE', #12044, #35264, #24809, .T. ) ;
#29780 = DIRECTION ( 'NONE',  ( -0.7660212471507179544, -0.6427876096865405842, -0.005961354470445141482 ) ) ;
#29781 = FACE_OUTER_BOUND ( 'NONE', #49841, .T. ) ;
#29782 = DIRECTION ( 'NONE',  ( 0.007781995580012663651, 0.000000000000000000, -0.9999697198139515519 ) ) ;
#29783 = CARTESIAN_POINT ( 'NONE',  ( -22.40634380310664397, 0.000000000000000000, 5.584705972946605534 ) ) ;
#29784 = FACE_OUTER_BOUND ( 'NONE', #3250, .T. ) ;
#29785 = EDGE_CURVE ( 'NONE', #39202, #2126, #47219, .T. ) ;
#29786 = EDGE_CURVE ( 'NONE', #23249, #17775, #16282, .T. ) ;
#29787 = CARTESIAN_POINT ( 'NONE',  ( -10.47421230394850866, 0.000000000000000000, 10.95934586908605723 ) ) ;
#29788 = ORIENTED_EDGE ( 'NONE', *, *, #6136, .F. ) ;
#29789 = DIRECTION ( 'NONE',  ( 0.5449076811759707706, 0.6444004775717708799, -0.5364919789714476250 ) ) ;
#29790 = DIRECTION ( 'NONE',  ( -0.005002170337468016433, -0.7660444431189770143, 0.6427681459581293666 ) ) ;
#29791 = CARTESIAN_POINT ( 'NONE',  ( -18.35337402512197968, 0.000000000000000000, 8.370897623149668121 ) ) ;
#29792 = CARTESIAN_POINT ( 'NONE',  ( -58.00000000000000711, 2.000000000000000000, -2.999999999999994227 ) ) ;
#29793 = FACE_OUTER_BOUND ( 'NONE', #8149, .T. ) ;
#29794 = FACE_OUTER_BOUND ( 'NONE', #41172, .T. ) ;
#29795 = CARTESIAN_POINT ( 'NONE',  ( 4.966775449259090536, -1.125037814383458512, -2.247047898273223598 ) ) ;
#29796 = ORIENTED_EDGE ( 'NONE', *, *, #29125, .T. ) ;
#29797 = LINE ( 'NONE', #42823, #36694 ) ;
#29798 = DIRECTION ( 'NONE',  ( 0.9999697198139515519, 0.000000000000000000, 0.007781995580013368816 ) ) ;
#29799 = ORIENTED_EDGE ( 'NONE', *, *, #49719, .F. ) ;
#29800 = ORIENTED_EDGE ( 'NONE', *, *, #46440, .F. ) ;
#29801 = CARTESIAN_POINT ( 'NONE',  ( -20.54126990917373519, -0.1191753592594197858, 4.760553241521720658 ) ) ;
#29802 = VECTOR ( 'NONE', #16471, 999.9999999999998863 ) ;
#29803 = ORIENTED_EDGE ( 'NONE', *, *, #48909, .F. ) ;
#29804 = ADVANCED_FACE ( 'NONE', ( #25644 ), #29065, .F. ) ;
#29805 = ORIENTED_EDGE ( 'NONE', *, *, #18806, .T. ) ;
#29806 = ORIENTED_EDGE ( 'NONE', *, *, #48541, .T. ) ;
#29807 = EDGE_LOOP ( 'NONE', ( #2713, #32988, #23870, #31994 ) ) ;
#29808 = ADVANCED_FACE ( 'NONE', ( #43284 ), #17141, .F. ) ;
#29809 = PLANE ( 'NONE',  #8514 ) ;
#29810 = CARTESIAN_POINT ( 'NONE',  ( -13.60688120397264278, -2.946525016555662457, 2.072686293655027434 ) ) ;
#29811 = ADVANCED_FACE ( 'NONE', ( #34452 ), #42677, .F. ) ;
#29812 = DIRECTION ( 'NONE',  ( 0.005961354470445682716, -0.6427876096865404731, -0.7660212471507180654 ) ) ;
#29813 = ORIENTED_EDGE ( 'NONE', *, *, #33053, .F. ) ;
#29814 = EDGE_CURVE ( 'NONE', #52782, #21764, #8625, .T. ) ;
#29815 = EDGE_LOOP ( 'NONE', ( #29103, #7890, #39609 ) ) ;
#29816 = DIRECTION ( 'NONE',  ( 0.005002170337468016433, -0.7660444431189770143, -0.6427681459581293666 ) ) ;
#29817 = LINE ( 'NONE', #42851, #2765 ) ;
#29818 = ORIENTED_EDGE ( 'NONE', *, *, #1134, .T. ) ;
#29819 = LINE ( 'NONE', #3957, #40017 ) ;
#29820 = CARTESIAN_POINT ( 'NONE',  ( -17.08865463677785357, 3.524445264749009876, 3.207297269127415085 ) ) ;
#29821 = ORIENTED_EDGE ( 'NONE', *, *, #7959, .F. ) ;
#29822 = LINE ( 'NONE', #55638, #7548 ) ;
#29823 = ORIENTED_EDGE ( 'NONE', *, *, #31173, .T. ) ;
#29824 = CARTESIAN_POINT ( 'NONE',  ( -20.02296364123857586, 1.376441525734817484, 6.094901730887621660 ) ) ;
#29825 = ADVANCED_FACE ( 'NONE', ( #16028 ), #33350, .F. ) ;
#29826 = DIRECTION ( 'NONE',  ( 0.5364919789714477361, 0.6444004775717706579, 0.5449076811759711036 ) ) ;
#29827 = ORIENTED_EDGE ( 'NONE', *, *, #23424, .F. ) ;
#29828 = LINE ( 'NONE', #30092, #26880 ) ;
#29829 = DIRECTION ( 'NONE',  ( 0.007781995580012662783, 0.000000000000000000, -0.9999697198139514409 ) ) ;
#29830 = CARTESIAN_POINT ( 'NONE',  ( -11.13365006456381856, 0.000000000000000000, 1.979111984108842037 ) ) ;
#29831 = CARTESIAN_POINT ( 'NONE',  ( -17.79123777228383929, 5.467268677019013978, 3.418218180132968076 ) ) ;
#29832 = EDGE_CURVE ( 'NONE', #51442, #30522, #42128, .T. ) ;
#29833 = ORIENTED_EDGE ( 'NONE', *, *, #3784, .F. ) ;
#29834 = VECTOR ( 'NONE', #49163, 1000.000000000000227 ) ;
#29835 = EDGE_CURVE ( 'NONE', #21379, #40714, #53194, .T. ) ;
#29836 = CARTESIAN_POINT ( 'NONE',  ( -69.59783862807636012, -0.6008070088998225255, -7.493102809087827332 ) ) ;
#29837 = DIRECTION ( 'NONE',  ( 0.007781995580012663651, 0.000000000000000000, -0.9999697198139515519 ) ) ;
#29838 = CARTESIAN_POINT ( 'NONE',  ( -10.67763532823858341, 0.000000000000000000, 3.090657005650145450 ) ) ;
#29839 = CARTESIAN_POINT ( 'NONE',  ( -25.20123094555300369, 0.000000000000000000, 6.470945668149052032 ) ) ;
#29840 = LINE ( 'NONE', #56221, #15830 ) ;
#29841 = EDGE_CURVE ( 'NONE', #33876, #7777, #4374, .T. ) ;
#29842 = PLANE ( 'NONE',  #19741 ) ;
#29843 = DIRECTION ( 'NONE',  ( -0.5449076811759708816, 0.6444004775717707689, 0.5364919789714475140 ) ) ;
#29844 = ORIENTED_EDGE ( 'NONE', *, *, #31402, .T. ) ;
#29845 = SURFACE_SIDE_STYLE ('',( #17316 ) ) ;
#29846 = CARTESIAN_POINT ( 'NONE',  ( -68.97544431584221059, -1.373506146286891395E-11, 7.657917462049396384 ) ) ;
#29847 = ORIENTED_EDGE ( 'NONE', *, *, #34373, .T. ) ;
#29848 = CARTESIAN_POINT ( 'NONE',  ( -2.579292853887890757, -4.639166217699263406, -2.216488638059722849 ) ) ;
#29849 = FACE_OUTER_BOUND ( 'NONE', #4841, .T. ) ;
#29850 = FACE_OUTER_BOUND ( 'NONE', #33026, .T. ) ;
#29851 = LINE ( 'NONE', #46893, #20565 ) ;
#29852 = LINE ( 'NONE', #38931, #19309 ) ;
#29853 = EDGE_CURVE ( 'NONE', #28798, #23596, #13702, .T. ) ;
#29854 = VERTEX_POINT ( 'NONE', #44099 ) ;
#29855 = VERTEX_POINT ( 'NONE', #4629 ) ;
#29856 = FACE_OUTER_BOUND ( 'NONE', #25680, .T. ) ;
#29857 = CARTESIAN_POINT ( 'NONE',  ( -1.300095020133916979, 4.816411402586080470, 3.723374632896542025 ) ) ;
#29858 = ORIENTED_EDGE ( 'NONE', *, *, #3718, .F. ) ;
#29859 = CARTESIAN_POINT ( 'NONE',  ( -25.20123094555300369, 0.000000000000000000, 6.470945668149052032 ) ) ;
#29860 = ORIENTED_EDGE ( 'NONE', *, *, #32641, .F. ) ;
#29861 = DIRECTION ( 'NONE',  ( 0.007781995580012662783, 0.000000000000000000, -0.9999697198139514409 ) ) ;
#29862 = ORIENTED_EDGE ( 'NONE', *, *, #19666, .T. ) ;
#29863 = CARTESIAN_POINT ( 'NONE',  ( -13.11728290589909918, -0.1191753592594190225, 5.187660494817285084 ) ) ;
#29864 = ORIENTED_EDGE ( 'NONE', *, *, #24813, .T. ) ;
#29865 = ORIENTED_EDGE ( 'NONE', *, *, #7894, .F. ) ;
#29866 = ORIENTED_EDGE ( 'NONE', *, *, #53458, .T. ) ;
#29867 = CARTESIAN_POINT ( 'NONE',  ( -9.388691517149283072, -0.1191753592594190225, 3.739348975930303354 ) ) ;
#29868 = DIRECTION ( 'NONE',  ( -0.6427681459581293666, -0.7660444431189770143, -0.005002170337467561935 ) ) ;
#29869 = PLANE ( 'NONE',  #32106 ) ;
#29870 = LINE ( 'NONE', #34670, #29405 ) ;
#29871 = VERTEX_POINT ( 'NONE', #52351 ) ;
#29872 = EDGE_CURVE ( 'NONE', #42922, #25139, #14300, .T. ) ;
#29873 = VERTEX_POINT ( 'NONE', #21942 ) ;
#29874 = ORIENTED_EDGE ( 'NONE', *, *, #48008, .F. ) ;
#29875 = DIRECTION ( 'NONE',  ( 0.000000000000000000, -0.000000000000000000, -1.000000000000000000 ) ) ;
#29876 = DIRECTION ( 'NONE',  ( 0.9999697198139515519, 0.000000000000000000, 0.007781995580013368816 ) ) ;
#29877 = EDGE_LOOP ( 'NONE', ( #34528, #22640, #2204, #33436 ) ) ;
#29878 = PLANE ( 'NONE',  #55664 ) ;
#29879 = EDGE_LOOP ( 'NONE', ( #25662, #27326, #31108, #35381 ) ) ;
#29880 = LINE ( 'NONE', #52006, #48714 ) ;
#29881 = DIRECTION ( 'NONE',  ( -0.9999697198139514409, -0.000000000000000000, -0.007781995580013368816 ) ) ;
#29882 = EDGE_CURVE ( 'NONE', #35428, #1353, #35567, .T. ) ;
#29883 = EDGE_LOOP ( 'NONE', ( #15604, #4248, #15882, #10679 ) ) ;
#29884 = DIRECTION ( 'NONE',  ( 0.9999697198139515519, 0.000000000000000000, 0.007781995580013368816 ) ) ;
#29885 = ORIENTED_EDGE ( 'NONE', *, *, #55256, .T. ) ;
#29886 = EDGE_CURVE ( 'NONE', #30608, #42734, #9165, .T. ) ;
#29887 = EDGE_CURVE ( 'NONE', #18842, #636, #35040, .T. ) ;
#29888 = DIRECTION ( 'NONE',  ( 0.000000000000000000, -1.000000000000000000, 0.000000000000000000 ) ) ;
#29889 = CARTESIAN_POINT ( 'NONE',  ( -20.16176772743538237, -0.1191753592594197858, 14.76194180572237968 ) ) ;
#29890 = VERTEX_POINT ( 'NONE', #915 ) ;
#29891 = LINE ( 'NONE', #35, #36859 ) ;
#29892 = LINE ( 'NONE', #26194, #22092 ) ;
#29893 = DIRECTION ( 'NONE',  ( -0.6427681459581293666, -0.7660444431189770143, -0.005002170337467561935 ) ) ;
#29894 = CARTESIAN_POINT ( 'NONE',  ( -18.67619601524082285, 0.000000000000000000, 3.936400510096834893 ) ) ;
#29895 = ADVANCED_FACE ( 'NONE', ( #48065 ), #662, .F. ) ;
#29896 = ORIENTED_EDGE ( 'NONE', *, *, #28853, .T. ) ;
#29897 = ADVANCED_FACE ( 'NONE', ( #34727 ), #64, .F. ) ;
#29898 = CARTESIAN_POINT ( 'NONE',  ( -70.00259797851279586, 0.1329035588801656675, 7.501778215771297553 ) ) ;
#29899 = LINE ( 'NONE', #34704, #6751 ) ;
#29900 = FACE_OUTER_BOUND ( 'NONE', #10885, .T. ) ;
#29901 = CARTESIAN_POINT ( 'NONE',  ( -20.18761153005478093, 0.000000000000000000, 5.232640590720539109 ) ) ;
#29902 = ADVANCED_FACE ( 'NONE', ( #40104 ), #18528, .F. ) ;
#29903 = LINE ( 'NONE', #3498, #31550 ) ;
#29904 = DIRECTION ( 'NONE',  ( -0.7660212471507179544, -0.6427876096865405842, -0.005961354470445141482 ) ) ;
#29905 = VERTEX_POINT ( 'NONE', #13449 ) ;
#29906 = DIRECTION ( 'NONE',  ( 0.5449076811759707706, 0.6444004775717708799, -0.5364919789714476250 ) ) ;
#29907 = CARTESIAN_POINT ( 'NONE',  ( -18.67619601524082285, 0.000000000000000000, 3.936400510096834893 ) ) ;
#29908 = CARTESIAN_POINT ( 'NONE',  ( 5.577510371788088506, -6.223674869166637258, 2.393421119419572474 ) ) ;
#29909 = ORIENTED_EDGE ( 'NONE', *, *, #54800, .F. ) ;
#29910 = DIRECTION ( 'NONE',  ( -0.005961354470445682716, -0.6427876096865404731, 0.7660212471507180654 ) ) ;
#29911 = FACE_OUTER_BOUND ( 'NONE', #40576, .T. ) ;
#29912 = VERTEX_POINT ( 'NONE', #4917 ) ;
#29913 = EDGE_CURVE ( 'NONE', #47218, #16890, #21685, .T. ) ;
#29914 = DIRECTION ( 'NONE',  ( 0.7660212471507180654, -0.6427876096865404731, 0.005961354470445141482 ) ) ;
#29915 = CARTESIAN_POINT ( 'NONE',  ( -18.78927038691023554, 0.000000000000000000, 4.674184678804012449 ) ) ;
#29916 = LINE ( 'NONE', #4072, #25064 ) ;
#29917 = CARTESIAN_POINT ( 'NONE',  ( -68.17482077307661825, 1.999999999996754596, 4.727715060444682926 ) ) ;
#29918 = ADVANCED_FACE ( 'NONE', ( #22239 ), #39574, .F. ) ;
#29919 = ORIENTED_EDGE ( 'NONE', *, *, #46289, .T. ) ;
#29920 = EDGE_LOOP ( 'NONE', ( #25868, #51460, #10279, #35823 ) ) ;
#29921 = CARTESIAN_POINT ( 'NONE',  ( -69.49476718086417293, -0.5994838070687775744, 7.360527835276493569 ) ) ;
#29922 = DIRECTION ( 'NONE',  ( -0.005961354470445682716, -0.6427876096865404731, 0.7660212471507180654 ) ) ;
#29923 = DIRECTION ( 'NONE',  ( 0.7660212471507180654, -0.6427876096865404731, 0.005961354470445141482 ) ) ;
#29924 = CARTESIAN_POINT ( 'NONE',  ( -13.17675323224890249, -1.327505506330657781, 1.957265181104025142 ) ) ;
#29925 = LINE ( 'NONE', #31325, #21059 ) ;
#29926 = DIRECTION ( 'NONE',  ( -0.7886751345948130876, 0.2113248654051844977, 0.5773502691896263972 ) ) ;
#29927 = ORIENTED_EDGE ( 'NONE', *, *, #45213, .T. ) ;
#29928 = CARTESIAN_POINT ( 'NONE',  ( -10.29984434460210352, -0.1134144341942118078, 0.7824357519659358440 ) ) ;
#29929 = FACE_OUTER_BOUND ( 'NONE', #14174, .T. ) ;
#29930 = VERTEX_POINT ( 'NONE', #52046 ) ;
#29931 = CARTESIAN_POINT ( 'NONE',  ( -69.48114687386605226, -8.789460189087408892, -7.500305896622815105 ) ) ;
#29932 = CARTESIAN_POINT ( 'NONE',  ( -16.99924723426068951, 0.000000000000000000, 13.49389102713827171 ) ) ;
#29933 = DIRECTION ( 'NONE',  ( -0.005002170337468016433, -0.7660444431189770143, 0.6427681459581293666 ) ) ;
#29934 = EDGE_LOOP ( 'NONE', ( #36466, #18720, #32797, #53351 ) ) ;
#29935 = DIRECTION ( 'NONE',  ( 0.007781995580012663651, -3.146120232559066537E-19, -0.9999697198139514409 ) ) ;
#29936 = EDGE_CURVE ( 'NONE', #44124, #42368, #35304, .T. ) ;
#29937 = ORIENTED_EDGE ( 'NONE', *, *, #13980, .F. ) ;
#29938 = VECTOR ( 'NONE', #18324, 1000.000000000000227 ) ;
#29939 = ORIENTED_EDGE ( 'NONE', *, *, #2429, .T. ) ;
#29940 = ORIENTED_EDGE ( 'NONE', *, *, #34068, .T. ) ;
#29941 = ORIENTED_EDGE ( 'NONE', *, *, #5711, .F. ) ;
#29942 = DIRECTION ( 'NONE',  ( -0.6427681459581293666, -0.7660444431189770143, -0.005002170337467561935 ) ) ;
#29944 = EDGE_CURVE ( 'NONE', #49575, #15364, #27060, .T. ) ;
#29943 = VERTEX_POINT ( 'NONE', #30499 ) ;
#29945 = CARTESIAN_POINT ( 'NONE',  ( -18.39746900504187010, 0.000000000000000000, 14.03700784672088808 ) ) ;
#29946 = EDGE_CURVE ( 'NONE', #34361, #37913, #17401, .T. ) ;
#29947 = ORIENTED_EDGE ( 'NONE', *, *, #31364, .T. ) ;
#29948 = LINE ( 'NONE', #3266, #54010 ) ;
#29949 = VERTEX_POINT ( 'NONE', #42289 ) ;
#29950 = CARTESIAN_POINT ( 'NONE',  ( -12.27728806973519404, 0.000000000000000000, 3.816872277745642084 ) ) ;
#29951 = EDGE_LOOP ( 'NONE', ( #26946, #24173, #16963, #19296 ) ) ;
#29952 = EDGE_CURVE ( 'NONE', #42667, #19558, #24962, .T. ) ;
#29953 = CARTESIAN_POINT ( 'NONE',  ( -14.20280369269832832, 0.000000000000000000, 12.40765738797303719 ) ) ;
#29954 = CARTESIAN_POINT ( 'NONE',  ( -26.13337879274045505, 0.000000000000000000, 6.833023547870798353 ) ) ;
#29955 = FACE_OUTER_BOUND ( 'NONE', #51012, .T. ) ;
#29956 = DIRECTION ( 'NONE',  ( -0.005961354470445682716, -0.6427876096865404731, 0.7660212471507180654 ) ) ;
#29957 = FILL_AREA_STYLE_COLOUR ( '', #48271 ) ;
#29958 = EDGE_LOOP ( 'NONE', ( #2366, #8517, #39644, #34357 ) ) ;
#29959 = VERTEX_POINT ( 'NONE', #20412 ) ;
#29960 = EDGE_CURVE ( 'NONE', #35804, #46919, #28945, .T. ) ;
#29961 = DIRECTION ( 'NONE',  ( 0.000000000000000000, -0.000000000000000000, -1.000000000000000000 ) ) ;
#29962 = PLANE ( 'NONE',  #28464 ) ;
#29963 = EDGE_CURVE ( 'NONE', #48365, #28099, #29202, .T. ) ;
#29964 = CARTESIAN_POINT ( 'NONE',  ( -27.06552663992790997, 0.000000000000000000, 7.195101427592543786 ) ) ;
#29965 = CARTESIAN_POINT ( 'NONE',  ( -24.27063949748155380, 0.000000000000000000, 6.308861732390097288 ) ) ;
#29966 = EDGE_CURVE ( 'NONE', #17816, #25674, #55327, .T. ) ;
#29967 = LINE ( 'NONE', #47270, #14972 ) ;
#29968 = PLANE ( 'NONE',  #13254 ) ;
#29969 = ORIENTED_EDGE ( 'NONE', *, *, #19652, .F. ) ;
#29970 = CARTESIAN_POINT ( 'NONE',  ( -21.47263955680318404, 0.000000000000000000, 5.022634149262071190 ) ) ;
#29971 = CARTESIAN_POINT ( 'NONE',  ( -15.91660050096674262, -0.1191753592594193972, 6.643203837240283960 ) ) ;
#29972 = ORIENTED_EDGE ( 'NONE', *, *, #22094, .F. ) ;
#29973 = ADVANCED_FACE ( 'NONE', ( #33744 ), #16422, .F. ) ;
#29974 = CARTESIAN_POINT ( 'NONE',  ( -16.75372128362536728, 0.000000000000000000, 7.644682351054170155 ) ) ;
#29975 = LINE ( 'NONE', #54079, #14241 ) ;
#29976 = DIRECTION ( 'NONE',  ( 0.5364919789714477361, 0.6444004775717706579, 0.5449076811759711036 ) ) ;
#29977 = CARTESIAN_POINT ( 'NONE',  ( 2.072287782118878319, 0.000000000000000000, -2.950529333540147015 ) ) ;
#29978 = AXIS2_PLACEMENT_3D ( 'NONE', #43515, #35028, #16626 ) ;
#29979 = VERTEX_POINT ( 'NONE', #33482 ) ;
#29980 = ORIENTED_EDGE ( 'NONE', *, *, #32454, .T. ) ;
#29981 = CARTESIAN_POINT ( 'NONE',  ( -14.00280974873554030, 0.000000000000000000, 12.40921378708904044 ) ) ;
#29982 = CARTESIAN_POINT ( 'NONE',  ( -15.96710241509184058, -0.1191753592594218814, 13.13259134697452879 ) ) ;
#29983 = CARTESIAN_POINT ( 'NONE',  ( 2.072287782118878319, 0.000000000000000000, -2.950529333540147015 ) ) ;
#29984 = PLANE ( 'NONE',  #7400 ) ;
#29985 = CARTESIAN_POINT ( 'NONE',  ( -10.27421835998572064, 0.000000000000000000, 10.96090226820206048 ) ) ;
#29986 = LINE ( 'NONE', #33676, #26460 ) ;
#29987 = PLANE ( 'NONE',  #8423 ) ;
#29988 = ORIENTED_EDGE ( 'NONE', *, *, #19434, .T. ) ;
#29989 = LINE ( 'NONE', #7874, #53173 ) ;
#29990 = DIRECTION ( 'NONE',  ( 0.007781995580012663651, -3.146120232559066537E-19, -0.9999697198139514409 ) ) ;
#29991 = CARTESIAN_POINT ( 'NONE',  ( 2.072287782118878319, 0.000000000000000000, -2.950529333540147015 ) ) ;
#29992 = ORIENTED_EDGE ( 'NONE', *, *, #42603, .F. ) ;
#29993 = PLANE ( 'NONE',  #4152 ) ;
#29994 = ADVANCED_FACE ( 'NONE', ( #49940 ), #41980, .F. ) ;
#29995 = B_SPLINE_CURVE_WITH_KNOTS ( 'NONE', 3,
 ( #2904, #5884, #33583, #20234, #37870, #55174, #23209, #11728, #36007, #16264, #36261, #54892, #16004, #46347, #50893, #31722, #11994, #53316, #49025, #53562, #10125, #27444 ),
 .UNSPECIFIED., .F., .F.,
 ( 4, 2, 2, 2, 2, 2, 2, 2, 2, 2, 4 ),
 ( -5.999998108584347237E-08, 0.0005071597037827979635, 0.001014379407546681881, 0.002028818815074472700, 0.003043258222602263953, 0.004057697630130054772, 0.006086576445185653758, 0.008115455260241252744, 0.01014433407529685346, 0.01217321289035245419, 0.01623097052046365216 ),
 .UNSPECIFIED. ) ;
#29996 = VERTEX_POINT ( 'NONE', #2535 ) ;
#29997 = VECTOR ( 'NONE', #53411, 999.9999999999998863 ) ;
#29998 = EDGE_CURVE ( 'NONE', #23767, #38400, #19855, .T. ) ;
#29999 = ORIENTED_EDGE ( 'NONE', *, *, #48608, .F. ) ;
#30000 = ORIENTED_EDGE ( 'NONE', *, *, #38292, .F. ) ;
#30001 = ORIENTED_EDGE ( 'NONE', *, *, #8388, .F. ) ;
#30002 = ORIENTED_EDGE ( 'NONE', *, *, #12885, .T. ) ;
#30003 = ORIENTED_EDGE ( 'NONE', *, *, #15474, .F. ) ;
#30004 = CARTESIAN_POINT ( 'NONE',  ( -18.09269438770527216, 0.2864062442990030766, 3.700610803468898258 ) ) ;
#30005 = DIRECTION ( 'NONE',  ( 0.6246952433987893460, 0.7422098413412802076, -0.2426528472758539279 ) ) ;
#30006 = FACE_OUTER_BOUND ( 'NONE', #16513, .T. ) ;
#30007 = ADVANCED_FACE ( 'NONE', ( #11628 ), #20112, .F. ) ;
#30008 = EDGE_CURVE ( 'NONE', #34747, #53648, #37446, .T. ) ;
#30009 = EDGE_CURVE ( 'NONE', #25732, #44724, #45406, .T. ) ;
#30010 = AXIS2_PLACEMENT_3D ( 'NONE', #41483, #11373, #54508 ) ;
#30011 = ORIENTED_EDGE ( 'NONE', *, *, #47737, .T. ) ;
#30012 = PLANE ( 'NONE',  #31318 ) ;
#30013 = ORIENTED_EDGE ( 'NONE', *, *, #26007, .T. ) ;
#30014 = DIRECTION ( 'NONE',  ( -0.005961354470445682716, -0.6427876096865404731, 0.7660212471507180654 ) ) ;
#30015 = EDGE_CURVE ( 'NONE', #11380, #2600, #11042, .T. ) ;
#30016 = EDGE_LOOP ( 'NONE', ( #48681, #48582, #53322, #31659 ) ) ;
#30017 = VECTOR ( 'NONE', #43945, 999.9999999999998863 ) ;
#30018 = FACE_OUTER_BOUND ( 'NONE', #53478, .T. ) ;
#30019 = PLANE ( 'NONE',  #36449 ) ;
#30020 = CARTESIAN_POINT ( 'NONE',  ( -29.86197018149027116, 0.000000000000000000, 8.281335066757780083 ) ) ;
#30021 = ORIENTED_EDGE ( 'NONE', *, *, #23935, .T. ) ;
#30022 = CARTESIAN_POINT ( 'NONE',  ( -19.18564475023670113, -3.432230869623159819, 9.767163286593927296 ) ) ;
#30023 = ORIENTED_EDGE ( 'NONE', *, *, #29171, .T. ) ;
#30024 = LINE ( 'NONE', #47334, #10134 ) ;
#30025 = CARTESIAN_POINT ( 'NONE',  ( -9.043391767268570192, 0.000000000000000000, 6.227357638963272102 ) ) ;
#30026 = EDGE_CURVE ( 'NONE', #55375, #27710, #15871, .T. ) ;
#30027 = EDGE_CURVE ( 'NONE', #54422, #16523, #23828, .T. ) ;
#30028 = DIRECTION ( 'NONE',  ( -0.6427681459581293666, -0.7660444431189770143, -0.005002170337467561935 ) ) ;
#30029 = CARTESIAN_POINT ( 'NONE',  ( -18.26565146671972073, -0.1191753592594149563, 9.948911607720113182 ) ) ;
#30030 = DIRECTION ( 'NONE',  ( 0.5449076811759707706, 0.6444004775717708799, -0.5364919789714476250 ) ) ;
#30031 = CARTESIAN_POINT ( 'NONE',  ( -26.13337879274045505, 0.000000000000000000, 6.833023547870798353 ) ) ;
#30032 = EDGE_CURVE ( 'NONE', #50886, #44511, #50528, .T. ) ;
#30033 = CARTESIAN_POINT ( 'NONE',  ( -14.90901332651993805, 0.9340140483890027046, 2.443298881491017038 ) ) ;
#30034 = DIRECTION ( 'NONE',  ( 0.005002170337468016433, -0.7660444431189770143, -0.6427681459581293666 ) ) ;
#30035 = ORIENTED_EDGE ( 'NONE', *, *, #7778, .T. ) ;
#30036 = CARTESIAN_POINT ( 'NONE',  ( -56.19068569781688893, 6.778861748851165103, -2.073212483771301073 ) ) ;
#30037 = ORIENTED_EDGE ( 'NONE', *, *, #45168, .F. ) ;
#30038 = VECTOR ( 'NONE', #49688, 999.9999999999998863 ) ;
#30039 = EDGE_CURVE ( 'NONE', #12427, #4219, #50786, .T. ) ;
#30040 = VECTOR ( 'NONE', #23527, 1000.000000000000114 ) ;
#30041 = CARTESIAN_POINT ( 'NONE',  ( -20.72814514249575168, 20.40220053346460460, -4.343046601173932153 ) ) ;
#30042 = DIRECTION ( 'NONE',  ( -0.9999697198139514409, -0.000000000000000000, -0.007781995580013368816 ) ) ;
#30043 = LINE ( 'NONE', #191, #23605 ) ;
#30044 = CARTESIAN_POINT ( 'NONE',  ( -13.10486132850893348, -4.565544526780663581, 1.826029526484286958 ) ) ;
#30045 = LINE ( 'NONE', #33728, #21363 ) ;
#30046 = ADVANCED_FACE ( 'NONE', ( #2248 ), #32634, .F. ) ;
#30047 = DIRECTION ( 'NONE',  ( 0.9999697198139515519, 0.000000000000000000, 0.007781995580013368816 ) ) ;
#30048 = PLANE ( 'NONE',  #7569 ) ;
#30049 = SHAPE_DEFINITION_REPRESENTATION ( #53650, #53575 ) ;
#30050 = EDGE_LOOP ( 'NONE', ( #38435, #45293, #42572, #13488 ) ) ;
#30051 = CARTESIAN_POINT ( 'NONE',  ( -12.20289707257236422, 23.88087912856912354, 3.602352073755655137 ) ) ;
#30052 = DIRECTION ( 'NONE',  ( 0.007781995580012663651, -3.146120232559066537E-19, -0.9999697198139514409 ) ) ;
#30053 = CARTESIAN_POINT ( 'NONE',  ( -26.13415699229845757, -0.1191753592594197858, 6.933020519852192365 ) ) ;
#30054 = CARTESIAN_POINT ( 'NONE',  ( -12.67560930558469323, -0.1191753592594190225, 8.142010695456853853 ) ) ;
#30055 = DIRECTION ( 'NONE',  ( -0.005002170337468016433, -0.7660444431189770143, 0.6427681459581293666 ) ) ;
#30056 = DIRECTION ( 'NONE',  ( 0.000000000000000000, -0.000000000000000000, -1.000000000000000000 ) ) ;
#30057 = CARTESIAN_POINT ( 'NONE',  ( -17.74404816805336793, 0.000000000000000000, 3.574322630375089460 ) ) ;
#30058 = EDGE_LOOP ( 'NONE', ( #26423, #41990, #29306, #30973 ) ) ;
#30059 = VECTOR ( 'NONE', #39799, 1000.000000000000227 ) ;
#30060 = DIRECTION ( 'NONE',  ( 0.007781995580012662783, 0.000000000000000000, -0.9999697198139514409 ) ) ;
#30061 = LINE ( 'NONE', #33220, #8887 ) ;
#30062 = VERTEX_POINT ( 'NONE', #50225 ) ;
#30063 = ORIENTED_EDGE ( 'NONE', *, *, #54176, .T. ) ;
#30064 = CARTESIAN_POINT ( 'NONE',  ( 2.072287782118878319, 0.000000000000000000, -2.950529333540147015 ) ) ;
#30065 = ORIENTED_EDGE ( 'NONE', *, *, #19743, .T. ) ;
#30066 = ORIENTED_EDGE ( 'NONE', *, *, #8575, .T. ) ;
#30067 = EDGE_LOOP ( 'NONE', ( #35743, #12124, #39268, #199 ) ) ;
#30068 = ORIENTED_EDGE ( 'NONE', *, *, #22087, .T. ) ;
#30069 = CARTESIAN_POINT ( 'NONE',  ( -18.40804000358828318, 2.876837460659008361, 3.740453431661805883 ) ) ;
#30070 = ORIENTED_EDGE ( 'NONE', *, *, #12194, .T. ) ;
#30071 = PLANE ( 'NONE',  #2432 ) ;
#30072 = CARTESIAN_POINT ( 'NONE',  ( -11.23199219178955310, -0.1134144341942142642, 1.144513631687679611 ) ) ;
#30073 = EDGE_CURVE ( 'NONE', #8011, #56197, #45989, .T. ) ;
#30074 = VECTOR ( 'NONE', #24587, 1000.000000000000227 ) ;
#30075 = AXIS2_PLACEMENT_3D ( 'NONE', #13876, #1380, #1919 ) ;
#30076 = ORIENTED_EDGE ( 'NONE', *, *, #21885, .T. ) ;
#30077 = ORIENTED_EDGE ( 'NONE', *, *, #14504, .T. ) ;
#30078 = ADVANCED_FACE ( 'NONE', ( #34589 ), #17559, .F. ) ;
#30079 = EDGE_CURVE ( 'NONE', #53603, #24506, #13323, .T. ) ;
#30080 = AXIS2_PLACEMENT_3D ( 'NONE', #51485, #8896, #13428 ) ;
#30081 = CARTESIAN_POINT ( 'NONE',  ( -65.59269431991148736, -5.464378949326944241E-14, -0.6466721865751011711 ) ) ;
#30082 = ORIENTED_EDGE ( 'NONE', *, *, #23515, .T. ) ;
#30083 = CARTESIAN_POINT ( 'NONE',  ( -19.11062313909426535, 4.819660872929013351, 3.951374342667357542 ) ) ;
#30084 = DIRECTION ( 'NONE',  ( -0.9999697198139514409, -0.000000000000000000, -0.007781995580013368816 ) ) ;
#30085 = ORIENTED_EDGE ( 'NONE', *, *, #8837, .F. ) ;
#30086 = DIRECTION ( 'NONE',  ( -0.005002170337468016433, -0.7660444431189770143, 0.6427681459581293666 ) ) ;
#30087 = ORIENTED_EDGE ( 'NONE', *, *, #33800, .F. ) ;
#30088 = CARTESIAN_POINT ( 'NONE',  ( -16.53317331066696383, 0.000000000000000000, 13.31285208727739899 ) ) ;
#30089 = VECTOR ( 'NONE', #42392, 1000.000000000000227 ) ;
#30090 = CARTESIAN_POINT ( 'NONE',  ( -11.63564965697357501, 0.000000000000000000, 6.776522214691770074 ) ) ;
#30091 = ORIENTED_EDGE ( 'NONE', *, *, #36245, .T. ) ;
#30092 = CARTESIAN_POINT ( 'NONE',  ( -13.08760808424579736, 3.200641362704010451, 1.663485951785882877 ) ) ;
#30093 = DIRECTION ( 'NONE',  ( 0.9999697198139515519, 0.000000000000000000, 0.007781995580013368816 ) ) ;
#30094 = PLANE ( 'NONE',  #41177 ) ;
#30095 = DIRECTION ( 'NONE',  ( -0.5364919789714478471, 0.6444004775717705469, -0.5449076811759709926 ) ) ;
#30096 = VERTEX_POINT ( 'NONE', #51636 ) ;
#30097 = DIRECTION ( 'NONE',  ( 0.5364919789714477361, 0.6444004775717706579, 0.5449076811759711036 ) ) ;
#30098 = LINE ( 'NONE', #8524, #39600 ) ;
#30099 = CARTESIAN_POINT ( 'NONE',  ( -21.47419595591918906, 0.000000000000000000, 5.222628093224860102 ) ) ;
#30100 = CARTESIAN_POINT ( 'NONE',  ( 2.072287782118878319, 0.000000000000000000, -2.950529333540147015 ) ) ;
#30101 = DIRECTION ( 'NONE',  ( 0.5364919789714477361, 0.6444004775717706579, 0.5449076811759711036 ) ) ;
#30102 = ADVANCED_FACE ( 'NONE', ( #46831 ), #34048, .F. ) ;
#30103 = DIRECTION ( 'NONE',  ( 0.5364919789714477361, 0.6444004775717706579, 0.5449076811759711036 ) ) ;
#30104 = CARTESIAN_POINT ( 'NONE',  ( -19.79127492296584734, -1.786397712959882034, 6.691370479880283106 ) ) ;
#30105 = DIRECTION ( 'NONE',  ( 0.007781995580012663651, 0.000000000000000000, -0.9999697198139515519 ) ) ;
#30106 = FACE_OUTER_BOUND ( 'NONE', #50437, .T. ) ;
#30107 = ORIENTED_EDGE ( 'NONE', *, *, #39078, .T. ) ;
#30109 = EDGE_CURVE ( 'NONE', #14557, #30246, #43406, .T. ) ;
#30108 =( LENGTH_UNIT ( ) NAMED_UNIT ( * ) SI_UNIT ( .MILLI., .METRE. ) );
#30110 = PLANE ( 'NONE',  #52281 ) ;
#30111 = VERTEX_POINT ( 'NONE', #12481 ) ;
#30112 = DIRECTION ( 'NONE',  ( 0.7660212471507180654, -0.6427876096865404731, 0.005961354470445141482 ) ) ;
#30113 = DIRECTION ( 'NONE',  ( -0.9999697198139514409, -0.000000000000000000, -0.007781995580013368816 ) ) ;
#30114 = VECTOR ( 'NONE', #16720, 999.9999999999998863 ) ;
#30115 = VECTOR ( 'NONE', #17113, 999.9999999999998863 ) ;
#30116 = ADVANCED_FACE ( 'NONE', ( #7940 ), #47670, .F. ) ;
#30117 = CARTESIAN_POINT ( 'NONE',  ( -64.10539783498545319, 7.375519243179410545, 5.000000000000000000 ) ) ;
#30118 = DIRECTION ( 'NONE',  ( 0.6427681459581294776, -0.7660444431189769032, 0.005002170337467562802 ) ) ;
#30119 = DIRECTION ( 'NONE',  ( -0.5449076811759708816, 0.6444004775717707689, 0.5364919789714475140 ) ) ;
#30120 = ORIENTED_EDGE ( 'NONE', *, *, #14271, .F. ) ;
#30121 = VECTOR ( 'NONE', #5957, 1000.000000000000227 ) ;
#30122 = ORIENTED_EDGE ( 'NONE', *, *, #41986, .F. ) ;
#30123 = PLANE ( 'NONE',  #46754 ) ;
#30124 = PLANE ( 'NONE',  #50358 ) ;
#30125 = ORIENTED_EDGE ( 'NONE', *, *, #13831, .F. ) ;
#30126 = CARTESIAN_POINT ( 'NONE',  ( 2.072287782118878319, 0.000000000000000000, -2.950529333540147015 ) ) ;
#30127 = EDGE_LOOP ( 'NONE', ( #315, #33632, #34525, #6077 ) ) ;
#30128 = DIRECTION ( 'NONE',  ( 0.005961354470445682716, -0.6427876096865404731, -0.7660212471507180654 ) ) ;
#30129 = VECTOR ( 'NONE', #33174, 999.9999999999998863 ) ;
#30130 = VERTEX_POINT ( 'NONE', #3647 ) ;
#30131 = DIRECTION ( 'NONE',  ( 0.007781995580012663651, -3.146120232559066537E-19, -0.9999697198139514409 ) ) ;
#30132 = VERTEX_POINT ( 'NONE', #20962 ) ;
#30133 = ORIENTED_EDGE ( 'NONE', *, *, #48709, .F. ) ;
#30134 = ORIENTED_EDGE ( 'NONE', *, *, #3482, .F. ) ;
#30135 = DIRECTION ( 'NONE',  ( 0.007781995580012663651, 0.000000000000000000, -0.9999697198139515519 ) ) ;
#30136 = EDGE_CURVE ( 'NONE', #35585, #28807, #25509, .T. ) ;
#30137 = CARTESIAN_POINT ( 'NONE',  ( -20.54204810873173415, 0.000000000000000000, 4.860550213503115558 ) ) ;
#30138 = DIRECTION ( 'NONE',  ( 0.000000000000000000, -1.000000000000000000, 0.000000000000000000 ) ) ;
#30139 = EDGE_CURVE ( 'NONE', #39543, #3963, #8199, .T. ) ;
#30140 = DIRECTION ( 'NONE',  ( 0.007781995580012663651, -3.146120232559066537E-19, -0.9999697198139514409 ) ) ;
#30141 = EDGE_LOOP ( 'NONE', ( #54374, #7429, #41262, #35737 ) ) ;
#30142 = ORIENTED_EDGE ( 'NONE', *, *, #27193, .F. ) ;
#30143 = VECTOR ( 'NONE', #11867, 1000.000000000000227 ) ;
#30144 = EDGE_CURVE ( 'NONE', #26056, #11768, #29797, .T. ) ;
#30145 = EDGE_CURVE ( 'NONE', #3478, #13447, #21254, .T. ) ;
#30146 = ORIENTED_EDGE ( 'NONE', *, *, #21864, .F. ) ;
#30147 = CARTESIAN_POINT ( 'NONE',  ( -17.46532115785441519, 0.000000000000000000, 13.67492996699914265 ) ) ;
#30148 = ORIENTED_EDGE ( 'NONE', *, *, #37441, .F. ) ;
#30149 = AXIS2_PLACEMENT_3D ( 'NONE', #52612, #35575, #39585 ) ;
#30150 = CARTESIAN_POINT ( 'NONE',  ( -14.93495759592298988, 0.000000000000000000, 12.77129166681078409 ) ) ;
#30151 = ORIENTED_EDGE ( 'NONE', *, *, #23745, .F. ) ;
#30152 = CARTESIAN_POINT ( 'NONE',  ( -8.862326071713864550, -0.04157877016374941087, 4.177890584275355756 ) ) ;
#30153 = CARTESIAN_POINT ( 'NONE',  ( -19.04209547915586143, -1.651309408375658760, 4.225232257889047105 ) ) ;
#30154 = AXIS2_PLACEMENT_3D ( 'NONE', #43129, #13319, #26346 ) ;
#30155 = VECTOR ( 'NONE', #41736, 999.9999999999998863 ) ;
#30156 = ORIENTED_EDGE ( 'NONE', *, *, #32629, .T. ) ;
#30157 = DIRECTION ( 'NONE',  ( 0.000000000000000000, 1.000000000000000000, 0.000000000000000000 ) ) ;
#30158 = ORIENTED_EDGE ( 'NONE', *, *, #5282, .F. ) ;
#30159 = ADVANCED_FACE ( 'NONE', ( #39133 ), #13022, .F. ) ;
#30160 = VECTOR ( 'NONE', #24395, 1000.000000000000114 ) ;
#30161 = CARTESIAN_POINT ( 'NONE',  ( -11.72533226533460038, 1.581621852479005774, 1.185986959513134487 ) ) ;
#30162 = AXIS2_PLACEMENT_3D ( 'NONE', #9597, #47929, #22643 ) ;
#30163 = ORIENTED_EDGE ( 'NONE', *, *, #29872, .F. ) ;
#30164 = DIRECTION ( 'NONE',  ( 0.5364919789714477361, 0.6444004775717706579, 0.5449076811759711036 ) ) ;
#30165 = CARTESIAN_POINT ( 'NONE',  ( -21.47263955680318404, 0.000000000000000000, 5.022634149262071190 ) ) ;
#30166 = CARTESIAN_POINT ( 'NONE',  ( -13.53118798318999794, 5.305366725996512045, 10.84430469370666117 ) ) ;
#30167 = VERTEX_POINT ( 'NONE', #55914 ) ;
#30168 = DIRECTION ( 'NONE',  ( -0.6427681459581293666, -0.7660444431189770143, -0.005002170337467561935 ) ) ;
#30169 = LINE ( 'NONE', #47197, #44581 ) ;
#30170 = DIRECTION ( 'NONE',  ( -0.6427681459581293666, -0.7660444431189770143, -0.005002170337467561935 ) ) ;
#30171 = VECTOR ( 'NONE', #10707, 1000.000000000000227 ) ;
#30172 = CARTESIAN_POINT ( 'NONE',  ( -26.13415699229845757, -0.1191753592594197858, 6.933020519852192365 ) ) ;
#30173 = PLANE ( 'NONE',  #23069 ) ;
#30174 = PLANE ( 'NONE',  #54226 ) ;
#30175 = FACE_OUTER_BOUND ( 'NONE', #44624, .T. ) ;
#30176 = ORIENTED_EDGE ( 'NONE', *, *, #20665, .F. ) ;
#30177 = CARTESIAN_POINT ( 'NONE',  ( -10.86170260555895695, 0.000000000000000000, 1.042558146282530629 ) ) ;
#30178 = DIRECTION ( 'NONE',  ( 0.7660212471507180654, -0.6427876096865404731, 0.005961354470445141482 ) ) ;
#30179 = CARTESIAN_POINT ( 'NONE',  ( -18.32906394269043560, 0.000000000000000000, 5.247104237792575177 ) ) ;
#30180 = ORIENTED_EDGE ( 'NONE', *, *, #40352, .F. ) ;
#30181 = CARTESIAN_POINT ( 'NONE',  ( -14.05230480659183989, -0.1191753592594174960, 5.919048077796793095 ) ) ;
#30182 = DIRECTION ( 'NONE',  ( 0.5449076811759707706, 0.6444004775717708799, -0.5364919789714476250 ) ) ;
#30183 = EDGE_LOOP ( 'NONE', ( #23015, #48028 ) ) ;
#30184 = AXIS2_PLACEMENT_3D ( 'NONE', #9266, #47908, #13278 ) ;
#30185 = LINE ( 'NONE', #12317, #12608 ) ;
#30186 = DIRECTION ( 'NONE',  ( -0.5449076811759708816, 0.6444004775717707689, 0.5364919789714475140 ) ) ;
#30187 = ADVANCED_FACE ( 'NONE', ( #17014 ), #34333, .F. ) ;
#30188 = AXIS2_PLACEMENT_3D ( 'NONE', #278, #9949, #27254 ) ;
#30189 = PLANE ( 'NONE',  #26011 ) ;
#30190 = CARTESIAN_POINT ( 'NONE',  ( -69.24581943945996443, 0.1330540280733476244, -6.471852447751588855 ) ) ;
#30191 = ORIENTED_EDGE ( 'NONE', *, *, #34401, .F. ) ;
#30192 = VERTEX_POINT ( 'NONE', #4245 ) ;
#30193 = CARTESIAN_POINT ( 'NONE',  ( -13.43470767021154089, -4.403642575758163424, 1.959318567117884546 ) ) ;
#30194 = CARTESIAN_POINT ( 'NONE',  ( -13.27065584551087163, 0.000000000000000000, 12.04557950825129176 ) ) ;
#30195 = AXIS2_PLACEMENT_3D ( 'NONE', #24137, #1432, #41168 ) ;
#30196 = LINE ( 'NONE', #48067, #6048 ) ;
#30197 = EDGE_CURVE ( 'NONE', #24558, #10708, #21558, .T. ) ;
#30198 = VECTOR ( 'NONE', #13426, 999.9999999999998863 ) ;
#30199 = LINE ( 'NONE', #13705, #41122 ) ;
#30200 = VECTOR ( 'NONE', #10430, 1000.000000000000227 ) ;
#30201 = LINE ( 'NONE', #26223, #41009 ) ;
#30202 = DIRECTION ( 'NONE',  ( -0.7660212471507179544, -0.6427876096865405842, -0.005961354470445141482 ) ) ;
#30204 = ADVANCED_FACE ( 'NONE', ( #30350 ), #28852, .F. ) ;
#30203 = VERTEX_POINT ( 'NONE', #51903 ) ;
#30205 = DIRECTION ( 'NONE',  ( 0.000000000000000000, -1.000000000000000000, 0.000000000000000000 ) ) ;
#30206 = EDGE_CURVE ( 'NONE', #31801, #50295, #20615, .T. ) ;
#30207 = VECTOR ( 'NONE', #47527, 1000.000000000000000 ) ;
#30208 = LINE ( 'NONE', #42983, #45994 ) ;
#30209 = VECTOR ( 'NONE', #38345, 999.9999999999998863 ) ;
#30210 = ORIENTED_EDGE ( 'NONE', *, *, #6611, .F. ) ;
#30211 = DIRECTION ( 'NONE',  ( 0.005002170337468016433, -0.7660444431189770143, -0.6427681459581293666 ) ) ;
#30212 = ADVANCED_FACE ( 'NONE', ( #24857 ), #33941, .F. ) ;
#30213 = DIRECTION ( 'NONE',  ( 0.9999697198139515519, 0.000000000000000000, 0.007781995580013368816 ) ) ;
#30214 = DIRECTION ( 'NONE',  ( 0.000000000000000000, 1.000000000000000000, 0.000000000000000000 ) ) ;
#30215 = ORIENTED_EDGE ( 'NONE', *, *, #44200, .F. ) ;
#30216 = CARTESIAN_POINT ( 'NONE',  ( -11.21901323774118708, 0.000000000000000000, 1.039777472322872098 ) ) ;
#30217 = EDGE_CURVE ( 'NONE', #32158, #17870, #15485, .T. ) ;
#30218 = VECTOR ( 'NONE', #30030, 1000.000000000000114 ) ;
#30219 = ORIENTED_EDGE ( 'NONE', *, *, #23733, .F. ) ;
#30220 = VECTOR ( 'NONE', #18333, 1000.000000000000227 ) ;
#30221 = ADVANCED_FACE ( 'NONE', ( #7841 ), #42467, .F. ) ;
#30222 = VERTEX_POINT ( 'NONE', #46718 ) ;
#30223 = VERTEX_POINT ( 'NONE', #33643 ) ;
#30224 = ORIENTED_EDGE ( 'NONE', *, *, #3418, .T. ) ;
#30225 = DIRECTION ( 'NONE',  ( 0.005002170337468016433, -0.7660444431189770143, -0.6427681459581293666 ) ) ;
#30226 = EDGE_LOOP ( 'NONE', ( #40736, #23458, #13919, #53598 ) ) ;
#30227 = AXIS2_PLACEMENT_3D ( 'NONE', #46334, #41800, #28190 ) ;
#30228 = FACE_OUTER_BOUND ( 'NONE', #29877, .T. ) ;
#30229 = EDGE_CURVE ( 'NONE', #22478, #13447, #20307, .T. ) ;
#30230 = ORIENTED_EDGE ( 'NONE', *, *, #34070, .F. ) ;
#30231 = PLANE ( 'NONE',  #30434 ) ;
#30232 = ORIENTED_EDGE ( 'NONE', *, *, #20596, .F. ) ;
#30233 = FACE_OUTER_BOUND ( 'NONE', #53786, .T. ) ;
#30234 = VECTOR ( 'NONE', #34128, 999.9999999999998863 ) ;
#30235 = EDGE_LOOP ( 'NONE', ( #15464, #47169, #38174, #31182 ) ) ;
#30236 = EDGE_CURVE ( 'NONE', #22227, #55768, #50696, .T. ) ;
#30237 = CARTESIAN_POINT ( 'NONE',  ( -13.48844913732735762, 0.000000000000000000, 6.023439161104203521 ) ) ;
#30238 = DIRECTION ( 'NONE',  ( -0.5364919789714478471, 0.6444004775717705469, -0.5449076811759709926 ) ) ;
#30239 = DIRECTION ( 'NONE',  ( 0.005961354470445682716, -0.6427876096865404731, -0.7660212471507180654 ) ) ;
#30240 = FACE_OUTER_BOUND ( 'NONE', #25915, .T. ) ;
#30241 = AXIS2_PLACEMENT_3D ( 'NONE', #47234, #30214, #3253 ) ;
#30242 = CARTESIAN_POINT ( 'NONE',  ( -8.577437216038198642, 0.000000000000000000, 6.061657791436306120 ) ) ;
#30243 = ORIENTED_EDGE ( 'NONE', *, *, #22692, .T. ) ;
#30244 = VECTOR ( 'NONE', #49221, 1000.000000000000114 ) ;
#30245 = AXIS2_PLACEMENT_3D ( 'NONE', #5815, #17762, #18885 ) ;
#30246 = VERTEX_POINT ( 'NONE', #2978 ) ;
#30247 = FACE_OUTER_BOUND ( 'NONE', #21432, .T. ) ;
#30248 = CARTESIAN_POINT ( 'NONE',  ( -18.66354898467281132, 0.000000000000000000, 14.21960318569776582 ) ) ;
#30249 = LINE ( 'NONE', #12385, #50546 ) ;
#30250 = AXIS2_PLACEMENT_3D ( 'NONE', #55141, #24209, #28169 ) ;
#30251 = VECTOR ( 'NONE', #5401, 999.9999999999998863 ) ;
#30252 = CARTESIAN_POINT ( 'NONE',  ( 2.072287782118878319, 0.000000000000000000, -2.950529333540147015 ) ) ;
#30253 = CARTESIAN_POINT ( 'NONE',  ( -11.26735747905060414, -0.1191753592594181482, 6.310053251662615992 ) ) ;
#30254 = DIRECTION ( 'NONE',  ( -0.005961354470445682716, -0.6427876096865404731, 0.7660212471507180654 ) ) ;
#30255 = ORIENTED_EDGE ( 'NONE', *, *, #15586, .T. ) ;
#30256 = CARTESIAN_POINT ( 'NONE',  ( -14.66887761629205222, 0.000000000000000000, 12.58869632783390990 ) ) ;
#30257 = DIRECTION ( 'NONE',  ( -0.005961354470445682716, -0.6427876096865404731, 0.7660212471507180654 ) ) ;
#30258 = ORIENTED_EDGE ( 'NONE', *, *, #46003, .T. ) ;
#30259 = CARTESIAN_POINT ( 'NONE',  ( -9.513398082562453340, 0.000000000000000000, 6.913700467289853435 ) ) ;
#30260 = LINE ( 'NONE', #47278, #31500 ) ;
#30261 = EDGE_CURVE ( 'NONE', #4723, #9720, #54659, .T. ) ;
#30262 = DIRECTION ( 'NONE',  ( -0.000000000000000000, -0.000000000000000000, 1.000000000000000000 ) ) ;
#30263 = DIRECTION ( 'NONE',  ( -0.005961354470445682716, -0.6427876096865404731, 0.7660212471507180654 ) ) ;
#30264 = ORIENTED_EDGE ( 'NONE', *, *, #1785, .T. ) ;
#30265 = AXIS2_PLACEMENT_3D ( 'NONE', #37544, #46070, #7178 ) ;
#30266 = EDGE_LOOP ( 'NONE', ( #42635, #35056, #32593, #49638 ) ) ;
#30267 = DIRECTION ( 'NONE',  ( -0.005002170337468016433, -0.7660444431189770143, 0.6427681459581293666 ) ) ;
#30268 = LINE ( 'NONE', #32514, #34032 ) ;
#30269 = DIRECTION ( 'NONE',  ( 0.7660212471507180654, -0.6427876096865404731, 0.005961354470445141482 ) ) ;
#30270 = VECTOR ( 'NONE', #37859, 999.9999999999998863 ) ;
#30271 = LINE ( 'NONE', #39347, #40038 ) ;
#30272 = DIRECTION ( 'NONE',  ( -0.6427681459581293666, -0.7660444431189770143, -0.005002170337467561935 ) ) ;
#30273 = AXIS2_PLACEMENT_3D ( 'NONE', #12197, #20438, #42576 ) ;
#30274 = DIRECTION ( 'NONE',  ( 0.9999697198139515519, 0.000000000000000000, 0.007781995580013368816 ) ) ;
#30275 = FACE_OUTER_BOUND ( 'NONE', #17229, .T. ) ;
#30277 = EDGE_CURVE ( 'NONE', #36770, #38019, #15768, .T. ) ;
#30276 = VERTEX_POINT ( 'NONE', #37643 ) ;
#30278 = DIRECTION ( 'NONE',  ( -0.005002170337468016433, -0.7660444431189770143, 0.6427681459581293666 ) ) ;
#30279 = LINE ( 'NONE', #52424, #2417 ) ;
#30280 = VECTOR ( 'NONE', #28383, 999.9999999999998863 ) ;
#30281 = EDGE_LOOP ( 'NONE', ( #41758, #41862, #46651, #5250 ) ) ;
#30282 = DIRECTION ( 'NONE',  ( 0.007781995580012663651, 0.000000000000000000, -0.9999697198139515519 ) ) ;
#30283 = VERTEX_POINT ( 'NONE', #16070 ) ;
#30284 = DIRECTION ( 'NONE',  ( 0.7660212471507180654, -0.6427876096865404731, 0.005961354470445141482 ) ) ;
#30285 = AXIS2_PLACEMENT_3D ( 'NONE', #17898, #5385, #27230 ) ;
#30286 = EDGE_LOOP ( 'NONE', ( #34682, #18623, #25468, #56139 ) ) ;
#30287 = EDGE_CURVE ( 'NONE', #46842, #6581, #47007, .T. ) ;
#30288 = ORIENTED_EDGE ( 'NONE', *, *, #15082, .F. ) ;
#30289 = EDGE_CURVE ( 'NONE', #52782, #7637, #16610, .T. ) ;
#30290 = VECTOR ( 'NONE', #352, 1000.000000000000114 ) ;
#30291 = EDGE_LOOP ( 'NONE', ( #12811, #32648, #22038, #8158 ) ) ;
#30292 = VERTEX_POINT ( 'NONE', #11535 ) ;
#30293 = VECTOR ( 'NONE', #41076, 1000.000000000000227 ) ;
#30294 = VERTEX_POINT ( 'NONE', #24304 ) ;
#30295 = EDGE_LOOP ( 'NONE', ( #14900, #26866, #20005, #47241 ) ) ;
#30296 = CARTESIAN_POINT ( 'NONE',  ( -17.26532721389163072, 0.000000000000000000, 13.67648636611514590 ) ) ;
#30297 = LINE ( 'NONE', #39374, #1173 ) ;
#30298 = CARTESIAN_POINT ( 'NONE',  ( 4.994031378522669762, 0.000000000000000000, -2.289010529401725780 ) ) ;
#30299 = EDGE_CURVE ( 'NONE', #25456, #50706, #42176, .T. ) ;
#30300 = VERTEX_POINT ( 'NONE', #11235 ) ;
#30301 = LINE ( 'NONE', #55558, #21297 ) ;
#30302 = ORIENTED_EDGE ( 'NONE', *, *, #31634, .F. ) ;
#30303 = VERTEX_POINT ( 'NONE', #7257 ) ;
#30304 = EDGE_CURVE ( 'NONE', #19686, #20073, #38185, .T. ) ;
#30305 = CARTESIAN_POINT ( 'NONE',  ( -16.81345671998191449, 0.000000000000000000, 3.412238694616132495 ) ) ;
#30306 = VECTOR ( 'NONE', #29296, 999.9999999999998863 ) ;
#30307 = PLANE ( 'NONE',  #35047 ) ;
#30308 = ORIENTED_EDGE ( 'NONE', *, *, #52802, .T. ) ;
#30309 = CARTESIAN_POINT ( 'NONE',  ( -15.61019731987982873, -1.975113310420657520, 5.986959926383320862 ) ) ;
#30310 = VECTOR ( 'NONE', #36193, 999.9999999999998863 ) ;
#30311 = ORIENTED_EDGE ( 'NONE', *, *, #51039, .F. ) ;
#30312 = CARTESIAN_POINT ( 'NONE',  ( -18.06838721921171498, 3.524445264749008988, 9.683911437457039639 ) ) ;
#30314 = VECTOR ( 'NONE', #22055, 999.9999999999998863 ) ;
#30313 = CARTESIAN_POINT ( 'NONE',  ( -22.40634380310664397, 0.000000000000000000, 5.584705972946605534 ) ) ;
#30315 = DIRECTION ( 'NONE',  ( 0.9999697198139515519, 0.000000000000000000, 0.007781995580013368816 ) ) ;
#30316 = CARTESIAN_POINT ( 'NONE',  ( 2.072287782118878319, 0.000000000000000000, -2.950529333540147015 ) ) ;
#30317 = DIRECTION ( 'NONE',  ( 0.007781995580012663651, -3.146120232559066537E-19, -0.9999697198139514409 ) ) ;
#30318 = PLANE ( 'NONE',  #39408 ) ;
#30319 = LINE ( 'NONE', #22377, #42044 ) ;
#30320 = VECTOR ( 'NONE', #20358, 999.9999999999998863 ) ;
#30321 = LINE ( 'NONE', #47642, #3220 ) ;
#30322 = ORIENTED_EDGE ( 'NONE', *, *, #43197, .F. ) ;
#30323 = CARTESIAN_POINT ( 'NONE',  ( -19.60912206198628027, -0.1191753592594197858, 4.398475361799976113 ) ) ;
#30324 = EDGE_CURVE ( 'NONE', #26517, #37130, #55502, .T. ) ;
#30325 = VECTOR ( 'NONE', #52459, 999.9999999999998863 ) ;
#30326 = CARTESIAN_POINT ( 'NONE',  ( -15.90797834045089587, -0.1191753592594207017, 5.535274727466993561 ) ) ;
#30327 = FACE_OUTER_BOUND ( 'NONE', #3081, .T. ) ;
#30328 = DIRECTION ( 'NONE',  ( -0.5449076811759708816, 0.6444004775717707689, 0.5364919789714475140 ) ) ;
#30329 = EDGE_CURVE ( 'NONE', #25044, #3649, #19767, .T. ) ;
#30330 = DIRECTION ( 'NONE',  ( 0.6427681459581294776, -0.7660444431189769032, 0.005002170337467562802 ) ) ;
#30331 = DIRECTION ( 'NONE',  ( 0.000000000000000000, 1.000000000000000000, 0.000000000000000000 ) ) ;
#30332 = DIRECTION ( 'NONE',  ( -0.005961354470445682716, -0.6427876096865404731, 0.7660212471507180654 ) ) ;
#30333 = AXIS2_PLACEMENT_3D ( 'NONE', #28587, #18966, #10449 ) ;
#30334 = DIRECTION ( 'NONE',  ( -0.7660212471507179544, -0.6427876096865405842, -0.005961354470445141482 ) ) ;
#30335 = VECTOR ( 'NONE', #7530, 1000.000000000000227 ) ;
#30336 = APPLICATION_PROTOCOL_DEFINITION ( 'draft international standard', 'automotive_design', 1998, #16258 ) ;
#30337 = ORIENTED_EDGE ( 'NONE', *, *, #22568, .F. ) ;
#30338 = EDGE_CURVE ( 'NONE', #39017, #50804, #54387, .T. ) ;
#30339 = FACE_OUTER_BOUND ( 'NONE', #38183, .T. ) ;
#30340 = DIRECTION ( 'NONE',  ( -0.7660212471507179544, -0.6427876096865405842, -0.005961354470445141482 ) ) ;
#30341 = DIRECTION ( 'NONE',  ( 0.6427681459581294776, -0.7660444431189769032, 0.005002170337467562802 ) ) ;
#30342 = EDGE_CURVE ( 'NONE', #38273, #22275, #45887, .T. ) ;
#30343 = ADVANCED_FACE ( 'NONE', ( #18023 ), #8110, .F. ) ;
#30344 = EDGE_CURVE ( 'NONE', #37808, #45566, #39321, .T. ) ;
#30345 = DIRECTION ( 'NONE',  ( -0.3313982828793700097, 0.4028455766673915694, -0.8531650599175529814 ) ) ;
#30346 = CARTESIAN_POINT ( 'NONE',  ( -14.01701317841955508, 0.000000000000000000, 2.326005055450897085 ) ) ;
#30347 = CARTESIAN_POINT ( 'NONE',  ( -22.40478740399063895, 0.000000000000000000, 5.384712028983816623 ) ) ;
#30348 = DIRECTION ( 'NONE',  ( 0.5449076811759707706, 0.6444004775717708799, -0.5364919789714476250 ) ) ;
#30349 = AXIS2_PLACEMENT_3D ( 'NONE', #13543, #24689, #50810 ) ;
#30350 = FACE_OUTER_BOUND ( 'NONE', #40541, .T. ) ;
#30351 = CARTESIAN_POINT ( 'NONE',  ( -9.353677591794285817, 2.186419275952748986, 2.912935481226179402 ) ) ;
#30352 = VECTOR ( 'NONE', #50531, 1000.000000000000227 ) ;
#30353 = ORIENTED_EDGE ( 'NONE', *, *, #8424, .F. ) ;
#30354 = CARTESIAN_POINT ( 'NONE',  ( -19.60990026154428278, 0.000000000000000000, 4.498472333781370125 ) ) ;
#30355 = AXIS2_PLACEMENT_3D ( 'NONE', #33869, #51190, #12302 ) ;
#30356 = ORIENTED_EDGE ( 'NONE', *, *, #4762, .T. ) ;
#30357 = EDGE_CURVE ( 'NONE', #2187, #14051, #4673, .T. ) ;
#30358 = EDGE_CURVE ( 'NONE', #21510, #37821, #43852, .T. ) ;
#30359 = ORIENTED_EDGE ( 'NONE', *, *, #28980, .T. ) ;
#30360 = ORIENTED_EDGE ( 'NONE', *, *, #54295, .F. ) ;
#30361 = VECTOR ( 'NONE', #18667, 999.9999999999998863 ) ;
#30362 = ORIENTED_EDGE ( 'NONE', *, *, #39654, .T. ) ;
#30363 = EDGE_CURVE ( 'NONE', #49603, #54423, #9212, .T. ) ;
#30364 = VECTOR ( 'NONE', #5564, 999.9999999999998863 ) ;
#30365 = ORIENTED_EDGE ( 'NONE', *, *, #29645, .F. ) ;
#30366 = DIRECTION ( 'NONE',  ( 0.005961354470445682716, -0.6427876096865404731, -0.7660212471507180654 ) ) ;
#30367 = FACE_OUTER_BOUND ( 'NONE', #29077, .T. ) ;
#30368 = AXIS2_PLACEMENT_3D ( 'NONE', #34632, #34944, #21855 ) ;
#30369 = ADVANCED_FACE ( 'NONE', ( #30247 ), #408, .F. ) ;
#30370 = ORIENTED_EDGE ( 'NONE', *, *, #891, .F. ) ;
#30371 = EDGE_CURVE ( 'NONE', #15287, #51394, #26005, .T. ) ;
#30372 = AXIS2_PLACEMENT_3D ( 'NONE', #13774, #30576, #52124 ) ;
#30373 = VECTOR ( 'NONE', #17752, 1000.000000000000227 ) ;
#30374 = CARTESIAN_POINT ( 'NONE',  ( -12.78414981984007071, -5.213152330870663320, 10.20340078340005974 ) ) ;
#30375 = ORIENTED_EDGE ( 'NONE', *, *, #7980, .F. ) ;
#30376 = LINE ( 'NONE', #47694, #19179 ) ;
#30377 = DIRECTION ( 'NONE',  ( 0.007781995580012663651, 0.000000000000000000, -0.9999697198139515519 ) ) ;
#30378 = VERTEX_POINT ( 'NONE', #43323 ) ;
#30379 = DIRECTION ( 'NONE',  ( 0.007781995580012663651, -3.146120232559066537E-19, -0.9999697198139514409 ) ) ;
#30380 = ORIENTED_EDGE ( 'NONE', *, *, #41778, .T. ) ;
#30381 = DIRECTION ( 'NONE',  ( -0.6427681459581293666, -0.7660444431189770143, -0.005002170337467561935 ) ) ;
#30382 = VECTOR ( 'NONE', #16708, 999.9999999999998863 ) ;
#30383 = DIRECTION ( 'NONE',  ( 0.5449076811759707706, 0.6444004775717708799, -0.5364919789714476250 ) ) ;
#30384 = ORIENTED_EDGE ( 'NONE', *, *, #35611, .F. ) ;
#30385 = DIRECTION ( 'NONE',  ( 0.5364919789714477361, 0.6444004775717706579, 0.5449076811759711036 ) ) ;
#30386 = LINE ( 'NONE', #21842, #35648 ) ;
#30388 = VECTOR ( 'NONE', #22356, 1000.000000000000000 ) ;
#30387 = LINE ( 'NONE', #3424, #5803 ) ;
#30389 = DIRECTION ( 'NONE',  ( -0.9999697198139514409, 0.000000000000000000, -0.007781995580013368816 ) ) ;
#30390 = ORIENTED_EDGE ( 'NONE', *, *, #51327, .T. ) ;
#30391 = VECTOR ( 'NONE', #16622, 1000.000000000000227 ) ;
#30392 = DIRECTION ( 'NONE',  ( 0.005002170337468016433, -0.7660444431189770143, -0.6427681459581293666 ) ) ;
#30393 = CARTESIAN_POINT ( 'NONE',  ( -45.77156441860525149, 4.499999999999981348, -5.000000000000000000 ) ) ;
#30394 = DIRECTION ( 'NONE',  ( -0.005002170337468016433, -0.7660444431189770143, 0.6427681459581293666 ) ) ;
#30395 = CARTESIAN_POINT ( 'NONE',  ( -16.53317331066696383, 0.000000000000000000, 13.31285208727739899 ) ) ;
#30396 = VECTOR ( 'NONE', #16194, 1000.000000000000227 ) ;
#30397 = CARTESIAN_POINT ( 'NONE',  ( -15.09516764022381174, 0.000000000000000000, 7.657589599010205639 ) ) ;
#30398 = DIRECTION ( 'NONE',  ( -0.5364919789714478471, 0.6444004775717705469, -0.5449076811759709926 ) ) ;
#30399 = DIRECTION ( 'NONE',  ( 0.000000000000000000, -0.000000000000000000, -1.000000000000000000 ) ) ;
#30401 = VECTOR ( 'NONE', #13192, 1000.000000000000227 ) ;
#30400 = PLANE ( 'NONE',  #257 ) ;
#30402 = DIRECTION ( 'NONE',  ( 0.005002170337468016433, -0.7660444431189770143, -0.6427681459581293666 ) ) ;
#30403 = VECTOR ( 'NONE', #15424, 1000.000000000000227 ) ;
#30404 = SURFACE_STYLE_USAGE ( .BOTH. , #51121 ) ;
#30406 = CARTESIAN_POINT ( 'NONE',  ( -20.56906454177918064, -5.051250379848161387, 12.96161735426753303 ) ) ;
#30405 = VECTOR ( 'NONE', #23362, 999.9999999999998863 ) ;
#30407 = VERTEX_POINT ( 'NONE', #4415 ) ;
#30408 = DIRECTION ( 'NONE',  ( 0.005961354470445682716, -0.6427876096865404731, -0.7660212471507180654 ) ) ;
#30409 = LINE ( 'NONE', #35784, #17273 ) ;
#30410 = AXIS2_PLACEMENT_3D ( 'NONE', #42805, #51355, #47351 ) ;
#30411 = EDGE_CURVE ( 'NONE', #15538, #11444, #17444, .T. ) ;
#30412 = EDGE_CURVE ( 'NONE', #30623, #40953, #34780, .T. ) ;
#30413 = CARTESIAN_POINT ( 'NONE',  ( -23.27598415104352014, 19.08968832676502458, -4.485782677847319100 ) ) ;
#30414 = EDGE_CURVE ( 'NONE', #25905, #37607, #13489, .T. ) ;
#30415 = DIRECTION ( 'NONE',  ( -0.9999697198139514409, -0.000000000000000000, -0.007781995580013368816 ) ) ;
#30416 = LINE ( 'NONE', #35243, #47401 ) ;
#30417 = VERTEX_POINT ( 'NONE', #39037 ) ;
#30418 = VECTOR ( 'NONE', #47041, 999.9999999999998863 ) ;
#30419 = VECTOR ( 'NONE', #8461, 999.9999999999998863 ) ;
#30420 = VERTEX_POINT ( 'NONE', #12915 ) ;
#30421 = DIRECTION ( 'NONE',  ( 1.000000000000000000, 0.000000000000000000, -1.224646799147353207E-16 ) ) ;
#30422 = FACE_OUTER_BOUND ( 'NONE', #5226, .T. ) ;
#30423 = ORIENTED_EDGE ( 'NONE', *, *, #101, .F. ) ;
#30424 = LINE ( 'NONE', #8856, #21179 ) ;
#30425 = ORIENTED_EDGE ( 'NONE', *, *, #40140, .F. ) ;
#30426 = DIRECTION ( 'NONE',  ( -0.005961354470445682716, -0.6427876096865404731, 0.7660212471507180654 ) ) ;
#30427 = VERTEX_POINT ( 'NONE', #39625 ) ;
#30428 = DIRECTION ( 'NONE',  ( 0.007781995580012663651, 0.000000000000000000, -0.9999697198139515519 ) ) ;
#30429 = EDGE_CURVE ( 'NONE', #6407, #26740, #43019, .T. ) ;
#30430 = VECTOR ( 'NONE', #3000, 999.9999999999998863 ) ;
#30431 = VERTEX_POINT ( 'NONE', #55803 ) ;
#30432 = EDGE_LOOP ( 'NONE', ( #54346, #11110, #29601, #13259 ) ) ;
#30433 = EDGE_LOOP ( 'NONE', ( #9335, #54358, #31534, #55351, #28932, #5477, #32732, #47301 ) ) ;
#30434 = AXIS2_PLACEMENT_3D ( 'NONE', #94, #55224, #47546 ) ;
#30435 = CARTESIAN_POINT ( 'NONE',  ( -14.46888367232926420, 0.000000000000000000, 12.59025272694991315 ) ) ;
#30436 = FACE_OUTER_BOUND ( 'NONE', #764, .T. ) ;
#30437 = VECTOR ( 'NONE', #2453, 1000.000000000000227 ) ;
#30438 = CARTESIAN_POINT ( 'NONE',  ( -10.74029228357944987, 0.000000000000000000, 11.14194120806293320 ) ) ;
#30439 = EDGE_CURVE ( 'NONE', #50871, #26864, #13748, .T. ) ;
#30440 = DIRECTION ( 'NONE',  ( 0.9999697198139515519, 0.000000000000000000, 0.007781995580013368816 ) ) ;
#30441 = EDGE_LOOP ( 'NONE', ( #56002, #37543, #6523 ) ) ;
#30442 = VECTOR ( 'NONE', #40797, 999.9999999999998863 ) ;
#30443 = EDGE_LOOP ( 'NONE', ( #28110, #14287, #28962, #7942 ) ) ;
#30444 = EDGE_CURVE ( 'NONE', #4538, #13662, #25416, .T. ) ;
#30445 = ORIENTED_EDGE ( 'NONE', *, *, #18569, .F. ) ;
#30446 = CIRCLE ( 'NONE', #29551, 2.125000000000000000 ) ;
#30447 = AXIS2_PLACEMENT_3D ( 'NONE', #27089, #43080, #4193 ) ;
#30448 = ADVANCED_FACE ( 'NONE', ( #21148 ), #47854, .F. ) ;
#30449 = DIRECTION ( 'NONE',  ( 0.5364919789714477361, 0.6444004775717706579, 0.5449076811759711036 ) ) ;
#30450 = ORIENTED_EDGE ( 'NONE', *, *, #49369, .F. ) ;
#30451 = LINE ( 'NONE', #12563, #20275 ) ;
#30452 = EDGE_CURVE ( 'NONE', #29102, #19178, #47263, .T. ) ;
#30453 = ORIENTED_EDGE ( 'NONE', *, *, #46894, .F. ) ;
#30454 = PLANE ( 'NONE',  #36922 ) ;
#30455 = CARTESIAN_POINT ( 'NONE',  ( -26.13415699229845757, -0.1191753592594197858, 6.933020519852192365 ) ) ;
#30456 = AXIS2_PLACEMENT_3D ( 'NONE', #32508, #49548, #28220 ) ;
#30457 = EDGE_LOOP ( 'NONE', ( #47545, #28536, #45479, #27462, #31887 ) ) ;
#30458 = AXIS2_PLACEMENT_3D ( 'NONE', #29753, #22044, #39373 ) ;
#30459 = EDGE_CURVE ( 'NONE', #15204, #19054, #13208, .T. ) ;
#30460 = DIRECTION ( 'NONE',  ( 0.5449076811759707706, 0.6444004775717708799, -0.5364919789714476250 ) ) ;
#30461 = VECTOR ( 'NONE', #2400, 1000.000000000000227 ) ;
#30462 = ORIENTED_EDGE ( 'NONE', *, *, #51310, .F. ) ;
#30463 = AXIS2_PLACEMENT_3D ( 'NONE', #19446, #10385, #24532 ) ;
#30464 = LINE ( 'NONE', #34164, #28173 ) ;
#30465 = AXIS2_PLACEMENT_3D ( 'NONE', #24875, #8127, #50974 ) ;
#30466 = VERTEX_POINT ( 'NONE', #17179 ) ;
#30467 = CARTESIAN_POINT ( 'NONE',  ( -17.25977937193981404, 5.305366725996510269, 12.29261621259364112 ) ) ;
#30468 = CARTESIAN_POINT ( 'NONE',  ( -10.27421835998572064, 0.000000000000000000, 10.96090226820206048 ) ) ;
#30469 = PLANE ( 'NONE',  #39147 ) ;
#30470 = ORIENTED_EDGE ( 'NONE', *, *, #31290, .T. ) ;
#30471 = CARTESIAN_POINT ( 'NONE',  ( -14.05517886009712036, -0.1191753592594174960, 6.288357781054557449 ) ) ;
#30472 = CARTESIAN_POINT ( 'NONE',  ( -13.73672976910459909, 0.000000000000000000, 12.22661844811216270 ) ) ;
#30473 = DIRECTION ( 'NONE',  ( 0.7660212471507180654, -0.6427876096865404731, 0.005961354470445141482 ) ) ;
#30474 = CARTESIAN_POINT ( 'NONE',  ( -16.93204742750033631, 5.467268677019011314, 12.43102267950012951 ) ) ;
#30475 = FACE_OUTER_BOUND ( 'NONE', #55825, .T. ) ;
#30476 = CARTESIAN_POINT ( 'NONE',  ( 2.072287782118878319, 0.000000000000000000, -2.950529333540147015 ) ) ;
#30477 = AXIS2_PLACEMENT_3D ( 'NONE', #55680, #55981, #282 ) ;
#30478 = PLANE ( 'NONE',  #54864 ) ;
#30479 = ORIENTED_EDGE ( 'NONE', *, *, #13184, .T. ) ;
#30480 = DIRECTION ( 'NONE',  ( 0.9999697198139515519, 0.000000000000000000, 0.007781995580013368816 ) ) ;
#30481 = FACE_OUTER_BOUND ( 'NONE', #11889, .T. ) ;
#30482 = LINE ( 'NONE', #48631, #35070 ) ;
#30483 = VERTEX_POINT ( 'NONE', #8957 ) ;
#30484 = CARTESIAN_POINT ( 'NONE',  ( -27.99923088623136636, 0.000000000000000000, 7.757173251277078130 ) ) ;
#30485 = VECTOR ( 'NONE', #17760, 1000.000000000000114 ) ;
#30486 = VERTEX_POINT ( 'NONE', #26259 ) ;
#30487 = ADVANCED_FACE ( 'NONE', ( #37932 ), #50961, .F. ) ;
#30488 = FACE_OUTER_BOUND ( 'NONE', #50018, .T. ) ;
#30489 = CARTESIAN_POINT ( 'NONE',  ( -10.44554592974990470, 0.000000000000000000, 7.275778347011597980 ) ) ;
#30490 = AXIS2_PLACEMENT_3D ( 'NONE', #24177, #50573, #10830 ) ;
#30491 = ADVANCED_FACE ( 'NONE', ( #55239 ), #32813, .F. ) ;
#30492 = EDGE_CURVE ( 'NONE', #30714, #46212, #33946, .T. ) ;
#30493 = LINE ( 'NONE', #51506, #50471 ) ;
#30494 = CARTESIAN_POINT ( 'NONE',  ( -67.20861331203366262, 1.999999999987024379, -0.6963329337696058108 ) ) ;
#30495 = EDGE_LOOP ( 'NONE', ( #10866, #30380, #36724, #2900 ) ) ;
#30496 = VECTOR ( 'NONE', #14735, 1000.000000000000227 ) ;
#30497 = AXIS2_PLACEMENT_3D ( 'NONE', #54573, #37270, #2360 ) ;
#30498 = EDGE_LOOP ( 'NONE', ( #42319, #13623, #40495, #43290 ) ) ;
#30499 = CARTESIAN_POINT ( 'NONE',  ( -15.98863513745331311, 0.000000000000000000, 3.049325577086037242 ) ) ;
#30500 = DIRECTION ( 'NONE',  ( -0.005002170337468016433, -0.7660444431189770143, 0.6427681459581293666 ) ) ;
#30501 = DIRECTION ( 'NONE',  ( 0.9999697198139515519, 0.000000000000000000, 0.007781995580013368816 ) ) ;
#30502 = VECTOR ( 'NONE', #40744, 999.9999999999998863 ) ;
#30503 = LINE ( 'NONE', #8629, #33870 ) ;
#30505 = DIRECTION ( 'NONE',  ( 0.000000000000000000, -0.000000000000000000, -1.000000000000000000 ) ) ;
#30504 = VECTOR ( 'NONE', #2747, 999.9999999999998863 ) ;
#30506 = DIRECTION ( 'NONE',  ( 0.005961354470445682716, -0.6427876096865404731, -0.7660212471507180654 ) ) ;
#30507 = VERTEX_POINT ( 'NONE', #54980 ) ;
#30508 = DIRECTION ( 'NONE',  ( -0.000000000000000000, -0.000000000000000000, -1.000000000000000000 ) ) ;
#30509 = AXIS2_PLACEMENT_3D ( 'NONE', #21345, #33300, #29868 ) ;
#30510 = AXIS2_PLACEMENT_3D ( 'NONE', #19138, #53781, #3511 ) ;
#30511 = DIRECTION ( 'NONE',  ( -0.5364919789714478471, 0.6444004775717705469, -0.5449076811759709926 ) ) ;
#30512 = ORIENTED_EDGE ( 'NONE', *, *, #7588, .F. ) ;
#30513 = CARTESIAN_POINT ( 'NONE',  ( -69.11692417668358246, -9.015782624321049710, -7.493102809087829108 ) ) ;
#30514 = CARTESIAN_POINT ( 'NONE',  ( -19.15756256483321351, -0.1191753592594164135, 5.140653641833157650 ) ) ;
#30515 = CARTESIAN_POINT ( 'NONE',  ( 0.2239497891030726440, -1.668917571073584849, -5.998622290806042479 ) ) ;
#30516 = ORIENTED_EDGE ( 'NONE', *, *, #55307, .T. ) ;
#30517 = DIRECTION ( 'NONE',  ( 0.005961354470445682716, -0.6427876096865404731, -0.7660212471507180654 ) ) ;
#30518 = ORIENTED_EDGE ( 'NONE', *, *, #4284, .T. ) ;
#30519 = ADVANCED_FACE ( 'NONE', ( #15491 ), #20026, .F. ) ;
#30520 = VECTOR ( 'NONE', #1579, 999.9999999999998863 ) ;
#30521 = ORIENTED_EDGE ( 'NONE', *, *, #35668, .F. ) ;
#30522 = VERTEX_POINT ( 'NONE', #41881 ) ;
#30523 = EDGE_CURVE ( 'NONE', #10129, #4038, #50435, .T. ) ;
#30524 = ORIENTED_EDGE ( 'NONE', *, *, #52228, .F. ) ;
#30525 = CARTESIAN_POINT ( 'NONE',  ( -8.375886872959409146, 0.000000000000000000, 5.863220246589520457 ) ) ;
#30526 = VECTOR ( 'NONE', #8842, 999.9999999999998863 ) ;
#30527 = ORIENTED_EDGE ( 'NONE', *, *, #52270, .F. ) ;
#30528 = CARTESIAN_POINT ( 'NONE',  ( -13.30581722938317846, 23.24410787913973664, -3.697606465566034561 ) ) ;
#30529 = ORIENTED_EDGE ( 'NONE', *, *, #36181, .F. ) ;
#30530 = CARTESIAN_POINT ( 'NONE',  ( -17.73140113748535285, 0.000000000000000000, 13.85752530597602039 ) ) ;
#30531 = VECTOR ( 'NONE', #29798, 999.9999999999998863 ) ;
#30532 = EDGE_CURVE ( 'NONE', #36489, #17725, #3563, .T. ) ;
#30533 = ORIENTED_EDGE ( 'NONE', *, *, #39830, .T. ) ;
#30534 = LINE ( 'NONE', #51794, #8380 ) ;
#30535 = EDGE_LOOP ( 'NONE', ( #46475, #42048, #48460, #25233 ) ) ;
#30536 = VECTOR ( 'NONE', #18674, 1000.000000000000227 ) ;
#30537 = PLANE ( 'NONE',  #5745 ) ;
#30538 = CARTESIAN_POINT ( 'NONE',  ( -14.93495759592298988, 0.000000000000000000, 12.77129166681078409 ) ) ;
#30539 = DIRECTION ( 'NONE',  ( -0.9999697198139514409, -0.000000000000000000, -0.007781995580013368816 ) ) ;
#30540 = CARTESIAN_POINT ( 'NONE',  ( -18.85791280579721985, -3.594132820645661308, 9.905569753500415686 ) ) ;
#30541 = LINE ( 'NONE', #47850, #50094 ) ;
#30542 = VERTEX_POINT ( 'NONE', #24863 ) ;
#30543 = ADVANCED_FACE ( 'NONE', ( #29407 ), #7847, .F. ) ;
#30544 = VERTEX_POINT ( 'NONE', #38191 ) ;
#30545 = CIRCLE ( 'NONE', #19621, 3.000000000000001332 ) ;
#30546 = DIRECTION ( 'NONE',  ( 0.9999697198139515519, 0.000000000000000000, 0.007781995580013368816 ) ) ;
#30547 = DIRECTION ( 'NONE',  ( -0.5364919789714478471, 0.6444004775717705469, -0.5449076811759709926 ) ) ;
#30548 = EDGE_CURVE ( 'NONE', #27352, #3917, #33396, .T. ) ;
#30549 = VECTOR ( 'NONE', #4461, 999.9999999999998863 ) ;
#30550 = DIRECTION ( 'NONE',  ( 0.5449076811759707706, 0.6444004775717708799, -0.5364919789714476250 ) ) ;
#30551 = VECTOR ( 'NONE', #10072, 1000.000000000000000 ) ;
#30552 = CARTESIAN_POINT ( 'NONE',  ( -19.22961988024793101, -0.1191753592594177458, 14.39986392600063603 ) ) ;
#30553 = PLANE ( 'NONE',  #19500 ) ;
#30554 = DIRECTION ( 'NONE',  ( -0.6246952433987894571, 0.7422098413412802076, 0.2426528472758539834 ) ) ;
#30555 = ORIENTED_EDGE ( 'NONE', *, *, #50277, .F. ) ;
#30556 = CARTESIAN_POINT ( 'NONE',  ( -19.55346843781402910, -2.379430070215138304, 7.303589053828619448 ) ) ;
#30557 = ADVANCED_FACE ( 'NONE', ( #46156 ), #33651, .T. ) ;
#30558 = CARTESIAN_POINT ( 'NONE',  ( -12.70458494993575194, -0.1191753592594197858, 11.86531876794841978 ) ) ;
#30559 = EDGE_LOOP ( 'NONE', ( #28017, #12562, #39538, #20672 ) ) ;
#30560 = FACE_OUTER_BOUND ( 'NONE', #29141, .T. ) ;
#30561 = DIRECTION ( 'NONE',  ( -0.9999697198139514409, -0.000000000000000000, -0.007781995580013368816 ) ) ;
#30562 = EDGE_CURVE ( 'NONE', #46828, #47750, #37348, .T. ) ;
#30563 = CARTESIAN_POINT ( 'NONE',  ( -58.00000000000000711, -9.000000000000000000, 7.102951435054649637E-15 ) ) ;
#30564 = ADVANCED_FACE ( 'NONE', ( #11792 ), #20870, .F. ) ;
#30565 = DIRECTION ( 'NONE',  ( 0.000000000000000000, 0.000000000000000000, -1.000000000000000000 ) ) ;
#30566 = VECTOR ( 'NONE', #46925, 1000.000000000000227 ) ;
#30567 = CARTESIAN_POINT ( 'NONE',  ( -20.54049170961573267, 0.000000000000000000, 4.660556269540326646 ) ) ;
#30568 = ORIENTED_EDGE ( 'NONE', *, *, #21018, .T. ) ;
#30569 = ORIENTED_EDGE ( 'NONE', *, *, #19110, .F. ) ;
#30570 = CARTESIAN_POINT ( 'NONE',  ( -20.10835023650160736, -0.9956879032862070433, 5.875079047949166799 ) ) ;
#30571 = DIRECTION ( 'NONE',  ( 0.000000000000000000, -1.000000000000000000, 0.000000000000000000 ) ) ;
#30572 = FACE_OUTER_BOUND ( 'NONE', #3332, .T. ) ;
#30573 = EDGE_CURVE ( 'NONE', #52239, #38033, #16618, .T. ) ;
#30574 = CARTESIAN_POINT ( 'NONE',  ( -14.01545677930355183, 0.000000000000000000, 2.126011111488108174 ) ) ;
#30575 = AXIS2_PLACEMENT_3D ( 'NONE', #48135, #31105, #47599 ) ;
#30576 = DIRECTION ( 'NONE',  ( 0.000000000000000000, -1.000000000000000000, 0.000000000000000000 ) ) ;
#30577 = CARTESIAN_POINT ( 'NONE',  ( -15.08079737269739873, 0.000000000000000000, 5.811041082721382978 ) ) ;
#30578 = FACE_OUTER_BOUND ( 'NONE', #13605, .T. ) ;
#30579 = ORIENTED_EDGE ( 'NONE', *, *, #17770, .F. ) ;
#30580 = EDGE_CURVE ( 'NONE', #43208, #42953, #37669, .T. ) ;
#30582 = AXIS2_PLACEMENT_3D ( 'NONE', #53508, #44702, #5819 ) ;
#30581 = CARTESIAN_POINT ( 'NONE',  ( -16.81190032086591302, 0.000000000000000000, 3.212244750653343583 ) ) ;
#30583 = CARTESIAN_POINT ( 'NONE',  ( -16.75659533713064775, 0.000000000000000000, 8.013992054311934510 ) ) ;
#30584 = VERTEX_POINT ( 'NONE', #37096 ) ;
#30585 = CARTESIAN_POINT ( 'NONE',  ( -22.02261458013905226, 4.333955019861509328, 12.54841105031995241 ) ) ;
#30586 = EDGE_LOOP ( 'NONE', ( #20564, #48664, #45786, #32654 ) ) ;
#30587 = DIRECTION ( 'NONE',  ( -0.005961354470445682716, -0.6427876096865404731, 0.7660212471507180654 ) ) ;
#30588 = DIRECTION ( 'NONE',  ( -0.6427681459581293666, -0.7660444431189770143, -0.005002170337467561935 ) ) ;
#30589 = VERTEX_POINT ( 'NONE', #7008 ) ;
#30590 = VECTOR ( 'NONE', #42092, 1000.000000000000227 ) ;
#30591 = ORIENTED_EDGE ( 'NONE', *, *, #17450, .F. ) ;
#30592 = ORIENTED_EDGE ( 'NONE', *, *, #2822, .F. ) ;
#30593 = VECTOR ( 'NONE', #910, 1000.000000000000000 ) ;
#30594 = ORIENTED_EDGE ( 'NONE', *, *, #12054, .F. ) ;
#30595 = ORIENTED_EDGE ( 'NONE', *, *, #7882, .T. ) ;
#30596 = VERTEX_POINT ( 'NONE', #24310 ) ;
#30597 = LINE ( 'NONE', #51851, #12286 ) ;
#30598 = DIRECTION ( 'NONE',  ( -0.005002170337468016433, -0.7660444431189770143, 0.6427681459581293666 ) ) ;
#30599 = CARTESIAN_POINT ( 'NONE',  ( -16.78706339993119556, 0.9340140483890039258, 4.934862808901015363 ) ) ;
#30600 = ORIENTED_EDGE ( 'NONE', *, *, #32567, .F. ) ;
#30601 = CARTESIAN_POINT ( 'NONE',  ( -4.394946353583525145, 7.064620221120807564, -1.511227158925545266 ) ) ;
#30602 = EDGE_CURVE ( 'NONE', #34227, #15529, #41620, .T. ) ;
#30603 = ORIENTED_EDGE ( 'NONE', *, *, #12768, .F. ) ;
#30604 = ORIENTED_EDGE ( 'NONE', *, *, #51779, .T. ) ;
#30605 = CARTESIAN_POINT ( 'NONE',  ( -17.74482636761137044, -0.1191753592594197858, 3.674319602356483916 ) ) ;
#30606 = LINE ( 'NONE', #47909, #43908 ) ;
#30607 = LINE ( 'NONE', #47910, #6900 ) ;
#30608 = VERTEX_POINT ( 'NONE', #46417 ) ;
#30609 = DIRECTION ( 'NONE',  ( 0.6427681459581294776, -0.7660444431189769032, 0.005002170337467562802 ) ) ;
#30610 = ORIENTED_EDGE ( 'NONE', *, *, #14473, .T. ) ;
#30611 = EDGE_CURVE ( 'NONE', #50804, #11380, #4679, .T. ) ;
#30612 = LINE ( 'NONE', #13284, #10098 ) ;
#30613 = DIRECTION ( 'NONE',  ( 0.005961354470445682716, -0.6427876096865404731, -0.7660212471507180654 ) ) ;
#30614 = ADVANCED_FACE ( 'NONE', ( #17183 ), #30553, .F. ) ;
#30615 = EDGE_CURVE ( 'NONE', #19873, #20126, #43327, .T. ) ;
#30616 = CARTESIAN_POINT ( 'NONE',  ( -7.860905869600908424, 1.712176620043476140E-14, 2.600000000000000089 ) ) ;
#30617 = AXIS2_PLACEMENT_3D ( 'NONE', #29983, #12940, #4991 ) ;
#30618 = LINE ( 'NONE', #48467, #48549 ) ;
#30619 = DIRECTION ( 'NONE',  ( -0.7660212471507179544, -0.6427876096865405842, -0.005961354470445141482 ) ) ;
#30620 = CARTESIAN_POINT ( 'NONE',  ( -8.944172994845175140, -0.1191753592594181482, 6.328132810502664185 ) ) ;
#30621 = FACE_OUTER_BOUND ( 'NONE', #48857, .T. ) ;
#30622 = DIRECTION ( 'NONE',  ( 0.5449076811759707706, 0.6444004775717708799, -0.5364919789714476250 ) ) ;
#30623 = VERTEX_POINT ( 'NONE', #30810 ) ;
#30624 = CARTESIAN_POINT ( 'NONE',  ( -9.908141408373387193, -0.1191753592594197858, 10.77908512878318703 ) ) ;
#30625 = AXIS2_PLACEMENT_3D ( 'NONE', #22907, #14127, #31721 ) ;
#30626 = DIRECTION ( 'NONE',  ( 0.000000000000000000, -1.000000000000000000, 0.000000000000000000 ) ) ;
#30627 = CARTESIAN_POINT ( 'NONE',  ( -20.54126990917373519, -0.1191753592594197858, 4.760553241521720658 ) ) ;
#30628 = EDGE_CURVE ( 'NONE', #36677, #16658, #13755, .T. ) ;
#30629 = CARTESIAN_POINT ( 'NONE',  ( -14.01701317841955508, 0.000000000000000000, 2.326005055450897085 ) ) ;
#30630 = CARTESIAN_POINT ( 'NONE',  ( -37.22581621634162019, 9.433890025003661250, -4.938189955668043751 ) ) ;
#30631 = DIRECTION ( 'NONE',  ( 0.7660212471507180654, -0.6427876096865404731, 0.005961354470445141482 ) ) ;
#30632 = EDGE_CURVE ( 'NONE', #26534, #9630, #52396, .T. ) ;
#30633 = LINE ( 'NONE', #48787, #23246 ) ;
#30634 = DIRECTION ( 'NONE',  ( 0.005002170337468016433, -0.7660444431189770143, -0.6427681459581293666 ) ) ;
#30635 = EDGE_LOOP ( 'NONE', ( #33092, #25080, #53768, #37690 ) ) ;
#30636 = LINE ( 'NONE', #3378, #24807 ) ;
#30637 = PLANE ( 'NONE',  #5909 ) ;
#30638 = CARTESIAN_POINT ( 'NONE',  ( 2.072287782118878319, 0.000000000000000000, -2.950529333540147015 ) ) ;
#30639 = EDGE_CURVE ( 'NONE', #32268, #46991, #708, .T. ) ;
#30640 = CARTESIAN_POINT ( 'NONE',  ( -11.62415344295244779, 0.000000000000000000, 5.299283401660711768 ) ) ;
#30641 = CARTESIAN_POINT ( 'NONE',  ( 2.072287782118878319, 0.000000000000000000, -2.950529333540147015 ) ) ;
#30642 = CARTESIAN_POINT ( 'NONE',  ( -16.81190032086591302, 0.000000000000000000, 3.212244750653343583 ) ) ;
#30643 = CARTESIAN_POINT ( 'NONE',  ( -10.76248383313556367, -0.1191753592594202577, 1.143333317821924489 ) ) ;
#30644 = ADVANCED_FACE ( 'NONE', ( #43858 ), #8116, .F. ) ;
#30645 = CARTESIAN_POINT ( 'NONE',  ( -12.80458192191714595, 0.000000000000000000, 11.86454056839041726 ) ) ;
#30646 = CARTESIAN_POINT ( 'NONE',  ( -68.58058681874440765, -9.692212885547005996, -6.443496511055998077 ) ) ;
#30647 = ORIENTED_EDGE ( 'NONE', *, *, #24819, .T. ) ;
#30648 = CARTESIAN_POINT ( 'NONE',  ( -9.748361534556408969, 0.000000000000000000, 3.097888829186164816 ) ) ;
#30649 = VERTEX_POINT ( 'NONE', #30253 ) ;
#30650 = ORIENTED_EDGE ( 'NONE', *, *, #18344, .F. ) ;
#30651 = ORIENTED_EDGE ( 'NONE', *, *, #15639, .F. ) ;
#30652 = VERTEX_POINT ( 'NONE', #8685 ) ;
#30653 = EDGE_LOOP ( 'NONE', ( #22792, #3474, #8633, #41326 ) ) ;
#30654 = DIRECTION ( 'NONE',  ( -0.6427681459581293666, -0.7660444431189770143, -0.005002170337467561935 ) ) ;
#30655 = CARTESIAN_POINT ( 'NONE',  ( -11.97318020560097729, 2.391131607591506114, 5.456365251615914680 ) ) ;
#30656 = VECTOR ( 'NONE', #10832, 999.9999999999998863 ) ;
#30657 = EDGE_LOOP ( 'NONE', ( #14518, #4510, #51477, #53442 ) ) ;
#30658 = ORIENTED_EDGE ( 'NONE', *, *, #33957, .T. ) ;
#30659 = EDGE_CURVE ( 'NONE', #53347, #39093, #47566, .T. ) ;
#30660 = EDGE_CURVE ( 'NONE', #51468, #36412, #22301, .T. ) ;
#30661 = CARTESIAN_POINT ( 'NONE',  ( -65.97216590917611256, 4.336808689942016158E-15, -3.251835480715624893 ) ) ;
#30663 = EDGE_CURVE ( 'NONE', #24292, #30130, #55811, .T. ) ;
#30662 = ORIENTED_EDGE ( 'NONE', *, *, #19291, .F. ) ;
#30664 = CARTESIAN_POINT ( 'NONE',  ( -18.32362714986662411, 1.095915999411505082, 5.797425035250995506 ) ) ;
#30665 = CARTESIAN_POINT ( 'NONE',  ( 5.359786524431358501, 0.000000000000000000, -2.456654125669140321 ) ) ;
#30666 = VERTEX_POINT ( 'NONE', #52649 ) ;
#30667 = PLANE ( 'NONE',  #4718 ) ;
#30668 = ADVANCED_FACE ( 'NONE', ( #31073 ), #35095, .F. ) ;
#30669 = EDGE_CURVE ( 'NONE', #37975, #41809, #13495, .T. ) ;
#30670 = EDGE_CURVE ( 'NONE', #6528, #52618, #18028, .T. ) ;
#30671 = ORIENTED_EDGE ( 'NONE', *, *, #31225, .F. ) ;
#30672 = DIRECTION ( 'NONE',  ( 0.6246952433987893460, 0.7422098413412802076, -0.2426528472758539279 ) ) ;
#30673 = LINE ( 'NONE', #12508, #10068 ) ;
#30674 = ORIENTED_EDGE ( 'NONE', *, *, #52054, .T. ) ;
#30675 = DIRECTION ( 'NONE',  ( -0.005002170337468016433, -0.7660444431189770143, 0.6427681459581293666 ) ) ;
#30676 = LINE ( 'NONE', #27509, #2993 ) ;
#30677 = PLANE ( 'NONE',  #50245 ) ;
#30678 = ORIENTED_EDGE ( 'NONE', *, *, #50679, .T. ) ;
#30679 = CARTESIAN_POINT ( 'NONE',  ( -10.74029228357944987, 0.000000000000000000, 11.14194120806293320 ) ) ;
#30680 = ORIENTED_EDGE ( 'NONE', *, *, #40180, .T. ) ;
#30681 = LINE ( 'NONE', #3427, #28290 ) ;
#30682 = CARTESIAN_POINT ( 'NONE',  ( -15.40103151951671734, 0.000000000000000000, 12.95233060667165681 ) ) ;
#30683 = CARTESIAN_POINT ( 'NONE',  ( -17.86442704584935015, 0.000000000000000000, 5.250720149560584638 ) ) ;
#30684 = ADVANCED_FACE ( 'NONE', ( #52102 ), #47860, .F. ) ;
#30685 = DIRECTION ( 'NONE',  ( 0.007781995580012663651, 0.000000000000000000, -0.9999697198139515519 ) ) ;
#30686 = FACE_OUTER_BOUND ( 'NONE', #15988, .T. ) ;
#30687 = CARTESIAN_POINT ( 'NONE',  ( -21.47263955680318404, 0.000000000000000000, 5.022634149262071190 ) ) ;
#30688 = FACE_OUTER_BOUND ( 'NONE', #26192, .T. ) ;
#30689 = EDGE_CURVE ( 'NONE', #32551, #37828, #42729, .T. ) ;
#30690 = DIRECTION ( 'NONE',  ( -0.005002170337468016433, -0.7660444431189770143, 0.6427681459581293666 ) ) ;
#30691 = EDGE_CURVE ( 'NONE', #51521, #39606, #12652, .T. ) ;
#30692 = DIRECTION ( 'NONE',  ( 0.007781995580012663651, 0.000000000000000000, -0.9999697198139515519 ) ) ;
#30693 = EDGE_LOOP ( 'NONE', ( #5239, #8570, #50135, #45564 ) ) ;
#30694 = FACE_OUTER_BOUND ( 'NONE', #41041, .T. ) ;
#30695 = CARTESIAN_POINT ( 'NONE',  ( -22.40634380310664397, 0.000000000000000000, 5.584705972946605534 ) ) ;
#30696 = CARTESIAN_POINT ( 'NONE',  ( -12.05619391717654310, -3.270328918600659218, 6.732133781913477222 ) ) ;
#30697 = EDGE_CURVE ( 'NONE', #3706, #42498, #29967, .T. ) ;
#30698 = VECTOR ( 'NONE', #19271, 1000.000000000000000 ) ;
#30699 = CARTESIAN_POINT ( 'NONE',  ( -23.25534951586139343, 19.16669783366043589, -4.483237922539919929 ) ) ;
#30700 = DIRECTION ( 'NONE',  ( 0.000000000000000000, -1.000000000000000000, 0.000000000000000000 ) ) ;
#30701 = FACE_OUTER_BOUND ( 'NONE', #11102, .T. ) ;
#30702 = ORIENTED_EDGE ( 'NONE', *, *, #28706, .F. ) ;
#30703 = VERTEX_POINT ( 'NONE', #25703 ) ;
#30704 = FACE_OUTER_BOUND ( 'NONE', #34053, .T. ) ;
#30705 = DIRECTION ( 'NONE',  ( -0.5364919789714478471, 0.6444004775717705469, -0.5449076811759709926 ) ) ;
#30706 = ORIENTED_EDGE ( 'NONE', *, *, #34325, .T. ) ;
#30707 = CARTESIAN_POINT ( 'NONE',  ( 2.072287782118878319, 0.000000000000000000, -2.950529333540147015 ) ) ;
#30708 = EDGE_LOOP ( 'NONE', ( #1955, #2881, #3394, #24480 ) ) ;
#30709 = DIRECTION ( 'NONE',  ( 0.5364919789714477361, 0.6444004775717706579, 0.5449076811759711036 ) ) ;
#30710 = ORIENTED_EDGE ( 'NONE', *, *, #1447, .F. ) ;
#30711 = LINE ( 'NONE', #4571, #19312 ) ;
#30712 = EDGE_LOOP ( 'NONE', ( #39137, #53397, #41053, #10821 ) ) ;
#30713 = ORIENTED_EDGE ( 'NONE', *, *, #38444, .F. ) ;
#30714 = VERTEX_POINT ( 'NONE', #27961 ) ;
#30715 =( BOUNDED_CURVE ( )  B_SPLINE_CURVE ( 3, ( #13977, #39561, #4617, #653 ),
 .UNSPECIFIED., .F., .F. ) 
 B_SPLINE_CURVE_WITH_KNOTS ( ( 4, 4 ),
 ( 3.141592653589797113, 3.526448838213318115 ),
 .UNSPECIFIED. ) 
 CURVE ( )  GEOMETRIC_REPRESENTATION_ITEM ( )  RATIONAL_B_SPLINE_CURVE ( ( 1.000000000000000000, 0.9876951826469675400, 0.9876951826469675400, 1.000000000000000000 ) ) 
 REPRESENTATION_ITEM ( '' )  );
#30716 = PLANE ( 'NONE',  #16615 ) ;
#30717 = DIRECTION ( 'NONE',  ( 0.7660212471507180654, -0.6427876096865404731, 0.005961354470445141482 ) ) ;
#30718 = LINE ( 'NONE', #35514, #40247 ) ;
#30719 = LINE ( 'NONE', #27560, #22067 ) ;
#30720 = EDGE_LOOP ( 'NONE', ( #2914, #9711, #7837, #36822 ) ) ;
#30722 = EDGE_LOOP ( 'NONE', ( #30311, #29947, #46186, #44867 ) ) ;
#30721 = EDGE_CURVE ( 'NONE', #14093, #682, #36751, .T. ) ;
#30723 = DIRECTION ( 'NONE',  ( 0.007781995580012663651, 0.000000000000000000, -0.9999697198139515519 ) ) ;
#30724 = EDGE_LOOP ( 'NONE', ( #30148, #22036, #22828, #56004, #46520 ) ) ;
#30725 = LINE ( 'NONE', #51165, #50180 ) ;
#30726 = ORIENTED_EDGE ( 'NONE', *, *, #50461, .T. ) ;
#30727 = CARTESIAN_POINT ( 'NONE',  ( -14.00280974873554030, 0.000000000000000000, 12.40921378708904044 ) ) ;
#30728 = DIRECTION ( 'NONE',  ( -0.005961354470445682716, -0.6427876096865404731, 0.7660212471507180654 ) ) ;
#30729 = EDGE_CURVE ( 'NONE', #9458, #34138, #19128, .T. ) ;
#30730 = EDGE_CURVE ( 'NONE', #19740, #4570, #40156, .T. ) ;
#30731 = EDGE_CURVE ( 'NONE', #38688, #7205, #48397, .T. ) ;
#30732 = AXIS2_PLACEMENT_3D ( 'NONE', #21090, #47212, #17392 ) ;
#30733 = ORIENTED_EDGE ( 'NONE', *, *, #55936, .F. ) ;
#30734 = FACE_OUTER_BOUND ( 'NONE', #3801, .T. ) ;
#30735 = ORIENTED_EDGE ( 'NONE', *, *, #49996, .F. ) ;
#30736 = EDGE_CURVE ( 'NONE', #50295, #7467, #14600, .T. ) ;
#30737 = DIRECTION ( 'NONE',  ( 0.5449076811759707706, 0.6444004775717708799, -0.5364919789714476250 ) ) ;
#30738 = ORIENTED_EDGE ( 'NONE', *, *, #14381, .T. ) ;
#30739 = DIRECTION ( 'NONE',  ( 0.9999697198139515519, 0.000000000000000000, 0.007781995580013368816 ) ) ;
#30740 = DIRECTION ( 'NONE',  ( -0.5364919789714478471, 0.6444004775717705469, -0.5449076811759709926 ) ) ;
#30741 = DIRECTION ( 'NONE',  ( 0.5364919789714477361, 0.6444004775717706579, 0.5449076811759711036 ) ) ;
#30742 = ORIENTED_EDGE ( 'NONE', *, *, #26350, .F. ) ;
#30743 = CARTESIAN_POINT ( 'NONE',  ( -9.024829791847592375, 0.000000000000000000, 3.842183660121707867 ) ) ;
#30744 = CARTESIAN_POINT ( 'NONE',  ( -19.53579455766131900, 0.000000000000000000, 6.884367473930582904 ) ) ;
#30745 = CARTESIAN_POINT ( 'NONE',  ( -68.99096209019747050, 1.598546839610802461, 7.480095325092517733 ) ) ;
#30746 = CARTESIAN_POINT ( 'NONE',  ( -21.47341775636118655, -0.1191753592594197858, 5.122631121243466090 ) ) ;
#30747 = CARTESIAN_POINT ( 'NONE',  ( -13.68556902778486339, 0.000000000000000000, 5.652573058730435918 ) ) ;
#30749 = ADVANCED_FACE ( 'NONE', ( #23416 ), #14049, .F. ) ;
#30748 = CARTESIAN_POINT ( 'NONE',  ( -30.79411802867772607, 0.000000000000000000, 8.643412946479525516 ) ) ;
#30750 = CARTESIAN_POINT ( 'NONE',  ( -15.37130680712323816, 0.000000000000000000, 9.132768899389256845 ) ) ;
#30751 = ORIENTED_EDGE ( 'NONE', *, *, #7377, .F. ) ;
#30752 = FACE_OUTER_BOUND ( 'NONE', #26637, .T. ) ;
#30753 = CARTESIAN_POINT ( 'NONE',  ( -15.32975240366000236, 0.000000000000000000, 3.793117294485577329 ) ) ;
#30754 = ADVANCED_FACE ( 'NONE', ( #27110 ), #6369, .F. ) ;
#30755 = DIRECTION ( 'NONE',  ( -0.5364919789714478471, 0.6444004775717705469, -0.5449076811759709926 ) ) ;
#30756 = ORIENTED_EDGE ( 'NONE', *, *, #12138, .F. ) ;
#30757 = PLANE ( 'NONE',  #44709 ) ;
#30758 = CARTESIAN_POINT ( 'NONE',  ( -21.47341775636118655, -0.1191753592594197858, 5.122631121243466090 ) ) ;
#30759 = ORIENTED_EDGE ( 'NONE', *, *, #49057, .F. ) ;
#30760 = DIRECTION ( 'NONE',  ( 0.007781995580012663651, 0.000000000000000000, -0.9999697198139515519 ) ) ;
#30761 = ADVANCED_FACE ( 'NONE', ( #45264 ), #40734, .F. ) ;
#30762 = CARTESIAN_POINT ( 'NONE',  ( -10.76823194014612639, -0.1191753592594204242, 1.881952724337453642 ) ) ;
#30763 = FACE_OUTER_BOUND ( 'NONE', #51347, .T. ) ;
#30764 = ADVANCED_FACE ( 'NONE', ( #15182 ), #40464, .F. ) ;
#30765 = DIRECTION ( 'NONE',  ( -0.6246952433987894571, 0.7422098413412802076, 0.2426528472758539834 ) ) ;
#30766 = EDGE_LOOP ( 'NONE', ( #32750, #16516, #32799, #37924 ) ) ;
#30767 = ORIENTED_EDGE ( 'NONE', *, *, #23717, .F. ) ;
#30768 = DIRECTION ( 'NONE',  ( -0.5364919789714478471, 0.6444004775717705469, -0.5449076811759709926 ) ) ;
#30769 = CARTESIAN_POINT ( 'NONE',  ( -13.73672976910459909, 0.000000000000000000, 12.22661844811216270 ) ) ;
#30770 = DIRECTION ( 'NONE',  ( 0.000000000000000000, -0.000000000000000000, -1.000000000000000000 ) ) ;
#30771 = DIRECTION ( 'NONE',  ( -0.005961354470445682716, -0.6427876096865404731, 0.7660212471507180654 ) ) ;
#30772 = VECTOR ( 'NONE', #10835, 1000.000000000000227 ) ;
#30773 = PLANE ( 'NONE',  #11974 ) ;
#30774 = CARTESIAN_POINT ( 'NONE',  ( -17.74404816805336793, 0.000000000000000000, 3.574322630375089460 ) ) ;
#30775 = ORIENTED_EDGE ( 'NONE', *, *, #1866, .T. ) ;
#30776 = DIRECTION ( 'NONE',  ( 0.007781995580012663651, -3.146120232559066537E-19, -0.9999697198139514409 ) ) ;
#30777 = DIRECTION ( 'NONE',  ( 0.000000000000000000, 0.000000000000000000, -1.000000000000000000 ) ) ;
#30778 = ORIENTED_EDGE ( 'NONE', *, *, #3670, .T. ) ;
#30779 = DIRECTION ( 'NONE',  ( 0.005961354470445682716, -0.6427876096865404731, -0.7660212471507180654 ) ) ;
#30780 = FACE_OUTER_BOUND ( 'NONE', #22783, .T. ) ;
#30781 = CARTESIAN_POINT ( 'NONE',  ( -11.14312833067548958, 1.419719901456505395, 3.539692811011753371 ) ) ;
#30782 = EDGE_LOOP ( 'NONE', ( #35506, #50542, #32344, #1062 ) ) ;
#30783 = DIRECTION ( 'NONE',  ( -0.9999697198139514409, -0.000000000000000000, -0.007781995580013368816 ) ) ;
#30784 = EDGE_LOOP ( 'NONE', ( #20713, #44262, #46801, #23330 ) ) ;
#30785 = ORIENTED_EDGE ( 'NONE', *, *, #21676, .F. ) ;
#30786 = EDGE_LOOP ( 'NONE', ( #49543, #8051, #44567, #55614 ) ) ;
#30787 = VERTEX_POINT ( 'NONE', #18587 ) ;
#30788 = DIRECTION ( 'NONE',  ( 0.000000000000000000, -0.000000000000000000, -1.000000000000000000 ) ) ;
#30789 = ORIENTED_EDGE ( 'NONE', *, *, #33380, .T. ) ;
#30790 = DIRECTION ( 'NONE',  ( 0.6427681459581294776, -0.7660444431189769032, 0.005002170337467562802 ) ) ;
#30791 = EDGE_CURVE ( 'NONE', #34450, #25142, #42156, .T. ) ;
#30792 = ORIENTED_EDGE ( 'NONE', *, *, #26141, .F. ) ;
#30793 = CARTESIAN_POINT ( 'NONE',  ( -14.13715331148882015, 0.000000000000000000, 3.971724389968579239 ) ) ;
#30794 = EDGE_LOOP ( 'NONE', ( #12458, #8827, #47382, #20360 ) ) ;
#30795 = DIRECTION ( 'NONE',  ( 0.005961354470445682716, -0.6427876096865404731, -0.7660212471507180654 ) ) ;
#30796 = ORIENTED_EDGE ( 'NONE', *, *, #14851, .T. ) ;
#30797 = ADVANCED_FACE ( 'NONE', ( #53254 ), #10059, .F. ) ;
#30798 = ADVANCED_FACE ( 'NONE', ( #9807 ), #39883, .F. ) ;
#30799 = FACE_OUTER_BOUND ( 'NONE', #48283, .T. ) ;
#30800 = DIRECTION ( 'NONE',  ( 0.5364919789714477361, 0.6444004775717706579, 0.5449076811759711036 ) ) ;
#30801 = CARTESIAN_POINT ( 'NONE',  ( -8.580311269543482666, 0.000000000000000000, 6.430967494694069586 ) ) ;
#30802 = LINE ( 'NONE', #48102, #47763 ) ;
#30803 = DIRECTION ( 'NONE',  ( -0.5449076811759708816, 0.6444004775717707689, 0.5364919789714475140 ) ) ;
#30804 = ORIENTED_EDGE ( 'NONE', *, *, #4935, .F. ) ;
#30805 = EDGE_LOOP ( 'NONE', ( #34185, #41718, #33484, #39534 ) ) ;
#30806 = CARTESIAN_POINT ( 'NONE',  ( -14.94760462649100496, 0.000000000000000000, 2.488088991209854051 ) ) ;
#30807 = LINE ( 'NONE', #56095, #3089 ) ;
#30808 = PLANE ( 'NONE',  #36941 ) ;
#30809 = FACE_OUTER_BOUND ( 'NONE', #26514, .T. ) ;
#30810 = CARTESIAN_POINT ( 'NONE',  ( -12.28147977762975707, 0.000000000000000000, 4.355497740298383214 ) ) ;
#30811 = LINE ( 'NONE', #47861, #36850 ) ;
#30812 = ORIENTED_EDGE ( 'NONE', *, *, #39955, .T. ) ;
#30813 = DIRECTION ( 'NONE',  ( 0.7660212471507180654, -0.6427876096865404731, 0.005961354470445141482 ) ) ;
#30814 = CARTESIAN_POINT ( 'NONE',  ( -30.79489622823572859, -0.1191753592594197858, 8.743409918460921304 ) ) ;
#30815 = ORIENTED_EDGE ( 'NONE', *, *, #45443, .F. ) ;
#30816 = CARTESIAN_POINT ( 'NONE',  ( -68.71918076694248612, -8.969740930377138710, 6.949370683160943862 ) ) ;
#30817 = DIRECTION ( 'NONE',  ( 0.000000000000000000, -1.000000000000000000, 0.000000000000000000 ) ) ;
#30818 = LINE ( 'NONE', #35636, #43181 ) ;
#30819 = ADVANCED_FACE ( 'NONE', ( #2075 ), #19411, .F. ) ;
#30820 = LINE ( 'NONE', #38796, #536 ) ;
#30821 = LINE ( 'NONE', #48124, #27425 ) ;
#30822 = ORIENTED_EDGE ( 'NONE', *, *, #46673, .T. ) ;
#30823 = EDGE_CURVE ( 'NONE', #15750, #13531, #49538, .T. ) ;
#30824 = EDGE_LOOP ( 'NONE', ( #53191, #43222, #29085, #11244, #30021, #42061, #50175, #5486, #18396, #18830, #51454, #27426, #14104, #22733, #42355, #31215 ) ) ;
#30825 = CARTESIAN_POINT ( 'NONE',  ( -15.61159646202592199, 2.876837460659008361, 2.654219792496569141 ) ) ;
#30826 = DIRECTION ( 'NONE',  ( 0.007781995580012663651, -3.146120232559066537E-19, -0.9999697198139514409 ) ) ;
#30827 = CARTESIAN_POINT ( 'NONE',  ( -22.40556560354864146, -0.1191753592594197858, 5.484709000965211523 ) ) ;
#30828 = DIRECTION ( 'NONE',  ( -0.9999697198139514409, -0.000000000000000000, -0.007781995580013368816 ) ) ;
#30829 = ADVANCED_FACE ( 'NONE', ( #36198 ), #53501, .F. ) ;
#30830 = DIRECTION ( 'NONE',  ( 0.007781995580012663651, 0.000000000000000000, -0.9999697198139515519 ) ) ;
#30831 = CARTESIAN_POINT ( 'NONE',  ( -13.93438848177649092, 24.61325290493446616, -3.678420148561327707 ) ) ;
#30832 = FACE_OUTER_BOUND ( 'NONE', #33981, .T. ) ;
#30833 = LINE ( 'NONE', #30581, #4210 ) ;
#30834 = FACE_OUTER_BOUND ( 'NONE', #22961, .T. ) ;
#30835 = ORIENTED_EDGE ( 'NONE', *, *, #21938, .T. ) ;
#30836 = DIRECTION ( 'NONE',  ( -0.5449076811759708816, 0.6444004775717707689, 0.5364919789714475140 ) ) ;
#30837 = ORIENTED_EDGE ( 'NONE', *, *, #44150, .F. ) ;
#30838 = CARTESIAN_POINT ( 'NONE',  ( -19.59569683186026268, 0.000000000000000000, 14.58168106541950948 ) ) ;
#30839 = DIRECTION ( 'NONE',  ( -0.005002170337468016433, -0.7660444431189770143, 0.6427681459581293666 ) ) ;
#30840 = ORIENTED_EDGE ( 'NONE', *, *, #10270, .F. ) ;
#30841 = ORIENTED_EDGE ( 'NONE', *, *, #36719, .T. ) ;
#30842 = ORIENTED_EDGE ( 'NONE', *, *, #32582, .F. ) ;
#30843 = ORIENTED_EDGE ( 'NONE', *, *, #25514, .F. ) ;
#30844 = VERTEX_POINT ( 'NONE', #45003 ) ;
#30845 = ORIENTED_EDGE ( 'NONE', *, *, #50850, .T. ) ;
#30846 = LINE ( 'NONE', #21199, #39492 ) ;
#30847 = LINE ( 'NONE', #43614, #32037 ) ;
#30848 = EDGE_CURVE ( 'NONE', #25456, #9641, #11733, .T. ) ;
#30849 = DIRECTION ( 'NONE',  ( -0.005961354470445682716, -0.6427876096865404731, 0.7660212471507180654 ) ) ;
#30850 = ORIENTED_EDGE ( 'NONE', *, *, #48874, .F. ) ;
#30851 = CARTESIAN_POINT ( 'NONE',  ( -11.67244013076689946, 0.000000000000000000, 11.50401908778467863 ) ) ;
#30852 = EDGE_LOOP ( 'NONE', ( #40991, #47965, #3596, #25682, #27417, #6348, #17227, #17948 ) ) ;
#30853 = ORIENTED_EDGE ( 'NONE', *, *, #25529, .F. ) ;
#30854 = ADVANCED_FACE ( 'NONE', ( #16011 ), #42111, .F. ) ;
#30855 = CARTESIAN_POINT ( 'NONE',  ( -10.80272058220951870, -0.1191753592594185784, 6.313669163430627229 ) ) ;
#30856 = PLANE ( 'NONE',  #20348 ) ;
#30857 = CARTESIAN_POINT ( 'NONE',  ( -18.59502454995801912, 0.000000000000000000, 5.414360484435545295 ) ) ;
#30858 = ORIENTED_EDGE ( 'NONE', *, *, #50821, .F. ) ;
#30859 = DIRECTION ( 'NONE',  ( 0.000000000000000000, -0.000000000000000000, -1.000000000000000000 ) ) ;
#30860 = ORIENTED_EDGE ( 'NONE', *, *, #43720, .T. ) ;
#30861 = CARTESIAN_POINT ( 'NONE',  ( -17.55053657858433169, -3.756034771668162797, 3.578708368817510532 ) ) ;
#30862 = FACE_OUTER_BOUND ( 'NONE', #21535, .T. ) ;
#30863 = ADVANCED_FACE ( 'NONE', ( #33040 ), #6639, .F. ) ;
#30864 = VECTOR ( 'NONE', #12079, 999.9999999999998863 ) ;
#30865 = LINE ( 'NONE', #1028, #14248 ) ;
#30866 = FACE_OUTER_BOUND ( 'NONE', #37969, .T. ) ;
#30867 = CARTESIAN_POINT ( 'NONE',  ( -20.06177075545399191, 0.000000000000000000, 14.76272000528038220 ) ) ;
#30868 = CARTESIAN_POINT ( 'NONE',  ( 5.283022392374841836, -1.075897820612792044, -2.393286648641791636 ) ) ;
#30869 = DIRECTION ( 'NONE',  ( 0.005002170337468016433, -0.7660444431189770143, -0.6427681459581293666 ) ) ;
#30870 = PLANE ( 'NONE',  #21346 ) ;
#30871 = EDGE_LOOP ( 'NONE', ( #31961, #25212, #51009, #44877 ) ) ;
#30872 = CARTESIAN_POINT ( 'NONE',  ( -12.60458797795435615, 0.000000000000000000, 11.86609696750642229 ) ) ;
#30873 = LINE ( 'NONE', #36015, #22909 ) ;
#30874 = DIRECTION ( 'NONE',  ( 0.005002170337468016433, -0.7660444431189770143, -0.6427681459581293666 ) ) ;
#30875 = LINE ( 'NONE', #26086, #53523 ) ;
#30876 = CARTESIAN_POINT ( 'NONE',  ( -18.83741502687287905, 20.05043840171031633, -4.259863338787211795 ) ) ;
#30877 = PLANE ( 'NONE',  #43139 ) ;
#30878 = FACE_OUTER_BOUND ( 'NONE', #51845, .T. ) ;
#30879 = DIRECTION ( 'NONE',  ( -0.005002170337468016433, -0.7660444431189770143, 0.6427681459581293666 ) ) ;
#30880 = EDGE_LOOP ( 'NONE', ( #13415, #17730, #16237, #34181 ) ) ;
#30881 = DIRECTION ( 'NONE',  ( -0.005002170337468016433, -0.7660444431189770143, 0.6427681459581293666 ) ) ;
#30882 = CARTESIAN_POINT ( 'NONE',  ( -18.67619601524082285, 0.000000000000000000, 3.936400510096834893 ) ) ;
#30883 = FACE_OUTER_BOUND ( 'NONE', #30127, .T. ) ;
#30884 = LINE ( 'NONE', #38866, #49077 ) ;
#30885 = EDGE_CURVE ( 'NONE', #53603, #11768, #41819, .T. ) ;
#30886 = CARTESIAN_POINT ( 'NONE',  ( -30.79567442779373110, 0.000000000000000000, 8.843406890442315316 ) ) ;
#30887 = PLANE ( 'NONE',  #32287 ) ;
#30888 = LINE ( 'NONE', #9617, #42829 ) ;
#30889 = CARTESIAN_POINT ( 'NONE',  ( -69.43561177275644525, -9.791245164465275153, -7.501782499249458169 ) ) ;
#30890 = DIRECTION ( 'NONE',  ( 0.005961354470445682716, -0.6427876096865404731, -0.7660212471507180654 ) ) ;
#30891 = EDGE_CURVE ( 'NONE', #21366, #36639, #20550, .T. ) ;
#30892 = ORIENTED_EDGE ( 'NONE', *, *, #55208, .T. ) ;
#30893 = VECTOR ( 'NONE', #9071, 1000.000000000000114 ) ;
#30894 = EDGE_CURVE ( 'NONE', #345, #51439, #11469, .T. ) ;
#30895 = EDGE_CURVE ( 'NONE', #29778, #22415, #10896, .T. ) ;
#30896 = AXIS2_PLACEMENT_3D ( 'NONE', #35296, #906, #18514 ) ;
#30897 = ORIENTED_EDGE ( 'NONE', *, *, #52635, .T. ) ;
#30898 = ORIENTED_EDGE ( 'NONE', *, *, #45389, .T. ) ;
#30899 = ORIENTED_EDGE ( 'NONE', *, *, #25193, .T. ) ;
#30900 = VERTEX_POINT ( 'NONE', #50900 ) ;
#30901 = DIRECTION ( 'NONE',  ( -0.005002170337468016433, -0.7660444431189770143, 0.6427681459581293666 ) ) ;
#30902 = EDGE_CURVE ( 'NONE', #39497, #44937, #37031, .T. ) ;
#30903 = CARTESIAN_POINT ( 'NONE',  ( -50.02554558092695913, 3.776013638374817294, -5.000000000000000000 ) ) ;
#30905 = EDGE_CURVE ( 'NONE', #1854, #53450, #15701, .T. ) ;
#30904 = EDGE_LOOP ( 'NONE', ( #4933, #51403, #18928, #22489 ) ) ;
#30906 = ORIENTED_EDGE ( 'NONE', *, *, #32410, .T. ) ;
#30907 = EDGE_CURVE ( 'NONE', #22464, #49826, #24501, .T. ) ;
#30908 = CARTESIAN_POINT ( 'NONE',  ( -67.45300034126424293, 4.561518438557346199E-46, -6.901381173728422525 ) ) ;
#30909 = ORIENTED_EDGE ( 'NONE', *, *, #1471, .F. ) ;
#30910 = CARTESIAN_POINT ( 'NONE',  ( -8.571689109027634146, 0.000000000000000000, 5.323038384920776522 ) ) ;
#30911 = DIRECTION ( 'NONE',  ( -0.005961354470445682716, -0.6427876096865404731, 0.7660212471507180654 ) ) ;
#30912 = ORIENTED_EDGE ( 'NONE', *, *, #48807, .F. ) ;
#30913 = DIRECTION ( 'NONE',  ( 0.000000000000000000, -0.000000000000000000, -1.000000000000000000 ) ) ;
#30914 = ADVANCED_FACE ( 'NONE', ( #32500 ), #2909, .F. ) ;
#30915 = VERTEX_POINT ( 'NONE', #33588 ) ;
#30916 = AXIS2_PLACEMENT_3D ( 'NONE', #20986, #16740, #34351 ) ;
#30917 = PLANE ( 'NONE',  #30075 ) ;
#30918 = PLANE ( 'NONE',  #9334 ) ;
#30919 = ADVANCED_FACE ( 'NONE', ( #32745 ), #55179, .F. ) ;
#30920 = DIRECTION ( 'NONE',  ( -0.9999697198139514409, -0.000000000000000000, -0.007781995580013368816 ) ) ;
#30921 = DIRECTION ( 'NONE',  ( -0.005002170337468016433, -0.7660444431189770143, 0.6427681459581293666 ) ) ;
#30922 = VERTEX_POINT ( 'NONE', #37576 ) ;
#30923 = CARTESIAN_POINT ( 'NONE',  ( -14.20280369269832832, 0.000000000000000000, 12.40765738797303719 ) ) ;
#30924 = CARTESIAN_POINT ( 'NONE',  ( -16.03461999353783440, 0.000000000000000000, 8.958280829210268692 ) ) ;
#30925 = LINE ( 'NONE', #18733, #1240 ) ;
#30926 = ORIENTED_EDGE ( 'NONE', *, *, #39477, .F. ) ;
#30927 = DIRECTION ( 'NONE',  ( 0.007781995580012663651, 0.000000000000000000, -0.9999697198139515519 ) ) ;
#30928 = ORIENTED_EDGE ( 'NONE', *, *, #24306, .T. ) ;
#30929 = VECTOR ( 'NONE', #41670, 999.9999999999998863 ) ;
#30930 = DIRECTION ( 'NONE',  ( 0.005002170337468016433, -0.7660444431189770143, -0.6427681459581293666 ) ) ;
#30931 = CARTESIAN_POINT ( 'NONE',  ( -8.704836502503972895, 0.000000000000000000, 4.583338061504010241 ) ) ;
#30932 = LINE ( 'NONE', #39173, #10455 ) ;
#30933 = CARTESIAN_POINT ( 'NONE',  ( -17.26532721389163072, 0.000000000000000000, 13.67648636611514590 ) ) ;
#30934 = CARTESIAN_POINT ( 'NONE',  ( -69.66297551618575312, -8.676591480033549075, 7.503902134509970345 ) ) ;
#30935 = DIRECTION ( 'NONE',  ( -0.6246952433987894571, 0.7422098413412802076, 0.2426528472758539834 ) ) ;
#30936 = LINE ( 'NONE', #48553, #42480 ) ;
#30937 = VECTOR ( 'NONE', #10146, 999.9999999999998863 ) ;
#30938 = DIRECTION ( 'NONE',  ( 0.007781995580012663651, 0.000000000000000000, -0.9999697198139515519 ) ) ;
#30939 = LINE ( 'NONE', #268, #15997 ) ;
#30940 = ORIENTED_EDGE ( 'NONE', *, *, #2447, .T. ) ;
#30941 = LINE ( 'NONE', #48251, #4866 ) ;
#30942 = DIRECTION ( 'NONE',  ( -0.6427681459581293666, -0.7660444431189770143, -0.005002170337467561935 ) ) ;
#30943 = CARTESIAN_POINT ( 'NONE',  ( -12.56492345065575122, 0.000000000000000000, 6.769290391155751152 ) ) ;
#30944 = DIRECTION ( 'NONE',  ( 0.5449076811759707706, 0.6444004775717708799, -0.5364919789714476250 ) ) ;
#30945 = EDGE_CURVE ( 'NONE', #7012, #15750, #33336, .T. ) ;
#30946 = PLANE ( 'NONE',  #35093 ) ;
#30947 = DIRECTION ( 'NONE',  ( 0.9999697198139515519, 0.000000000000000000, 0.007781995580013368816 ) ) ;
#30948 = ORIENTED_EDGE ( 'NONE', *, *, #3499, .F. ) ;
#30949 = ORIENTED_EDGE ( 'NONE', *, *, #12536, .F. ) ;
#30950 = LINE ( 'NONE', #17625, #48579 ) ;
#30951 = DIRECTION ( 'NONE',  ( 0.9999697198139515519, 0.000000000000000000, 0.007781995580013368816 ) ) ;
#30952 = EDGE_CURVE ( 'NONE', #22163, #6183, #28210, .T. ) ;
#30953 = VECTOR ( 'NONE', #12164, 999.9999999999998863 ) ;
#30954 = VECTOR ( 'NONE', #43093, 1000.000000000000227 ) ;
#30955 = VERTEX_POINT ( 'NONE', #42411 ) ;
#30956 = DIRECTION ( 'NONE',  ( 0.6427681459581294776, -0.7660444431189769032, 0.005002170337467562802 ) ) ;
#30957 = VERTEX_POINT ( 'NONE', #3503 ) ;
#30958 = DIRECTION ( 'NONE',  ( 0.5364919789714477361, 0.6444004775717706579, 0.5449076811759711036 ) ) ;
#30959 = EDGE_CURVE ( 'NONE', #19103, #44937, #11167, .T. ) ;
#30960 = VERTEX_POINT ( 'NONE', #45521 ) ;
#30961 = VERTEX_POINT ( 'NONE', #24790 ) ;
#30962 = VERTEX_POINT ( 'NONE', #50641 ) ;
#30963 = CARTESIAN_POINT ( 'NONE',  ( -12.54269775668131714, 2.553033558614008047, 1.472486354876782810 ) ) ;
#30964 = CARTESIAN_POINT ( 'NONE',  ( -12.54193102261348969, 0.000000000000000000, 3.814812765093635871 ) ) ;
#30965 = CARTESIAN_POINT ( 'NONE',  ( -14.14158376411010387, 0.000000000000000000, 4.541028037189134281 ) ) ;
#30966 = LINE ( 'NONE', #9967, #33005 ) ;
#30967 = EDGE_CURVE ( 'NONE', #42922, #50620, #23954, .T. ) ;
#30968 = ORIENTED_EDGE ( 'NONE', *, *, #13028, .F. ) ;
#30969 = ORIENTED_EDGE ( 'NONE', *, *, #8740, .T. ) ;
#30970 = VECTOR ( 'NONE', #46261, 1000.000000000000227 ) ;
#30971 = EDGE_CURVE ( 'NONE', #39202, #12878, #343, .T. ) ;
#30972 = DIRECTION ( 'NONE',  ( 0.005002170337468016433, -0.7660444431189770143, -0.6427681459581293666 ) ) ;
#30973 = ORIENTED_EDGE ( 'NONE', *, *, #18086, .F. ) ;
#30974 = LINE ( 'NONE', #9406, #30059 ) ;
#30975 = ORIENTED_EDGE ( 'NONE', *, *, #43733, .T. ) ;
#30976 = DIRECTION ( 'NONE',  ( -0.6427681459581293666, -0.7660444431189770143, -0.005002170337467561935 ) ) ;
#30977 = DIRECTION ( 'NONE',  ( -0.005961354470445682716, -0.6427876096865404731, 0.7660212471507180654 ) ) ;
#30978 = EDGE_CURVE ( 'NONE', #13435, #19083, #17126, .T. ) ;
#30979 = ORIENTED_EDGE ( 'NONE', *, *, #22007, .F. ) ;
#30980 = CARTESIAN_POINT ( 'NONE',  ( -25.20123094555300369, 0.000000000000000000, 6.470945668149052032 ) ) ;
#30981 = EDGE_LOOP ( 'NONE', ( #9782, #11197, #24829 ) ) ;
#30982 = FACE_OUTER_BOUND ( 'NONE', #54170, .T. ) ;
#30983 = ORIENTED_EDGE ( 'NONE', *, *, #52628, .T. ) ;
#30984 = LINE ( 'NONE', #48303, #1355 ) ;
#30985 = LINE ( 'NONE', #887, #43849 ) ;
#30986 = LINE ( 'NONE', #25926, #27349 ) ;
#30987 = VERTEX_POINT ( 'NONE', #12310 ) ;
#30989 = DIRECTION ( 'NONE',  ( 0.7660212471507180654, -0.6427876096865404731, 0.005961354470445141482 ) ) ;
#30988 = VECTOR ( 'NONE', #6455, 1000.000000000000227 ) ;
#30990 = VECTOR ( 'NONE', #20225, 1000.000000000000227 ) ;
#30991 = FACE_OUTER_BOUND ( 'NONE', #14189, .T. ) ;
#30992 = DIRECTION ( 'NONE',  ( 0.000000000000000000, -0.000000000000000000, -1.000000000000000000 ) ) ;
#30993 = CARTESIAN_POINT ( 'NONE',  ( 2.072287782118878319, 0.000000000000000000, -2.950529333540147015 ) ) ;
#30994 = PLANE ( 'NONE',  #55774 ) ;
#30995 = DIRECTION ( 'NONE',  ( -0.005002170337468016433, -0.7660444431189770143, 0.6427681459581293666 ) ) ;
#30996 = PLANE ( 'NONE',  #9527 ) ;
#30997 = AXIS2_PLACEMENT_3D ( 'NONE', #18313, #9828, #40184 ) ;
#30998 = EDGE_LOOP ( 'NONE', ( #44812, #44518, #19990, #32670 ) ) ;
#30999 = DIRECTION ( 'NONE',  ( -0.9321478471874540261, 0.000000000000000000, 0.3620778797217457656 ) ) ;
#31000 = PLANE ( 'NONE',  #43144 ) ;
#31001 = DIRECTION ( 'NONE',  ( -0.6427681459581293666, -0.7660444431189770143, -0.005002170337467561935 ) ) ;
#31002 = ORIENTED_EDGE ( 'NONE', *, *, #34843, .T. ) ;
#31003 = LINE ( 'NONE', #43514, #40173 ) ;
#31004 = DIRECTION ( 'NONE',  ( 0.9999697198139515519, 0.000000000000000000, 0.007781995580013368816 ) ) ;
#31005 = ORIENTED_EDGE ( 'NONE', *, *, #25278, .F. ) ;
#31006 = ADVANCED_FACE ( 'NONE', ( #12590 ), #9149, .F. ) ;
#31007 = DIRECTION ( 'NONE',  ( 0.007781995580012663651, -3.146120232559066537E-19, -0.9999697198139514409 ) ) ;
#31008 = DIRECTION ( 'NONE',  ( 0.5449076811759707706, 0.6444004775717708799, -0.5364919789714476250 ) ) ;
#31009 = AXIS2_PLACEMENT_3D ( 'NONE', #40285, #13873, #18133 ) ;
#31010 = ADVANCED_FACE ( 'NONE', ( #42955 ), #4899, .F. ) ;
#31011 = LINE ( 'NONE', #9444, #49554 ) ;
#31012 = AXIS2_PLACEMENT_3D ( 'NONE', #18571, #14868, #52924 ) ;
#31013 = CARTESIAN_POINT ( 'NONE',  ( -15.88130887279446490, 0.000000000000000000, 3.050160814894388839 ) ) ;
#31014 = ORIENTED_EDGE ( 'NONE', *, *, #19743, .F. ) ;
#31015 = ORIENTED_EDGE ( 'NONE', *, *, #173, .T. ) ;
#31016 = ADVANCED_FACE ( 'NONE', ( #49 ), #4362, .F. ) ;
#31017 = DIRECTION ( 'NONE',  ( 0.5364919789714477361, 0.6444004775717706579, 0.5449076811759711036 ) ) ;
#31018 = DIRECTION ( 'NONE',  ( 0.7660212471507180654, -0.6427876096865404731, 0.005961354470445141482 ) ) ;
#31019 = CARTESIAN_POINT ( 'NONE',  ( -9.766923509977383233, 0.000000000000000000, 5.483062808027726831 ) ) ;
#31020 = ADVANCED_FACE ( 'NONE', ( #34437 ), #46951, .F. ) ;
#31021 = ADVANCED_FACE ( 'NONE', ( #30481 ), #43783, .F. ) ;
#31022 = EDGE_CURVE ( 'NONE', #33706, #48284, #26463, .T. ) ;
#31023 = CARTESIAN_POINT ( 'NONE',  ( -21.47263955680318404, 0.000000000000000000, 5.022634149262071190 ) ) ;
#31024 = CARTESIAN_POINT ( 'NONE',  ( -17.96341130604493941, 4.010151117816511679, 3.531585906670110742 ) ) ;
#31025 = LINE ( 'NONE', #39004, #16737 ) ;
#31026 = ORIENTED_EDGE ( 'NONE', *, *, #46881, .F. ) ;
#31027 = DIRECTION ( 'NONE',  ( -0.7660212471507179544, -0.6427876096865405842, -0.005961354470445141482 ) ) ;
#31028 = DIRECTION ( 'NONE',  ( 0.007781995580012663651, 0.000000000000000000, -0.9999697198139515519 ) ) ;
#31029 = VERTEX_POINT ( 'NONE', #17684 ) ;
#31030 = DIRECTION ( 'NONE',  ( 0.6427681459581294776, -0.7660444431189769032, 0.005002170337467562802 ) ) ;
#31031 = VECTOR ( 'NONE', #19841, 999.9999999999998863 ) ;
#31032 = FACE_OUTER_BOUND ( 'NONE', #52143, .T. ) ;
#31033 = LINE ( 'NONE', #48663, #17548 ) ;
#31034 = VERTEX_POINT ( 'NONE', #8609 ) ;
#31035 = AXIS2_PLACEMENT_3D ( 'NONE', #7489, #12023, #50080 ) ;
#31036 = VECTOR ( 'NONE', #1390, 999.9999999999998863 ) ;
#31037 = PLANE ( 'NONE',  #54768 ) ;
#31038 = EDGE_CURVE ( 'NONE', #54725, #54555, #47800, .T. ) ;
#31039 = ORIENTED_EDGE ( 'NONE', *, *, #16396, .F. ) ;
#31041 = ORIENTED_EDGE ( 'NONE', *, *, #51080, .F. ) ;
#31040 = EDGE_CURVE ( 'NONE', #21773, #2815, #38983, .T. ) ;
#31042 = VECTOR ( 'NONE', #26942, 999.9999999999998863 ) ;
#31043 = ORIENTED_EDGE ( 'NONE', *, *, #20352, .T. ) ;
#31044 = VECTOR ( 'NONE', #29561, 1000.000000000000227 ) ;
#31045 = EDGE_CURVE ( 'NONE', #44182, #5782, #34713, .T. ) ;
#31046 = VERTEX_POINT ( 'NONE', #13148 ) ;
#31047 = CARTESIAN_POINT ( 'NONE',  ( -69.53087401356451380, -8.661442845389931477, -7.341494710781373279 ) ) ;
#31048 = ORIENTED_EDGE ( 'NONE', *, *, #34700, .T. ) ;
#31049 = CARTESIAN_POINT ( 'NONE',  ( -14.82067173329432563, 1.905425754524005200, 5.765301610339943039 ) ) ;
#31050 = CARTESIAN_POINT ( 'NONE',  ( -14.56888064431065821, -0.1191753592594197858, 12.58947452739191064 ) ) ;
#31051 = EDGE_CURVE ( 'NONE', #32191, #48518, #50372, .T. ) ;
#31052 = ORIENTED_EDGE ( 'NONE', *, *, #49383, .T. ) ;
#31053 = DIRECTION ( 'NONE',  ( -0.7886751345948130876, 0.2113248654051844977, -0.5773502691896263972 ) ) ;
#31054 = EDGE_LOOP ( 'NONE', ( #23306, #3137, #13497, #28175 ) ) ;
#31056 = VECTOR ( 'NONE', #54323, 1000.000000000000227 ) ;
#31055 = DIRECTION ( 'NONE',  ( 0.6427681459581294776, -0.7660444431189769032, 0.005002170337467562802 ) ) ;
#31057 = ORIENTED_EDGE ( 'NONE', *, *, #52829, .F. ) ;
#31058 = ADVANCED_FACE ( 'NONE', ( #21926 ), #35024, .F. ) ;
#31059 = CARTESIAN_POINT ( 'NONE',  ( -17.74404816805336793, 0.000000000000000000, 3.574322630375089460 ) ) ;
#31060 = LINE ( 'NONE', #49219, #52870 ) ;
#31061 = DIRECTION ( 'NONE',  ( -0.005002170337468016433, -0.7660444431189770143, 0.6427681459581293666 ) ) ;
#31062 = DIRECTION ( 'NONE',  ( -1.000000000000000000, -0.000000000000000000, -0.000000000000000000 ) ) ;
#31063 = CARTESIAN_POINT ( 'NONE',  ( -17.23833534428622372, 2.553033558614007603, 7.767238996852877442 ) ) ;
#31064 = PLANE ( 'NONE',  #13832 ) ;
#31065 = EDGE_LOOP ( 'NONE', ( #11186, #10767, #12966, #3705 ) ) ;
#31066 = ORIENTED_EDGE ( 'NONE', *, *, #13350, .T. ) ;
#31067 = CARTESIAN_POINT ( 'NONE',  ( -12.98834176436399623, -3.270328918600660995, 7.094211661635224431 ) ) ;
#31068 = LINE ( 'NONE', #9504, #10370 ) ;
#31069 = AXIS2_PLACEMENT_3D ( 'NONE', #13765, #976, #31932 ) ;
#31070 = CARTESIAN_POINT ( 'NONE',  ( -19.76861662533108799, -0.8417996532631553119, 5.742270417481394773 ) ) ;
#31071 = CARTESIAN_POINT ( 'NONE',  ( -16.01294521988485542, 0.000000000000000000, 6.173118962443128410 ) ) ;
#31072 = ORIENTED_EDGE ( 'NONE', *, *, #53852, .T. ) ;
#31073 = FACE_OUTER_BOUND ( 'NONE', #9728, .T. ) ;
#31074 = LINE ( 'NONE', #48965, #54056 ) ;
#31075 = ORIENTED_EDGE ( 'NONE', *, *, #45570, .F. ) ;
#31077 = CARTESIAN_POINT ( 'NONE',  ( -25.83279121425626812, 17.74370688441070953, -4.657437592157546824 ) ) ;
#31076 = VECTOR ( 'NONE', #52382, 1000.000000000000114 ) ;
#31078 = CARTESIAN_POINT ( 'NONE',  ( -19.23669273636768295, -2.946525016555658905, 8.989866006152718469 ) ) ;
#31079 = ORIENTED_EDGE ( 'NONE', *, *, #29011, .F. ) ;
#31080 = VECTOR ( 'NONE', #7281, 1000.000000000000227 ) ;
#31081 = VECTOR ( 'NONE', #34502, 1000.000000000000227 ) ;
#31082 = CARTESIAN_POINT ( 'NONE',  ( -9.542064456761055524, 0.000000000000000000, 10.59726798936431180 ) ) ;
#31083 = DIRECTION ( 'NONE',  ( 0.9999697198139515519, 0.000000000000000000, 0.007781995580013368816 ) ) ;
#31084 = DIRECTION ( 'NONE',  ( -0.5364919789714478471, 0.6444004775717705469, -0.5449076811759709926 ) ) ;
#31085 = CARTESIAN_POINT ( 'NONE',  ( -9.971347906561460306, 0.000000000000000000, 6.050810056132276848 ) ) ;
#31086 = CARTESIAN_POINT ( 'NONE',  ( -19.60912206198628027, -0.1191753592594197858, 4.398475361799976113 ) ) ;
#31087 = VERTEX_POINT ( 'NONE', #30753 ) ;
#31088 = VECTOR ( 'NONE', #14089, 999.9999999999998863 ) ;
#31089 = VECTOR ( 'NONE', #20939, 999.9999999999998863 ) ;
#31090 = ORIENTED_EDGE ( 'NONE', *, *, #46792, .T. ) ;
#31091 = DIRECTION ( 'NONE',  ( 0.9999697198139515519, 0.000000000000000000, 0.007781995580013368816 ) ) ;
#31092 = DIRECTION ( 'NONE',  ( 0.007781995580012663651, -3.146120232559066537E-19, -0.9999697198139514409 ) ) ;
#31093 = LINE ( 'NONE', #13238, #39689 ) ;
#31094 = EDGE_CURVE ( 'NONE', #15067, #9201, #33877, .T. ) ;
#31095 = ADVANCED_FACE ( 'NONE', ( #8053 ), #25364, .F. ) ;
#31096 = CARTESIAN_POINT ( 'NONE',  ( -15.14133055664494520, -3.108426967578160838, 2.663553012464920933 ) ) ;
#31097 = VECTOR ( 'NONE', #30093, 999.9999999999998863 ) ;
#31098 = CARTESIAN_POINT ( 'NONE',  ( -11.67244013076689946, 0.000000000000000000, 11.50401908778467863 ) ) ;
#31100 = EDGE_CURVE ( 'NONE', #18224, #11899, #14285, .T. ) ;
#31099 = EDGE_LOOP ( 'NONE', ( #55669, #1984, #52073, #44455 ) ) ;
#31102 = VECTOR ( 'NONE', #13406, 999.9999999999998863 ) ;
#31101 = CARTESIAN_POINT ( 'NONE',  ( -12.08016817927768827, 0.000000000000000000, 4.187738380119410131 ) ) ;
#31103 = CARTESIAN_POINT ( 'NONE',  ( -9.046265820773848887, 0.000000000000000000, 6.596667342221034680 ) ) ;
#31104 = DIRECTION ( 'NONE',  ( -0.000000000000000000, -0.000000000000000000, -1.000000000000000000 ) ) ;
#31105 = DIRECTION ( 'NONE',  ( 0.005961354470445682716, -0.6427876096865404731, -0.7660212471507180654 ) ) ;
#31106 = ORIENTED_EDGE ( 'NONE', *, *, #11307, .T. ) ;
#31107 = PLANE ( 'NONE',  #4745 ) ;
#31108 = ORIENTED_EDGE ( 'NONE', *, *, #25529, .T. ) ;
#31109 = CARTESIAN_POINT ( 'NONE',  ( -13.10003858486740214, -0.1191753592594189115, 2.971802275270698956 ) ) ;
#31110 = VECTOR ( 'NONE', #21067, 1000.000000000000114 ) ;
#31111 = LINE ( 'NONE', #22035, #10292 ) ;
#31112 = EDGE_LOOP ( 'NONE', ( #11579, #11890, #4447, #54221 ) ) ;
#31113 = LINE ( 'NONE', #36231, #3621 ) ;
#31114 = AXIS2_PLACEMENT_3D ( 'NONE', #9752, #47809, #22782 ) ;
#31115 = ORIENTED_EDGE ( 'NONE', *, *, #17717, .T. ) ;
#31116 = ORIENTED_EDGE ( 'NONE', *, *, #2135, .F. ) ;
#31117 = ORIENTED_EDGE ( 'NONE', *, *, #52634, .F. ) ;
#31118 = LINE ( 'NONE', #30069, #2091 ) ;
#31119 = ORIENTED_EDGE ( 'NONE', *, *, #49776, .T. ) ;
#31120 = ORIENTED_EDGE ( 'NONE', *, *, #20232, .T. ) ;
#31121 = VECTOR ( 'NONE', #9958, 1000.000000000000227 ) ;
#31122 = PLANE ( 'NONE',  #25671 ) ;
#31123 = DIRECTION ( 'NONE',  ( 0.005002170337468016433, -0.7660444431189770143, -0.6427681459581293666 ) ) ;
#31124 = ORIENTED_EDGE ( 'NONE', *, *, #37045, .F. ) ;
#31125 = AXIS2_PLACEMENT_3D ( 'NONE', #13244, #47882, #43884 ) ;
#31126 = AXIS2_PLACEMENT_3D ( 'NONE', #21310, #51954, #21605 ) ;
#31127 = ORIENTED_EDGE ( 'NONE', *, *, #3561, .T. ) ;
#31128 = CARTESIAN_POINT ( 'NONE',  ( -16.40420069433451289, -0.1191753592594190225, 9.590322214343837359 ) ) ;
#31129 = ORIENTED_EDGE ( 'NONE', *, *, #6086, .T. ) ;
#31130 = ORIENTED_EDGE ( 'NONE', *, *, #13620, .F. ) ;
#31131 = EDGE_CURVE ( 'NONE', #29285, #2305, #52863, .T. ) ;
#31132 = AXIS2_PLACEMENT_3D ( 'NONE', #24676, #6532, #49706 ) ;
#31133 = AXIS2_PLACEMENT_3D ( 'NONE', #52034, #29910, #34440 ) ;
#31134 = DIRECTION ( 'NONE',  ( -0.6427681459581293666, -0.7660444431189770143, -0.005002170337467561935 ) ) ;
#31135 = EDGE_CURVE ( 'NONE', #34678, #39202, #649, .T. ) ;
#31136 = CARTESIAN_POINT ( 'NONE',  ( -21.47341775636118655, -0.1191753592594197858, 5.122631121243466090 ) ) ;
#31137 = DIRECTION ( 'NONE',  ( 0.005961354470445682716, -0.6427876096865404731, -0.7660212471507180654 ) ) ;
#31138 = ADVANCED_FACE ( 'NONE', ( #1178 ), #31000, .F. ) ;
#31139 = ORIENTED_EDGE ( 'NONE', *, *, #31740, .T. ) ;
#31140 = LINE ( 'NONE', #30309, #49133 ) ;
#31141 = VERTEX_POINT ( 'NONE', #6306 ) ;
#31142 = EDGE_CURVE ( 'NONE', #13383, #14078, #35854, .T. ) ;
#31143 = CARTESIAN_POINT ( 'NONE',  ( -10.96854034462895555, 0.1245042932765021287, 1.346207436594613505 ) ) ;
#31144 = AXIS2_PLACEMENT_3D ( 'NONE', #29089, #20851, #50406 ) ;
#31145 = DIRECTION ( 'NONE',  ( 0.7660212471507180654, -0.6427876096865404731, 0.005961354470445141482 ) ) ;
#31146 = DIRECTION ( 'NONE',  ( 0.005961354470445682716, -0.6427876096865404731, -0.7660212471507180654 ) ) ;
#31147 = LINE ( 'NONE', #4479, #16871 ) ;
#31148 = CARTESIAN_POINT ( 'NONE',  ( 5.617234462649089544, -1.043562741351909740, -2.260263880414688842 ) ) ;
#31149 = LINE ( 'NONE', #22072, #42992 ) ;
#31150 = DIRECTION ( 'NONE',  ( 0.9321478471874541372, 0.000000000000000000, -0.3620778797217453771 ) ) ;
#31151 = ORIENTED_EDGE ( 'NONE', *, *, #13746, .F. ) ;
#31152 = DIRECTION ( 'NONE',  ( 0.9999697198139515519, 0.000000000000000000, 0.007781995580013368816 ) ) ;
#31153 = VECTOR ( 'NONE', #55039, 1000.000000000000000 ) ;
#31154 = DIRECTION ( 'NONE',  ( 0.007781995580012663651, -3.146120232559066537E-19, -0.9999697198139514409 ) ) ;
#31155 = DIRECTION ( 'NONE',  ( -0.005002170337468016433, -0.7660444431189770143, 0.6427681459581293666 ) ) ;
#31156 = LINE ( 'NONE', #8185, #20847 ) ;
#31157 = AXIS2_PLACEMENT_3D ( 'NONE', #8922, #30771, #21691 ) ;
#31158 = PLANE ( 'NONE',  #14992 ) ;
#31159 = LINE ( 'NONE', #39414, #17720 ) ;
#31160 = CARTESIAN_POINT ( 'NONE',  ( 2.072287782118878319, 0.000000000000000000, -2.950529333540147015 ) ) ;
#31161 = DIRECTION ( 'NONE',  ( 0.7660212471507180654, -0.6427876096865404731, 0.005961354470445141482 ) ) ;
#31162 = VERTEX_POINT ( 'NONE', #14817 ) ;
#31163 = AXIS2_PLACEMENT_3D ( 'NONE', #17156, #24828, #80 ) ;
#31164 = LINE ( 'NONE', #43652, #32951 ) ;
#31165 = LINE ( 'NONE', #44244, #3117 ) ;
#31166 = FACE_OUTER_BOUND ( 'NONE', #46886, .T. ) ;
#31167 = VECTOR ( 'NONE', #5507, 999.9999999999998863 ) ;
#31168 = VECTOR ( 'NONE', #48374, 999.9999999999998863 ) ;
#31169 = EDGE_CURVE ( 'NONE', #45628, #41178, #53440, .T. ) ;
#31170 = DIRECTION ( 'NONE',  ( -0.5364919789714478471, 0.6444004775717705469, -0.5449076811759709926 ) ) ;
#31171 = FACE_OUTER_BOUND ( 'NONE', #28970, .T. ) ;
#31172 = CARTESIAN_POINT ( 'NONE',  ( -10.27421835998572064, 0.000000000000000000, 10.96090226820206048 ) ) ;
#31173 = EDGE_CURVE ( 'NONE', #14388, #46093, #14538, .T. ) ;
#31174 = EDGE_CURVE ( 'NONE', #36024, #51395, #10585, .T. ) ;
#31175 = DIRECTION ( 'NONE',  ( 0.5364919789714477361, 0.6444004775717706579, 0.5449076811759711036 ) ) ;
#31176 = AXIS2_PLACEMENT_3D ( 'NONE', #37749, #54469, #50220 ) ;
#31177 = VECTOR ( 'NONE', #28088, 999.9999999999998863 ) ;
#31178 = DIRECTION ( 'NONE',  ( -0.9999697198139514409, -0.000000000000000000, -0.007781995580013368816 ) ) ;
#31179 = CARTESIAN_POINT ( 'NONE',  ( -11.35088832955830007, 0.000000000000000000, 4.193413804539424916 ) ) ;
#31180 = ORIENTED_EDGE ( 'NONE', *, *, #50755, .T. ) ;
#31181 = EDGE_CURVE ( 'NONE', #14703, #34243, #17969, .T. ) ;
#31182 = ORIENTED_EDGE ( 'NONE', *, *, #33034, .F. ) ;
#31183 = VERTEX_POINT ( 'NONE', #27898 ) ;
#31184 = EDGE_LOOP ( 'NONE', ( #43612, #9685, #32499, #2331 ) ) ;
#31185 = AXIS2_PLACEMENT_3D ( 'NONE', #43238, #56009, #55416 ) ;
#31186 = VERTEX_POINT ( 'NONE', #45204 ) ;
#31187 = DIRECTION ( 'NONE',  ( 0.7660212471507180654, -0.6427876096865404731, 0.005961354470445141482 ) ) ;
#31188 = DIRECTION ( 'NONE',  ( -0.9999697198139514409, -0.000000000000000000, -0.007781995580013368816 ) ) ;
#31189 = VECTOR ( 'NONE', #2635, 1000.000000000000227 ) ;
#31190 = ORIENTED_EDGE ( 'NONE', *, *, #29656, .T. ) ;
#31191 = ORIENTED_EDGE ( 'NONE', *, *, #10414, .T. ) ;
#31192 = VECTOR ( 'NONE', #26325, 1000.000000000000227 ) ;
#31193 = PLANE ( 'NONE',  #2066 ) ;
#31194 = VERTEX_POINT ( 'NONE', #40384 ) ;
#31195 = CIRCLE ( 'NONE', #15745, 3.000000000000001332 ) ;
#31196 = CYLINDRICAL_SURFACE ( 'NONE', #49969, 2.000000000000001776 ) ;
#31197 = LINE ( 'NONE', #27219, #31392 ) ;
#31198 = ORIENTED_EDGE ( 'NONE', *, *, #43720, .F. ) ;
#31199 = DIRECTION ( 'NONE',  ( 0.5449076811759707706, 0.6444004775717708799, -0.5364919789714476250 ) ) ;
#31200 = VECTOR ( 'NONE', #31839, 1000.000000000000000 ) ;
#31201 = ORIENTED_EDGE ( 'NONE', *, *, #6249, .F. ) ;
#31202 = CARTESIAN_POINT ( 'NONE',  ( -9.542064456761055524, 0.000000000000000000, 10.59726798936431180 ) ) ;
#31203 = EDGE_CURVE ( 'NONE', #17816, #11120, #36139, .T. ) ;
#31204 = DIRECTION ( 'NONE',  ( 0.9321478471874541372, 0.000000000000000000, -0.3620778797217453771 ) ) ;
#31205 = AXIS2_PLACEMENT_3D ( 'NONE', #46749, #12094, #3317 ) ;
#31206 = LINE ( 'NONE', #44829, #52697 ) ;
#31207 = CARTESIAN_POINT ( 'NONE',  ( -17.97791203186454112, 1.257817950434005683, 3.625032319110802259 ) ) ;
#31208 = VECTOR ( 'NONE', #18044, 999.9999999999998863 ) ;
#31209 = ORIENTED_EDGE ( 'NONE', *, *, #42887, .T. ) ;
#31210 = CARTESIAN_POINT ( 'NONE',  ( -12.80323208052646855, 3.362543313726509719, 7.373037692220082207 ) ) ;
#31211 = DIRECTION ( 'NONE',  ( 0.6246952433987894571, -0.7422098413412800966, -0.2426528472758541777 ) ) ;
#31212 = DIRECTION ( 'NONE',  ( -0.7660212471507179544, -0.6427876096865405842, -0.005961354470445141482 ) ) ;
#31213 = VERTEX_POINT ( 'NONE', #44926 ) ;
#31214 = CARTESIAN_POINT ( 'NONE',  ( -17.46532115785441519, 0.000000000000000000, 13.67492996699914265 ) ) ;
#31215 = ORIENTED_EDGE ( 'NONE', *, *, #8809, .T. ) ;
#31216 = ADVANCED_FACE ( 'NONE', ( #6040 ), #1744, .F. ) ;
#31217 = LINE ( 'NONE', #14734, #25570 ) ;
#31218 = LINE ( 'NONE', #34939, #8795 ) ;
#31219 = DIRECTION ( 'NONE',  ( 0.005002170337468016433, -0.7660444431189770143, -0.6427681459581293666 ) ) ;
#31220 = DIRECTION ( 'NONE',  ( 0.000000000000000000, -0.000000000000000000, -1.000000000000000000 ) ) ;
#31221 = DIRECTION ( 'NONE',  ( -0.9999697198139514409, -0.000000000000000000, -0.007781995580013368816 ) ) ;
#31222 = EDGE_CURVE ( 'NONE', #38353, #24617, #5045, .T. ) ;
#31223 = DIRECTION ( 'NONE',  ( 0.000000000000000000, -1.000000000000000000, 0.000000000000000000 ) ) ;
#31225 = EDGE_CURVE ( 'NONE', #10401, #20294, #19066, .T. ) ;
#31224 = FACE_OUTER_BOUND ( 'NONE', #35196, .T. ) ;
#31226 = AXIS2_PLACEMENT_3D ( 'NONE', #29233, #51094, #167 ) ;
#31227 = LINE ( 'NONE', #9363, #24749 ) ;
#31228 = LINE ( 'NONE', #13901, #25984 ) ;
#31229 = VERTEX_POINT ( 'NONE', #23353 ) ;
#31230 = CARTESIAN_POINT ( 'NONE',  ( -26.13493519185646008, 0.000000000000000000, 7.033017491833586377 ) ) ;
#31231 = DIRECTION ( 'NONE',  ( -0.5449076811759708816, 0.6444004775717707689, 0.5364919789714475140 ) ) ;
#31232 = EDGE_CURVE ( 'NONE', #37122, #40408, #40672, .T. ) ;
#31233 = DIRECTION ( 'NONE',  ( 0.007781995580012663651, -3.146120232559066537E-19, -0.9999697198139514409 ) ) ;
#31234 = VECTOR ( 'NONE', #7983, 999.9999999999998863 ) ;
#31235 = FACE_OUTER_BOUND ( 'NONE', #12324, .T. ) ;
#31236 = ADVANCED_FACE ( 'NONE', ( #13686 ), #48319, .F. ) ;
#31237 = PLANE ( 'NONE',  #20043 ) ;
#31238 = DIRECTION ( 'NONE',  ( -0.5364919789714478471, 0.6444004775717705469, -0.5449076811759709926 ) ) ;
#31239 = EDGE_CURVE ( 'NONE', #29528, #36994, #5737, .T. ) ;
#31240 = DIRECTION ( 'NONE',  ( -0.7660212471507179544, -0.6427876096865405842, -0.005961354470445141482 ) ) ;
#31241 = ORIENTED_EDGE ( 'NONE', *, *, #46948, .T. ) ;
#31242 = VECTOR ( 'NONE', #50757, 999.9999999999998863 ) ;
#31243 = VERTEX_POINT ( 'NONE', #18818 ) ;
#31244 = DIRECTION ( 'NONE',  ( -0.9335804264972047406, 0.3583679495452925523, 0.000000000000000000 ) ) ;
#31245 = VECTOR ( 'NONE', #11893, 999.9999999999998863 ) ;
#31246 = DIRECTION ( 'NONE',  ( 0.9999697198139515519, 0.000000000000000000, 0.007781995580013368816 ) ) ;
#31247 = VECTOR ( 'NONE', #56029, 1000.000000000000114 ) ;
#31248 = EDGE_CURVE ( 'NONE', #36758, #36001, #40089, .T. ) ;
#31249 = ORIENTED_EDGE ( 'NONE', *, *, #10930, .F. ) ;
#31250 = DIRECTION ( 'NONE',  ( -0.5364919789714478471, 0.6444004775717705469, -0.5449076811759709926 ) ) ;
#31251 = ORIENTED_EDGE ( 'NONE', *, *, #21641, .T. ) ;
#31252 = CARTESIAN_POINT ( 'NONE',  ( -18.66354898467281132, 0.000000000000000000, 14.21960318569776582 ) ) ;
#31253 = EDGE_CURVE ( 'NONE', #40596, #15338, #54823, .T. ) ;
#31254 = VECTOR ( 'NONE', #48070, 999.9999999999998863 ) ;
#31255 = ORIENTED_EDGE ( 'NONE', *, *, #49770, .T. ) ;
#31256 = VECTOR ( 'NONE', #28671, 1000.000000000000114 ) ;
#31257 = ORIENTED_EDGE ( 'NONE', *, *, #53005, .F. ) ;
#31258 = ORIENTED_EDGE ( 'NONE', *, *, #37791, .T. ) ;
#31259 = CARTESIAN_POINT ( 'NONE',  ( -16.79925329029790149, 0.000000000000000000, 13.49544742625427496 ) ) ;
#31260 = DIRECTION ( 'NONE',  ( 0.9999697198139515519, 0.000000000000000000, 0.007781995580013368816 ) ) ;
#31261 = DIRECTION ( 'NONE',  ( 0.5449076811759707706, 0.6444004775717708799, -0.5364919789714476250 ) ) ;
#31262 = PLANE ( 'NONE',  #41992 ) ;
#31263 = EDGE_LOOP ( 'NONE', ( #42064, #33188, #35880, #45556 ) ) ;
#31264 = VERTEX_POINT ( 'NONE', #20168 ) ;
#31265 = VECTOR ( 'NONE', #53641, 1000.000000000000227 ) ;
#31266 = LINE ( 'NONE', #27278, #10052 ) ;
#31267 = AXIS2_PLACEMENT_3D ( 'NONE', #36927, #32638, #49943 ) ;
#31268 = EDGE_LOOP ( 'NONE', ( #17945, #45883, #18556, #38519 ) ) ;
#31269 = PLANE ( 'NONE',  #35521 ) ;
#31270 = ORIENTED_EDGE ( 'NONE', *, *, #22202, .F. ) ;
#31271 = VECTOR ( 'NONE', #894, 999.9999999999998863 ) ;
#31272 = CARTESIAN_POINT ( 'NONE',  ( -18.39746900504187010, 0.000000000000000000, 14.03700784672088808 ) ) ;
#31273 = CARTESIAN_POINT ( 'NONE',  ( -12.33850799832341849, 0.000000000000000000, 11.68350162852954632 ) ) ;
#31274 = ORIENTED_EDGE ( 'NONE', *, *, #34015, .F. ) ;
#31275 = DIRECTION ( 'NONE',  ( 0.6427681459581294776, -0.7660444431189769032, 0.005002170337467562802 ) ) ;
#31276 = EDGE_CURVE ( 'NONE', #39446, #50762, #45739, .T. ) ;
#31277 = VECTOR ( 'NONE', #15610, 1000.000000000000227 ) ;
#31278 = ORIENTED_EDGE ( 'NONE', *, *, #32631, .T. ) ;
#31279 = CARTESIAN_POINT ( 'NONE',  ( -17.01269937210870964, 1.743523803501506819, 6.351050902876947291 ) ) ;
#31280 = VECTOR ( 'NONE', #27346, 1000.000000000000227 ) ;
#31281 = AXIS2_PLACEMENT_3D ( 'NONE', #28989, #50577, #55663 ) ;
#31282 = EDGE_LOOP ( 'NONE', ( #39984, #1543, #22173, #12685 ) ) ;
#31283 = LINE ( 'NONE', #886, #19612 ) ;
#31284 = LINE ( 'NONE', #48614, #4859 ) ;
#31285 = VECTOR ( 'NONE', #18759, 999.9999999999998863 ) ;
#31286 = VECTOR ( 'NONE', #33156, 1000.000000000000227 ) ;
#31287 = LINE ( 'NONE', #23049, #32821 ) ;
#31288 = ORIENTED_EDGE ( 'NONE', *, *, #43627, .T. ) ;
#31289 = AXIS2_PLACEMENT_3D ( 'NONE', #23057, #1473, #6034 ) ;
#31290 = EDGE_CURVE ( 'NONE', #4086, #12666, #24715, .T. ) ;
#31291 = FACE_OUTER_BOUND ( 'NONE', #619, .T. ) ;
#31292 = PLANE ( 'NONE',  #20127 ) ;
#31293 = LINE ( 'NONE', #35843, #23091 ) ;
#31294 = CARTESIAN_POINT ( 'NONE',  ( -56.07732056155856526, 3.800000000000001155, -1.969389477338281624 ) ) ;
#31295 = LINE ( 'NONE', #14812, #25871 ) ;
#31297 = EDGE_CURVE ( 'NONE', #54809, #1909, #2584, .T. ) ;
#31296 = DIRECTION ( 'NONE',  ( 0.005961354470445682716, -0.6427876096865404731, -0.7660212471507180654 ) ) ;
#31298 = VECTOR ( 'NONE', #12419, 999.9999999999998863 ) ;
#31299 = VECTOR ( 'NONE', #2444, 1000.000000000000000 ) ;
#31300 =( NAMED_UNIT ( * ) SI_UNIT ( $, .STERADIAN. ) SOLID_ANGLE_UNIT ( ) );
#31301 = ORIENTED_EDGE ( 'NONE', *, *, #26168, .T. ) ;
#31302 = PLANE ( 'NONE',  #15315 ) ;
#31303 = CARTESIAN_POINT ( 'NONE',  ( -18.19192721912726896, 5.305366725996512045, 12.65469409231538833 ) ) ;
#31304 = CARTESIAN_POINT ( 'NONE',  ( -17.74482636761137044, -0.1191753592594197858, 3.674319602356483916 ) ) ;
#31305 = ORIENTED_EDGE ( 'NONE', *, *, #39409, .F. ) ;
#31306 = DIRECTION ( 'NONE',  ( 0.005961354470445682716, -0.6427876096865404731, -0.7660212471507180654 ) ) ;
#31307 = DIRECTION ( 'NONE',  ( 0.9999697198139515519, 0.000000000000000000, 0.007781995580013368816 ) ) ;
#31308 = ORIENTED_EDGE ( 'NONE', *, *, #20248, .F. ) ;
#31309 = LINE ( 'NONE', #13443, #51561 ) ;
#31310 = EDGE_CURVE ( 'NONE', #2289, #1437, #49988, .T. ) ;
#31311 = LINE ( 'NONE', #52343, #35727 ) ;
#31312 = LINE ( 'NONE', #23071, #55913 ) ;
#31313 = ADVANCED_FACE ( 'NONE', ( #28422 ), #37219, .F. ) ;
#31314 = CARTESIAN_POINT ( 'NONE',  ( -9.752553242450971993, 0.000000000000000000, 3.636514291738904170 ) ) ;
#31315 = AXIS2_PLACEMENT_3D ( 'NONE', #27390, #18899, #11751 ) ;
#31316 = EDGE_LOOP ( 'NONE', ( #24080, #45473, #41300, #18467 ) ) ;
#31317 = VERTEX_POINT ( 'NONE', #6867 ) ;
#31318 = AXIS2_PLACEMENT_3D ( 'NONE', #3339, #52153, #51858 ) ;
#31319 = CARTESIAN_POINT ( 'NONE',  ( -24.26986129792355129, -0.1191753592594197858, 6.208864760408702388 ) ) ;
#31320 = DIRECTION ( 'NONE',  ( 0.000000000000000000, -0.000000000000000000, -1.000000000000000000 ) ) ;
#31321 = CARTESIAN_POINT ( 'NONE',  ( -65.33883713333176502, 2.000000000000018208, 0.6542134465202600335 ) ) ;
#31322 = AXIS2_PLACEMENT_3D ( 'NONE', #52653, #25707, #34791 ) ;
#31323 = LINE ( 'NONE', #48651, #42004 ) ;
#31324 = ADVANCED_FACE ( 'NONE', ( #23884 ), #36679, .F. ) ;
#31325 = CARTESIAN_POINT ( 'NONE',  ( -21.47976836131305234, -2.298917212465657833, 8.798318018248513894 ) ) ;
#31326 = FACE_OUTER_BOUND ( 'NONE', #36161, .T. ) ;
#31327 = VECTOR ( 'NONE', #12140, 999.9999999999998863 ) ;
#31328 = ORIENTED_EDGE ( 'NONE', *, *, #27610, .T. ) ;
#31329 = LINE ( 'NONE', #1202, #37382 ) ;
#31330 = EDGE_CURVE ( 'NONE', #10301, #17288, #45456, .T. ) ;
#31331 = CARTESIAN_POINT ( 'NONE',  ( -15.88130887279446490, 0.000000000000000000, 3.050160814894388839 ) ) ;
#31332 = VECTOR ( 'NONE', #1721, 1000.000000000000114 ) ;
#31334 = ORIENTED_EDGE ( 'NONE', *, *, #7725, .F. ) ;
#31333 = AXIS2_PLACEMENT_3D ( 'NONE', #21514, #49211, #39862 ) ;
#31335 = FACE_OUTER_BOUND ( 'NONE', #5202, .T. ) ;
#31336 = CARTESIAN_POINT ( 'NONE',  ( 2.072287782118878319, 0.000000000000000000, -2.950529333540147015 ) ) ;
#31337 = CARTESIAN_POINT ( 'NONE',  ( -14.57595350043041194, -2.946525016555658905, 7.179476607543993083 ) ) ;
#31338 = AXIS2_PLACEMENT_3D ( 'NONE', #36536, #49619, #45336 ) ;
#31339 = VERTEX_POINT ( 'NONE', #46288 ) ;
#31340 = VECTOR ( 'NONE', #27640, 1000.000000000000000 ) ;
#31341 = PLANE ( 'NONE',  #24723 ) ;
#31342 = ORIENTED_EDGE ( 'NONE', *, *, #38974, .F. ) ;
#31343 = VECTOR ( 'NONE', #39593, 999.9999999999998863 ) ;
#31344 = ORIENTED_EDGE ( 'NONE', *, *, #6851, .F. ) ;
#31345 = VECTOR ( 'NONE', #5200, 1000.000000000000227 ) ;
#31346 = ORIENTED_EDGE ( 'NONE', *, *, #45485, .T. ) ;
#31347 = EDGE_LOOP ( 'NONE', ( #38904, #1303, #46683, #48442 ) ) ;
#31348 = LINE ( 'NONE', #13726, #43872 ) ;
#31349 = ORIENTED_EDGE ( 'NONE', *, *, #8250, .T. ) ;
#31350 = CARTESIAN_POINT ( 'NONE',  ( -55.47117325737978888, 6.581829179614757663, 1.080525476705103127 ) ) ;
#31351 = DIRECTION ( 'NONE',  ( 0.007781995580012662783, 0.000000000000000000, -0.9999697198139514409 ) ) ;
#31352 = ORIENTED_EDGE ( 'NONE', *, *, #20846, .F. ) ;
#31353 = DIRECTION ( 'NONE',  ( 0.007781995580012663651, 0.000000000000000000, -0.9999697198139515519 ) ) ;
#31354 = EDGE_LOOP ( 'NONE', ( #1146, #8910, #37256, #16609 ) ) ;
#31355 = DIRECTION ( 'NONE',  ( 0.007781995580012662783, 0.000000000000000000, -0.9999697198139514409 ) ) ;
#31356 = EDGE_CURVE ( 'NONE', #34418, #54919, #40924, .T. ) ;
#31357 = ORIENTED_EDGE ( 'NONE', *, *, #11924, .F. ) ;
#31358 = VECTOR ( 'NONE', #44100, 999.9999999999998863 ) ;
#31359 = DIRECTION ( 'NONE',  ( 0.6427681459581294776, -0.7660444431189769032, 0.005002170337467562802 ) ) ;
#31360 = EDGE_CURVE ( 'NONE', #28311, #3535, #27706, .T. ) ;
#31361 = CARTESIAN_POINT ( 'NONE',  ( -0.2408075302807476947, -4.234515647955085171, 3.311911398282993524 ) ) ;
#31362 = VECTOR ( 'NONE', #28005, 1000.000000000000000 ) ;
#31363 = CARTESIAN_POINT ( 'NONE',  ( -23.34675815411524979, 18.98665190278753556, 4.490845985905339788 ) ) ;
#31364 = EDGE_CURVE ( 'NONE', #32426, #14652, #41212, .T. ) ;
#31365 = DIRECTION ( 'NONE',  ( 0.000000000000000000, -0.000000000000000000, -1.000000000000000000 ) ) ;
#31366 = CARTESIAN_POINT ( 'NONE',  ( -15.92740756652831102, 3.200641362704007786, 8.320864864478828338 ) ) ;
#31367 = CARTESIAN_POINT ( 'NONE',  ( -18.04930495852531536, -5.375054281893163477, 12.51427452863701895 ) ) ;
#31368 = AXIS2_PLACEMENT_3D ( 'NONE', #14415, #31460, #48775 ) ;
#31369 = ORIENTED_EDGE ( 'NONE', *, *, #19994, .F. ) ;
#31370 = ADVANCED_FACE ( 'NONE', ( #2008 ), #41502, .F. ) ;
#31371 = EDGE_CURVE ( 'NONE', #40825, #49950, #15936, .T. ) ;
#31372 = ADVANCED_FACE ( 'NONE', ( #15114 ), #32438, .F. ) ;
#31373 = EDGE_LOOP ( 'NONE', ( #1670, #41631, #42203, #9463 ) ) ;
#31374 = PLANE ( 'NONE',  #11944 ) ;
#31375 = DIRECTION ( 'NONE',  ( 0.9321478471874540261, -0.000000000000000000, -0.3620778797217457101 ) ) ;
#31376 = VECTOR ( 'NONE', #36132, 999.9999999999998863 ) ;
#31377 = CARTESIAN_POINT ( 'NONE',  ( -23.33771345073609638, -0.1191753592594197858, 5.846786880686956955 ) ) ;
#31378 = VECTOR ( 'NONE', #22983, 1000.000000000000227 ) ;
#31379 = AXIS2_PLACEMENT_3D ( 'NONE', #13954, #13420, #14268 ) ;
#31380 = CARTESIAN_POINT ( 'NONE',  ( -12.17651289819579929, -0.1191753592594186895, 3.717653505322246144 ) ) ;
#31381 = ORIENTED_EDGE ( 'NONE', *, *, #52450, .F. ) ;
#31382 = CARTESIAN_POINT ( 'NONE',  ( -7.291207867172650126, -7.010517566319160565, -0.3862208295925149693 ) ) ;
#31383 = DIRECTION ( 'NONE',  ( 0.007781995580012663651, -3.146120232559066537E-19, -0.9999697198139514409 ) ) ;
#31384 = ORIENTED_EDGE ( 'NONE', *, *, #18475, .T. ) ;
#31385 = DIRECTION ( 'NONE',  ( 0.9999697198139515519, 0.000000000000000000, 0.007781995580013368816 ) ) ;
#31386 = AXIS2_PLACEMENT_3D ( 'NONE', #36262, #32293, #49609 ) ;
#31387 = CARTESIAN_POINT ( 'NONE',  ( -15.65448691412668580, 5.143464774974014553, 2.598562622234925623 ) ) ;
#31388 = ORIENTED_EDGE ( 'NONE', *, *, #17459, .F. ) ;
#31389 = VECTOR ( 'NONE', #17617, 999.9999999999998863 ) ;
#31390 = CARTESIAN_POINT ( 'NONE',  ( -9.070553403303552642, 0.000000000000000000, 3.641821772184214101 ) ) ;
#31391 = DIRECTION ( 'NONE',  ( -0.005961354470445682716, -0.6427876096865404731, 0.7660212471507180654 ) ) ;
#31392 = VECTOR ( 'NONE', #5100, 999.9999999999998863 ) ;
#31393 = EDGE_CURVE ( 'NONE', #21230, #51597, #54272, .T. ) ;
#31394 = DIRECTION ( 'NONE',  ( 0.7660212471507180654, -0.6427876096865404731, 0.005961354470445141482 ) ) ;
#31395 = CARTESIAN_POINT ( 'NONE',  ( -22.40478740399063895, 0.000000000000000000, 5.384712028983816623 ) ) ;
#31396 = VECTOR ( 'NONE', #14502, 1000.000000000000227 ) ;
#31397 = EDGE_CURVE ( 'NONE', #55983, #25397, #11100, .T. ) ;
#31398 = LINE ( 'NONE', #17774, #9304 ) ;
#31399 = ORIENTED_EDGE ( 'NONE', *, *, #25576, .F. ) ;
#31400 = VECTOR ( 'NONE', #47352, 1000.000000000000114 ) ;
#31401 = VERTEX_POINT ( 'NONE', #28727 ) ;
#31402 = EDGE_CURVE ( 'NONE', #17816, #35294, #46035, .T. ) ;
#31403 = CARTESIAN_POINT ( 'NONE',  ( -19.55525183663760913, 3.686347215771509589, 4.160241867659052240 ) ) ;
#31404 = CARTESIAN_POINT ( 'NONE',  ( -13.07066190154808361, 0.000000000000000000, 12.04713590736729678 ) ) ;
#31405 = CARTESIAN_POINT ( 'NONE',  ( -12.18721420714108028, -1.813211359398158029, 1.557398059203232377 ) ) ;
#31406 = EDGE_CURVE ( 'NONE', #47316, #30844, #13007, .T. ) ;
#31407 = CARTESIAN_POINT ( 'NONE',  ( -16.25459574472089130, 0.000000000000000000, 3.216581823729005585 ) ) ;
#31408 = PLANE ( 'NONE',  #23950 ) ;
#31409 = EDGE_LOOP ( 'NONE', ( #14196, #31116, #3664, #47127 ) ) ;
#31410 = CARTESIAN_POINT ( 'NONE',  ( -16.09647726239903776, 23.36497036543017813, -3.956233406722669432 ) ) ;
#31411 = CARTESIAN_POINT ( 'NONE',  ( -18.80232300004736956, 0.000000000000000000, 6.351417435797861444 ) ) ;
#31412 = VECTOR ( 'NONE', #16947, 999.9999999999998863 ) ;
#31413 = DIRECTION ( 'NONE',  ( 0.6427681459581294776, -0.7660444431189769032, 0.005002170337467562802 ) ) ;
#31414 = DIRECTION ( 'NONE',  ( 0.7660212471507180654, -0.6427876096865404731, 0.005961354470445141482 ) ) ;
#31415 = ORIENTED_EDGE ( 'NONE', *, *, #1320, .F. ) ;
#31416 = LINE ( 'NONE', #9833, #34739 ) ;
#31417 = EDGE_LOOP ( 'NONE', ( #26104, #38070, #14801, #47778 ) ) ;
#31418 = CARTESIAN_POINT ( 'NONE',  ( -21.93567466420777379, 19.99370817364452790, -4.408991681665293427 ) ) ;
#31419 = VECTOR ( 'NONE', #55180, 1000.000000000000000 ) ;
#31420 = DIRECTION ( 'NONE',  ( 0.9999697198139515519, 0.000000000000000000, 0.007781995580013368816 ) ) ;
#31421 = ORIENTED_EDGE ( 'NONE', *, *, #39523, .F. ) ;
#31422 = CARTESIAN_POINT ( 'NONE',  ( -10.37421533196711465, -0.1191753592594197858, 10.96012406864405975 ) ) ;
#31423 = VECTOR ( 'NONE', #27323, 1000.000000000000114 ) ;
#31424 = ORIENTED_EDGE ( 'NONE', *, *, #30670, .T. ) ;
#31425 = ORIENTED_EDGE ( 'NONE', *, *, #4388, .T. ) ;
#31426 = AXIS2_PLACEMENT_3D ( 'NONE', #18368, #22078, #39115 ) ;
#31427 = VERTEX_POINT ( 'NONE', #9295 ) ;
#31428 = LINE ( 'NONE', #55621, #21193 ) ;
#31429 = ORIENTED_EDGE ( 'NONE', *, *, #42479, .F. ) ;
#31430 = ORIENTED_EDGE ( 'NONE', *, *, #13979, .F. ) ;
#31431 = PLANE ( 'NONE',  #26560 ) ;
#31432 = DIRECTION ( 'NONE',  ( 0.9999697198139515519, 0.000000000000000000, 0.007781995580013368816 ) ) ;
#31433 = ORIENTED_EDGE ( 'NONE', *, *, #28187, .F. ) ;
#31434 = VECTOR ( 'NONE', #1019, 999.9999999999998863 ) ;
#31435 = VECTOR ( 'NONE', #22826, 1000.000000000000227 ) ;
#31436 = ORIENTED_EDGE ( 'NONE', *, *, #23745, .T. ) ;
#31437 = CARTESIAN_POINT ( 'NONE',  ( -20.46176247598743103, -2.784623065533159636, 4.740520492340843717 ) ) ;
#31438 = EDGE_LOOP ( 'NONE', ( #21228, #23467, #44095, #1929 ) ) ;
#31439 = ORIENTED_EDGE ( 'NONE', *, *, #46792, .F. ) ;
#31440 = CIRCLE ( 'NONE', #24166, 2.749999999999997335 ) ;
#31441 = AXIS2_PLACEMENT_3D ( 'NONE', #46661, #54603, #33599 ) ;
#31442 = EDGE_CURVE ( 'NONE', #14652, #10233, #5340, .T. ) ;
#31443 = LINE ( 'NONE', #49015, #12045 ) ;
#31444 = CARTESIAN_POINT ( 'NONE',  ( -16.79925329029790149, 0.000000000000000000, 13.49544742625427496 ) ) ;
#31445 = LINE ( 'NONE', #40527, #45009 ) ;
#31446 = FACE_OUTER_BOUND ( 'NONE', #17813, .T. ) ;
#31447 = ORIENTED_EDGE ( 'NONE', *, *, #43715, .F. ) ;
#31448 = CARTESIAN_POINT ( 'NONE',  ( -14.10280672071693431, -0.1191753592594197858, 12.40843558753103792 ) ) ;
#31449 = ORIENTED_EDGE ( 'NONE', *, *, #15883, .T. ) ;
#31450 = ADVANCED_FACE ( 'NONE', ( #22649 ), #26089, .F. ) ;
#31451 = EDGE_CURVE ( 'NONE', #50934, #46898, #48187, .T. ) ;
#31452 = CARTESIAN_POINT ( 'NONE',  ( -12.80458192191714595, 0.000000000000000000, 11.86454056839041726 ) ) ;
#31453 = EDGE_CURVE ( 'NONE', #21908, #8254, #39121, .T. ) ;
#31454 = AXIS2_PLACEMENT_3D ( 'NONE', #7387, #37800, #46567 ) ;
#31455 = LINE ( 'NONE', #52456, #24201 ) ;
#31456 = CARTESIAN_POINT ( 'NONE',  ( -30.79411802867772607, 0.000000000000000000, 8.643412946479525516 ) ) ;
#31457 = CARTESIAN_POINT ( 'NONE',  ( -16.72941120119383029, 0.000000000000000000, 4.520888965697079875 ) ) ;
#31458 = DIRECTION ( 'NONE',  ( 0.000000000000000000, -1.000000000000000000, 0.000000000000000000 ) ) ;
#31459 = DIRECTION ( 'NONE',  ( 0.000000000000000000, 1.000000000000000000, 0.000000000000000000 ) ) ;
#31460 = DIRECTION ( 'NONE',  ( -0.005961354470445682716, -0.6427876096865404731, 0.7660212471507180654 ) ) ;
#31461 = ORIENTED_EDGE ( 'NONE', *, *, #26294, .T. ) ;
#31462 = FACE_OUTER_BOUND ( 'NONE', #40532, .T. ) ;
#31463 = PLANE ( 'NONE',  #225 ) ;
#31464 = DIRECTION ( 'NONE',  ( -0.5364919789714478471, 0.6444004775717705469, -0.5449076811759709926 ) ) ;
#31466 = DIRECTION ( 'NONE',  ( 0.6427681459581294776, -0.7660444431189769032, 0.005002170337467562802 ) ) ;
#31465 = VECTOR ( 'NONE', #40188, 999.9999999999998863 ) ;
#31467 = FACE_OUTER_BOUND ( 'NONE', #52559, .T. ) ;
#31468 = CARTESIAN_POINT ( 'NONE',  ( -15.60102546347950536, 0.000000000000000000, 12.95077420755565356 ) ) ;
#31469 = ADVANCED_FACE ( 'NONE', ( #9031 ), #47653, .F. ) ;
#31470 = CARTESIAN_POINT ( 'NONE',  ( -19.60834386242827776, 0.000000000000000000, 4.298478389818581213 ) ) ;
#31471 = AXIS2_PLACEMENT_3D ( 'NONE', #38265, #51041, #16143 ) ;
#31472 = CARTESIAN_POINT ( 'NONE',  ( -70.38892378062969613, -1.000000000000149436, 7.852029984319922384 ) ) ;
#31473 = ORIENTED_EDGE ( 'NONE', *, *, #4604, .F. ) ;
#31474 = EDGE_CURVE ( 'NONE', #43785, #42567, #43395, .T. ) ;
#31475 = FACE_OUTER_BOUND ( 'NONE', #22497, .T. ) ;
#31476 = CARTESIAN_POINT ( 'NONE',  ( -22.36868959911851462, 19.74370688441071309, 4.433756599430258127 ) ) ;
#31477 = LINE ( 'NONE', #5606, #45999 ) ;
#31478 = ADVANCED_FACE ( 'NONE', ( #48484 ), #1044, .F. ) ;
#31479 = VECTOR ( 'NONE', #16133, 999.9999999999998863 ) ;
#31480 = DIRECTION ( 'NONE',  ( -0.005961354470445682716, -0.6427876096865404731, 0.7660212471507180654 ) ) ;
#31481 = DIRECTION ( 'NONE',  ( 0.7660212471507180654, -0.6427876096865404731, 0.005961354470445141482 ) ) ;
#31482 = LINE ( 'NONE', #48795, #44964 ) ;
#31483 = LINE ( 'NONE', #48495, #24702 ) ;
#31484 = EDGE_CURVE ( 'NONE', #2493, #38484, #506, .T. ) ;
#31485 = AXIS2_PLACEMENT_3D ( 'NONE', #55676, #30700, #43459 ) ;
#31486 = CARTESIAN_POINT ( 'NONE',  ( -68.64163227075424345, -9.699815782473507397, 6.404540763468498099 ) ) ;
#31487 = CARTESIAN_POINT ( 'NONE',  ( -15.22910602592149765, 0.000000000000000000, 9.133875538749295586 ) ) ;
#31488 = ORIENTED_EDGE ( 'NONE', *, *, #37718, .F. ) ;
#31489 = AXIS2_PLACEMENT_3D ( 'NONE', #29028, #3475, #25601 ) ;
#31490 = VERTEX_POINT ( 'NONE', #17544 ) ;
#31491 = ORIENTED_EDGE ( 'NONE', *, *, #31886, .T. ) ;
#31492 = ORIENTED_EDGE ( 'NONE', *, *, #55641, .T. ) ;
#31493 = ORIENTED_EDGE ( 'NONE', *, *, #34271, .F. ) ;
#31494 = DIRECTION ( 'NONE',  ( 0.9999697198139515519, 0.000000000000000000, 0.007781995580013368816 ) ) ;
#31495 = CARTESIAN_POINT ( 'NONE',  ( -24.27063949748155380, 0.000000000000000000, 6.308861732390097288 ) ) ;
#31496 = ORIENTED_EDGE ( 'NONE', *, *, #43632, .F. ) ;
#31497 = VECTOR ( 'NONE', #31028, 999.9999999999998863 ) ;
#31498 = ORIENTED_EDGE ( 'NONE', *, *, #25341, .F. ) ;
#31499 = ORIENTED_EDGE ( 'NONE', *, *, #1241, .F. ) ;
#31500 = VECTOR ( 'NONE', #31083, 999.9999999999998863 ) ;
#31501 = CARTESIAN_POINT ( 'NONE',  ( -67.90139828824541723, -8.876202928981230755, -5.589544126885695796 ) ) ;
#31502 = ORIENTED_EDGE ( 'NONE', *, *, #4387, .F. ) ;
#31503 = DIRECTION ( 'NONE',  ( -0.5449076811759708816, 0.6444004775717707689, 0.5364919789714475140 ) ) ;
#31504 = DIRECTION ( 'NONE',  ( 0.5449076811759707706, 0.6444004775717708799, -0.5364919789714476250 ) ) ;
#31505 = EDGE_LOOP ( 'NONE', ( #46001, #26875, #49749, #41532, #47282 ) ) ;
#31506 = PLANE ( 'NONE',  #46524 ) ;
#31508 = ORIENTED_EDGE ( 'NONE', *, *, #2520, .T. ) ;
#31507 = EDGE_CURVE ( 'NONE', #39389, #31631, #43114, .T. ) ;
#31509 = B_SPLINE_CURVE_WITH_KNOTS ( 'NONE', 3,
 ( #55514, #38195, #29412, #50966 ),
 .UNSPECIFIED., .F., .F.,
 ( 4, 4 ),
 ( 0.000000000000000000, 1.000000000000000000 ),
 .UNSPECIFIED. ) ;
#31510 = VECTOR ( 'NONE', #24565, 999.9999999999998863 ) ;
#31511 = CARTESIAN_POINT ( 'NONE',  ( -21.33651914525451687, -3.270328918600659662, 5.064809129883542482 ) ) ;
#31512 = CARTESIAN_POINT ( 'NONE',  ( -19.45503627000849889, -1.000000000000000000, 7.556996783084074742 ) ) ;
#31513 = EDGE_CURVE ( 'NONE', #34665, #31630, #18373, .T. ) ;
#31514 = EDGE_CURVE ( 'NONE', #39217, #10989, #35176, .T. ) ;
#31515 = LINE ( 'NONE', #53365, #42722 ) ;
#31516 = DIRECTION ( 'NONE',  ( -0.7660212471507179544, -0.6427876096865405842, -0.005961354470445141482 ) ) ;
#31517 = ORIENTED_EDGE ( 'NONE', *, *, #46265, .T. ) ;
#31518 = LINE ( 'NONE', #47708, #424 ) ;
#31519 = DIRECTION ( 'NONE',  ( -0.6427681459581293666, -0.7660444431189770143, -0.005002170337467561935 ) ) ;
#31520 = DIRECTION ( 'NONE',  ( 0.007781995580012663651, -3.146120232559066537E-19, -0.9999697198139514409 ) ) ;
#31521 = VERTEX_POINT ( 'NONE', #52471 ) ;
#31522 = PLANE ( 'NONE',  #27393 ) ;
#31523 = ORIENTED_EDGE ( 'NONE', *, *, #6663, .F. ) ;
#31524 = CARTESIAN_POINT ( 'NONE',  ( -22.40556560354864146, -0.1191753592594197858, 5.484709000965211523 ) ) ;
#31525 = DIRECTION ( 'NONE',  ( 0.007781995580012663651, 0.000000000000000000, -0.9999697198139515519 ) ) ;
#31526 = CARTESIAN_POINT ( 'NONE',  ( -20.66714045964574709, 20.62987310936011909, 4.333808234688889094 ) ) ;
#31527 = CARTESIAN_POINT ( 'NONE',  ( 2.072287782118878319, 0.000000000000000000, -2.950529333540147015 ) ) ;
#31528 = DIRECTION ( 'NONE',  ( -0.7660212471507179544, -0.6427876096865405842, -0.005961354470445141482 ) ) ;
#31529 = DIRECTION ( 'NONE',  ( 0.000000000000000000, -0.000000000000000000, -1.000000000000000000 ) ) ;
#31530 = LINE ( 'NONE', #40016, #33401 ) ;
#31531 = CARTESIAN_POINT ( 'NONE',  ( -8.875996589204540044, 0.000000000000000000, 10.41778544861944233 ) ) ;
#31532 = SURFACE_STYLE_FILL_AREA ( #52529 ) ;
#31533 = CARTESIAN_POINT ( 'NONE',  ( -12.15271748404464880, 0.000000000000000000, 1.601849296007406664 ) ) ;
#31534 = ORIENTED_EDGE ( 'NONE', *, *, #46101, .F. ) ;
#31535 = CARTESIAN_POINT ( 'NONE',  ( -22.45197700822111031, 5.467268677019013978, 5.228607578741694795 ) ) ;
#31536 = DIRECTION ( 'NONE',  ( 0.000000000000000000, -0.000000000000000000, -1.000000000000000000 ) ) ;
#31537 = DIRECTION ( 'NONE',  ( -0.9999697198139514409, -0.000000000000000000, -0.007781995580013368816 ) ) ;
#31538 = CARTESIAN_POINT ( 'NONE',  ( -16.53317331066696383, 0.000000000000000000, 13.31285208727739899 ) ) ;
#31539 = CARTESIAN_POINT ( 'NONE',  ( -31.72626587586518099, 0.000000000000000000, 9.005490826201270949 ) ) ;
#31540 = EDGE_CURVE ( 'NONE', #52053, #15174, #34874, .T. ) ;
#31541 = CARTESIAN_POINT ( 'NONE',  ( -18.15283808406918098, -3.917936722690662954, 3.807497207905658154 ) ) ;
#31542 = PLANE ( 'NONE',  #30188 ) ;
#31543 = ORIENTED_EDGE ( 'NONE', *, *, #14297, .F. ) ;
#31544 = VECTOR ( 'NONE', #11556, 1000.000000000000227 ) ;
#31545 = ORIENTED_EDGE ( 'NONE', *, *, #34783, .T. ) ;
#31546 = EDGE_CURVE ( 'NONE', #35148, #42919, #52728, .T. ) ;
#31547 = LINE ( 'NONE', #6261, #55880 ) ;
#31548 = DIRECTION ( 'NONE',  ( -0.9997703818010067467, 0.000000000000000000, 0.02142857142857158143 ) ) ;
#31549 = EDGE_CURVE ( 'NONE', #42286, #21767, #30633, .T. ) ;
#31550 = VECTOR ( 'NONE', #56030, 999.9999999999998863 ) ;
#31551 = ORIENTED_EDGE ( 'NONE', *, *, #33796, .T. ) ;
#31552 = CARTESIAN_POINT ( 'NONE',  ( -29.86352658060627618, 0.000000000000000000, 8.481329010720569883 ) ) ;
#31553 = EDGE_CURVE ( 'NONE', #25397, #52695, #47934, .T. ) ;
#31554 = EDGE_LOOP ( 'NONE', ( #45860, #41782, #10755, #25893 ) ) ;
#31555 = LINE ( 'NONE', #28107, #15656 ) ;
#31556 = ORIENTED_EDGE ( 'NONE', *, *, #17647, .T. ) ;
#31557 = ORIENTED_EDGE ( 'NONE', *, *, #5405, .F. ) ;
#31558 = ORIENTED_EDGE ( 'NONE', *, *, #8411, .T. ) ;
#31559 = CARTESIAN_POINT ( 'NONE',  ( -16.00875351199029240, 0.000000000000000000, 5.634493499890388613 ) ) ;
#31560 = DIRECTION ( 'NONE',  ( 0.007781995580012662783, 0.000000000000000000, -0.9999697198139514409 ) ) ;
#31561 = DIRECTION ( 'NONE',  ( 0.000000000000000000, -5.782411586589354681E-16, 1.000000000000000000 ) ) ;
#31562 = LINE ( 'NONE', #9117, #47526 ) ;
#31563 = ORIENTED_EDGE ( 'NONE', *, *, #30459, .F. ) ;
#31564 = ORIENTED_EDGE ( 'NONE', *, *, #33166, .T. ) ;
#31565 = EDGE_CURVE ( 'NONE', #15218, #17024, #56169, .T. ) ;
#31566 = CARTESIAN_POINT ( 'NONE',  ( -20.07452495636445633, -3.432230869623159819, 4.569442209528198795 ) ) ;
#31567 = ORIENTED_EDGE ( 'NONE', *, *, #30287, .F. ) ;
#31568 = FACE_OUTER_BOUND ( 'NONE', #15596, .T. ) ;
#31569 = ADVANCED_FACE ( 'NONE', ( #30878 ), #17255, .F. ) ;
#31570 = ORIENTED_EDGE ( 'NONE', *, *, #37437, .T. ) ;
#31571 = CARTESIAN_POINT ( 'NONE',  ( 0.3240706152708106025, -3.670543518250628967, -1.335466778558061241E-15 ) ) ;
#31572 = CARTESIAN_POINT ( 'NONE',  ( -16.93802730567246329, 0.000000000000000000, 5.627261676354369691 ) ) ;
#31573 = ORIENTED_EDGE ( 'NONE', *, *, #50726, .F. ) ;
#31574 = ADVANCED_FACE ( 'NONE', ( #49325 ), #53328, .F. ) ;
#31575 = CARTESIAN_POINT ( 'NONE',  ( -24.74852218546340410, 18.25476860917765620, -4.557895514311181451 ) ) ;
#31576 = EDGE_LOOP ( 'NONE', ( #51802, #36560, #30258, #52908 ) ) ;
#31577 = EDGE_CURVE ( 'NONE', #5343, #49645, #19784, .T. ) ;
#31578 = EDGE_CURVE ( 'NONE', #45628, #9765, #19498, .T. ) ;
#31579 = CARTESIAN_POINT ( 'NONE',  ( -25.20123094555300369, 0.000000000000000000, 6.470945668149052032 ) ) ;
#31580 = EDGE_LOOP ( 'NONE', ( #17157, #18578, #50313, #53758 ) ) ;
#31581 = CARTESIAN_POINT ( 'NONE',  ( -19.25390728375132099, 0.000000000000000000, 4.670568767036004765 ) ) ;
#31582 = CARTESIAN_POINT ( 'NONE',  ( -12.69021377840191533, -0.1941918491731548790, 1.929943632359736538 ) ) ;
#31583 = DIRECTION ( 'NONE',  ( -0.5449076811759708816, 0.6444004775717707689, 0.5364919789714475140 ) ) ;
#31584 = ORIENTED_EDGE ( 'NONE', *, *, #719, .T. ) ;
#31585 = VECTOR ( 'NONE', #3837, 1000.000000000000227 ) ;
#31586 = PRODUCT_RELATED_PRODUCT_CATEGORY ( 'part', '', ( #53221 ) ) ;
#31587 = DIRECTION ( 'NONE',  ( -0.6427681459581293666, -0.7660444431189770143, -0.005002170337467561935 ) ) ;
#31588 = CARTESIAN_POINT ( 'NONE',  ( -16.47626446233665831, 0.000000000000000000, 6.000187291380142618 ) ) ;
#31589 = LINE ( 'NONE', #27594, #29549 ) ;
#31590 = DIRECTION ( 'NONE',  ( -0.005961354470445682716, -0.6427876096865404731, 0.7660212471507180654 ) ) ;
#31591 = CARTESIAN_POINT ( 'NONE',  ( -24.26908309836554878, 0.000000000000000000, 6.108867788427308376 ) ) ;
#31592 = EDGE_CURVE ( 'NONE', #15287, #14766, #24042, .T. ) ;
#31593 = CARTESIAN_POINT ( 'NONE',  ( -68.02159960128747684, -9.628770505094481180, 5.304050906517969288 ) ) ;
#31594 = ORIENTED_EDGE ( 'NONE', *, *, #13055, .F. ) ;
#31595 = CARTESIAN_POINT ( 'NONE',  ( -15.13495153988577968, 0.000000000000000000, 12.76973526769478084 ) ) ;
#31596 = DIRECTION ( 'NONE',  ( 0.007781995580012663651, -3.146120232559066537E-19, -0.9999697198139514409 ) ) ;
#31597 = DIRECTION ( 'NONE',  ( 0.005961354470445682716, -0.6427876096865404731, -0.7660212471507180654 ) ) ;
#31598 = VERTEX_POINT ( 'NONE', #44784 ) ;
#31599 = FACE_OUTER_BOUND ( 'NONE', #14025, .T. ) ;
#31600 = CARTESIAN_POINT ( 'NONE',  ( -18.23116282465632310, -0.1191753592594167882, 5.517195168626942703 ) ) ;
#31601 = VERTEX_POINT ( 'NONE', #2162 ) ;
#31602 = CARTESIAN_POINT ( 'NONE',  ( -18.19747506107908563, 0.000000000000000000, 14.03856424583689311 ) ) ;
#31603 = CARTESIAN_POINT ( 'NONE',  ( -19.62714374037757636, 0.4483081953215045656, 4.291477522278790424 ) ) ;
#31604 = DIRECTION ( 'NONE',  ( 0.7660212471507180654, -0.6427876096865404731, 0.005961354470445141482 ) ) ;
#31605 = DIRECTION ( 'NONE',  ( 0.5449076811759707706, 0.6444004775717708799, -0.5364919789714476250 ) ) ;
#31606 = ORIENTED_EDGE ( 'NONE', *, *, #28868, .F. ) ;
#31607 = ORIENTED_EDGE ( 'NONE', *, *, #14001, .T. ) ;
#31608 = CARTESIAN_POINT ( 'NONE',  ( -14.93495759592298988, 0.000000000000000000, 12.77129166681078409 ) ) ;
#31609 = CARTESIAN_POINT ( 'NONE',  ( -16.53317331066696383, 0.000000000000000000, 13.31285208727739899 ) ) ;
#31610 = CARTESIAN_POINT ( 'NONE',  ( -16.48045617023122134, 0.000000000000000000, 6.538812753932882416 ) ) ;
#31611 = PLANE ( 'NONE',  #42903 ) ;
#31612 = DIRECTION ( 'NONE',  ( 0.005961354470445682716, -0.6427876096865404731, -0.7660212471507180654 ) ) ;
#31613 = VERTEX_POINT ( 'NONE', #10971 ) ;
#31614 = LINE ( 'NONE', #10017, #4105 ) ;
#31615 = ADVANCED_FACE ( 'NONE', ( #6189 ), #28289, .F. ) ;
#31616 = ORIENTED_EDGE ( 'NONE', *, *, #18108, .F. ) ;
#31617 = CARTESIAN_POINT ( 'NONE',  ( -15.13495153988577968, 0.000000000000000000, 12.76973526769478084 ) ) ;
#31618 = LINE ( 'NONE', #9764, #55973 ) ;
#31619 = EDGE_LOOP ( 'NONE', ( #7202, #26180, #4862, #23245 ) ) ;
#31620 = DIRECTION ( 'NONE',  ( 0.3313982828793700097, 0.4028455766673916805, 0.8531650599175528704 ) ) ;
#31621 = DIRECTION ( 'NONE',  ( 0.000000000000000000, -1.000000000000000000, 0.000000000000000000 ) ) ;
#31622 = DIRECTION ( 'NONE',  ( 0.007781995580012663651, -3.146120232559066537E-19, -0.9999697198139514409 ) ) ;
#31623 = EDGE_CURVE ( 'NONE', #23133, #21974, #41074, .T. ) ;
#31624 = VERTEX_POINT ( 'NONE', #32304 ) ;
#31625 = AXIS2_PLACEMENT_3D ( 'NONE', #42670, #29914, #12595 ) ;
#31626 = FACE_OUTER_BOUND ( 'NONE', #8500, .T. ) ;
#31627 = ORIENTED_EDGE ( 'NONE', *, *, #5695, .T. ) ;
#31628 = EDGE_CURVE ( 'NONE', #45792, #10825, #37105, .T. ) ;
#31629 = EDGE_CURVE ( 'NONE', #27319, #44456, #36844, .T. ) ;
#31630 = VERTEX_POINT ( 'NONE', #41374 ) ;
#31631 = VERTEX_POINT ( 'NONE', #10727 ) ;
#31632 = ORIENTED_EDGE ( 'NONE', *, *, #40581, .F. ) ;
#31633 = DIRECTION ( 'NONE',  ( 0.6427681459581294776, -0.7660444431189769032, 0.005002170337467562802 ) ) ;
#31634 = EDGE_CURVE ( 'NONE', #35152, #25894, #22923, .T. ) ;
#31635 = B_SPLINE_CURVE_WITH_KNOTS ( 'NONE', 1,
 ( #28627, #24355 ),
 .UNSPECIFIED., .F., .F.,
 ( 2, 2 ),
 ( 0.001874228446202059594, 0.003011459512596941206 ),
 .UNSPECIFIED. ) ;
#31636 = ORIENTED_EDGE ( 'NONE', *, *, #23891, .T. ) ;
#31637 = DIRECTION ( 'NONE',  ( 0.5449076811759707706, 0.6444004775717708799, -0.5364919789714476250 ) ) ;
#31638 = LINE ( 'NONE', #18263, #3232 ) ;
#31639 = ORIENTED_EDGE ( 'NONE', *, *, #46063, .F. ) ;
#31640 = EDGE_CURVE ( 'NONE', #27257, #17489, #9881, .T. ) ;
#31641 = ORIENTED_EDGE ( 'NONE', *, *, #46076, .F. ) ;
#31642 = CARTESIAN_POINT ( 'NONE',  ( -19.72584868671897596, 0.000000000000000000, 5.605566205746312036 ) ) ;
#31643 = VERTEX_POINT ( 'NONE', #19204 ) ;
#31644 = ADVANCED_FACE ( 'NONE', ( #2465 ), #32827, .F. ) ;
#31645 = CARTESIAN_POINT ( 'NONE',  ( -11.60492197282151139, -1.651309408375657428, 3.899757593961617808 ) ) ;
#31646 = DIRECTION ( 'NONE',  ( -0.005961354470445682716, -0.6427876096865404731, 0.7660212471507180654 ) ) ;
#31647 = CARTESIAN_POINT ( 'NONE',  ( -19.12962290826653700, 0.000000000000000000, 14.40064212555863854 ) ) ;
#31648 = LINE ( 'NONE', #48380, #3962 ) ;
#31649 = CARTESIAN_POINT ( 'NONE',  ( -21.00667280355191124, -3.432230869623159819, 4.931520089249944228 ) ) ;
#31650 = CARTESIAN_POINT ( 'NONE',  ( -29.86352658060627618, 0.000000000000000000, 8.481329010720569883 ) ) ;
#31651 = ORIENTED_EDGE ( 'NONE', *, *, #23456, .T. ) ;
#31652 = EDGE_CURVE ( 'NONE', #41949, #27295, #36021, .T. ) ;
#31653 = ORIENTED_EDGE ( 'NONE', *, *, #3925, .F. ) ;
#31654 = DIRECTION ( 'NONE',  ( -0.6427681459581293666, -0.7660444431189770143, -0.005002170337467561935 ) ) ;
#31655 = DIRECTION ( 'NONE',  ( 0.007781995580012663651, -3.146120232559066537E-19, -0.9999697198139514409 ) ) ;
#31656 = FACE_OUTER_BOUND ( 'NONE', #22185, .T. ) ;
#31657 = EDGE_CURVE ( 'NONE', #1914, #31885, #10439, .T. ) ;
#31658 = CARTESIAN_POINT ( 'NONE',  ( -24.53375310857961367, 18.49370688441070953, 4.545578210335888159 ) ) ;
#31659 = ORIENTED_EDGE ( 'NONE', *, *, #55833, .T. ) ;
#31660 = DIRECTION ( 'NONE',  ( -0.7886751345948130876, 0.2113248654051844977, -0.5773502691896263972 ) ) ;
#31661 = LINE ( 'NONE', #18588, #17794 ) ;
#31662 = VERTEX_POINT ( 'NONE', #18677 ) ;
#31663 = FACE_OUTER_BOUND ( 'NONE', #3887, .T. ) ;
#31664 = CARTESIAN_POINT ( 'NONE',  ( -20.10727089963316061, 4.819660872929009798, 12.60155257131766859 ) ) ;
#31665 = ORIENTED_EDGE ( 'NONE', *, *, #19421, .F. ) ;
#31666 = COLOUR_RGB ( '', 0.40784314, 0.44705882, 0.49803922) ;
#31667 = CARTESIAN_POINT ( 'NONE',  ( -68.17944635737889314, -8.907771540513445885, 6.097755213354407289 ) ) ;
#31668 = DIRECTION ( 'NONE',  ( 0.005002170337468016433, -0.7660444431189770143, -0.6427681459581293666 ) ) ;
#31669 = DIRECTION ( 'NONE',  ( 0.007781995580012663651, 0.000000000000000000, -0.9999697198139515519 ) ) ;
#31670 = DIRECTION ( 'NONE',  ( 0.000000000000000000, -0.000000000000000000, -1.000000000000000000 ) ) ;
#31671 = CARTESIAN_POINT ( 'NONE',  ( -20.31522615006396038, 5.143464774974012776, 4.408952020843655895 ) ) ;
#31672 = VERTEX_POINT ( 'NONE', #32004 ) ;
#31673 = ORIENTED_EDGE ( 'NONE', *, *, #34451, .T. ) ;
#31674 = DIRECTION ( 'NONE',  ( 0.6427681459581294776, -0.7660444431189769032, 0.005002170337467562802 ) ) ;
#31675 = PLANE ( 'NONE',  #17695 ) ;
#31676 = FACE_OUTER_BOUND ( 'NONE', #10042, .T. ) ;
#31677 = CARTESIAN_POINT ( 'NONE',  ( -9.769797563482667258, 0.000000000000000000, 5.852372511285491186 ) ) ;
#31678 = CARTESIAN_POINT ( 'NONE',  ( -25.20200914511100265, -0.1191753592594197858, 6.570942640130446932 ) ) ;
#31679 = ADVANCED_FACE ( 'NONE', ( #1631 ), #45086, .F. ) ;
#31680 = ORIENTED_EDGE ( 'NONE', *, *, #21392, .F. ) ;
#31681 = CARTESIAN_POINT ( 'NONE',  ( -14.70243142924463875, 24.16982310246453380, -3.792938838976426918 ) ) ;
#31682 = LINE ( 'NONE', #41762, #41094 ) ;
#31683 = DIRECTION ( 'NONE',  ( -0.9999697198139514409, -0.000000000000000000, -0.007781995580013368816 ) ) ;
#31684 = LINE ( 'NONE', #6395, #27854 ) ;
#31685 = ORIENTED_EDGE ( 'NONE', *, *, #12644, .T. ) ;
#31686 = DIRECTION ( 'NONE',  ( 0.5449076811759707706, 0.6444004775717708799, -0.5364919789714476250 ) ) ;
#31687 = ORIENTED_EDGE ( 'NONE', *, *, #5224, .T. ) ;
#31688 = DIRECTION ( 'NONE',  ( 0.5364919789714477361, 0.6444004775717706579, 0.5449076811759711036 ) ) ;
#31689 = ADVANCED_FACE ( 'NONE', ( #23223 ), #40550, .F. ) ;
#31690 = EDGE_CURVE ( 'NONE', #14373, #52348, #3842, .T. ) ;
#31691 = LINE ( 'NONE', #5007, #26623 ) ;
#31692 = ORIENTED_EDGE ( 'NONE', *, *, #13350, .F. ) ;
#31693 = DIRECTION ( 'NONE',  ( -0.9999697198139514409, -0.000000000000000000, -0.007781995580013368816 ) ) ;
#31694 = ORIENTED_EDGE ( 'NONE', *, *, #34221, .T. ) ;
#31695 = EDGE_CURVE ( 'NONE', #38002, #27953, #11805, .T. ) ;
#31696 = EDGE_LOOP ( 'NONE', ( #24005, #36567, #38368, #31709 ) ) ;
#31697 = ORIENTED_EDGE ( 'NONE', *, *, #7457, .T. ) ;
#31698 = CARTESIAN_POINT ( 'NONE',  ( -28.93137873341882127, 0.000000000000000000, 8.119251130998824451 ) ) ;
#31699 = ORIENTED_EDGE ( 'NONE', *, *, #43124, .F. ) ;
#31700 = ORIENTED_EDGE ( 'NONE', *, *, #27188, .T. ) ;
#31701 = FACE_OUTER_BOUND ( 'NONE', #13927, .T. ) ;
#31702 = PLANE ( 'NONE',  #4095 ) ;
#31703 = VERTEX_POINT ( 'NONE', #38204 ) ;
#31704 = EDGE_CURVE ( 'NONE', #37525, #20361, #19642, .T. ) ;
#31705 = EDGE_LOOP ( 'NONE', ( #34411, #11423, #16882, #18872 ) ) ;
#31706 = CARTESIAN_POINT ( 'NONE',  ( -18.32618988918515512, 0.000000000000000000, 4.877794534534811710 ) ) ;
#31707 = EDGE_CURVE ( 'NONE', #38106, #35325, #20632, .T. ) ;
#31708 = EDGE_LOOP ( 'NONE', ( #9033, #32321, #33922, #21428 ) ) ;
#31709 = ORIENTED_EDGE ( 'NONE', *, *, #34854, .F. ) ;
#31710 = ADVANCED_FACE ( 'NONE', ( #46739 ), #29420, .F. ) ;
#31711 = CARTESIAN_POINT ( 'NONE',  ( -27.99845268667336384, -0.1191753592594197858, 7.657176279295684118 ) ) ;
#31712 = DIRECTION ( 'NONE',  ( 0.007781995580012663651, -3.146120232559066537E-19, -0.9999697198139514409 ) ) ;
#31713 = EDGE_CURVE ( 'NONE', #51394, #34166, #16629, .T. ) ;
#31714 = LINE ( 'NONE', #49017, #31434 ) ;
#31715 = CARTESIAN_POINT ( 'NONE',  ( -68.13647802434893208, -11.18517250923651574, -7.477522605581023996 ) ) ;
#31716 = ORIENTED_EDGE ( 'NONE', *, *, #35407, .F. ) ;
#31717 = LINE ( 'NONE', #10120, #21976 ) ;
#31718 = ORIENTED_EDGE ( 'NONE', *, *, #52873, .F. ) ;
#31719 = ADVANCED_FACE ( 'NONE', ( #46430 ), #3573, .F. ) ;
#31720 = DIRECTION ( 'NONE',  ( 0.7660212471507180654, -0.6427876096865404731, 0.005961354470445141482 ) ) ;
#31721 = DIRECTION ( 'NONE',  ( 0.6427681459581294776, -0.7660444431189769032, 0.005002170337467562802 ) ) ;
#31722 = CARTESIAN_POINT ( 'NONE',  ( -67.33383789142597209, 0.1329135175168457139, -0.6948190221874496197 ) ) ;
#31723 = FACE_OUTER_BOUND ( 'NONE', #16746, .T. ) ;
#31724 = CARTESIAN_POINT ( 'NONE',  ( -22.40478740399063895, 0.000000000000000000, 5.384712028983816623 ) ) ;
#31725 = CARTESIAN_POINT ( 'NONE',  ( -22.38231225002310865, -5.536956232915663634, 14.46307039415223272 ) ) ;
#31726 = ORIENTED_EDGE ( 'NONE', *, *, #54325, .F. ) ;
#31727 = CARTESIAN_POINT ( 'NONE',  ( -10.43155435078125670, 0.000000000000000000, 5.477890497143714121 ) ) ;
#31728 = ORIENTED_EDGE ( 'NONE', *, *, #46601, .T. ) ;
#31729 = CARTESIAN_POINT ( 'NONE',  ( -13.17065887352947762, -0.1191753592594197858, 12.04635770780929427 ) ) ;
#31730 = DIRECTION ( 'NONE',  ( 0.007781995580012662783, 0.000000000000000000, -0.9999697198139514409 ) ) ;
#31731 = DIRECTION ( 'NONE',  ( -0.9999697198139514409, -0.000000000000000000, -0.007781995580013368816 ) ) ;
#31732 = CARTESIAN_POINT ( 'NONE',  ( -16.84874834815419575, -0.1191753592594177180, 7.005281716962028504 ) ) ;
#31733 = DIRECTION ( 'NONE',  ( -0.7660212471507179544, -0.6427876096865405842, -0.005961354470445141482 ) ) ;
#31734 = CARTESIAN_POINT ( 'NONE',  ( -69.12566734621377407, -1.678475092257100935E-13, 7.875383342262419539 ) ) ;
#31735 = EDGE_LOOP ( 'NONE', ( #29805, #6971, #25070, #48138 ) ) ;
#31736 = PLANE ( 'NONE',  #54704 ) ;
#31737 = DIRECTION ( 'NONE',  ( 0.005961354470445682716, -0.6427876096865404731, -0.7660212471507180654 ) ) ;
#31738 = DIRECTION ( 'NONE',  ( -0.5364919789714478471, 0.6444004775717705469, -0.5449076811759709926 ) ) ;
#31739 = B_SPLINE_CURVE_WITH_KNOTS ( 'NONE', 3,
 ( #39196, #16490, #29586, #55682 ),
 .UNSPECIFIED., .F., .F.,
 ( 4, 4 ),
 ( 0.0002809688904423142679, 0.0003536739149152803505 ),
 .UNSPECIFIED. ) ;
#31740 = EDGE_CURVE ( 'NONE', #22414, #30649, #33664, .T. ) ;
#31741 = PLANE ( 'NONE',  #33707 ) ;
#31742 = DIRECTION ( 'NONE',  ( -0.005961354470445682716, -0.6427876096865404731, 0.7660212471507180654 ) ) ;
#31743 = ADVANCED_FACE ( 'NONE', ( #51285 ), #12398, .F. ) ;
#31744 = CARTESIAN_POINT ( 'NONE',  ( -18.63227683361970577, -2.784623065533159636, 8.489381659524488200 ) ) ;
#31745 = DIRECTION ( 'NONE',  ( -0.5449076811759708816, 0.6444004775717707689, 0.5364919789714475140 ) ) ;
#31746 = CARTESIAN_POINT ( 'NONE',  ( -23.29661994227107868, 19.01267450544941084, 4.488313114961025363 ) ) ;
#31747 = EDGE_CURVE ( 'NONE', #24350, #33683, #47023, .T. ) ;
#31748 = CARTESIAN_POINT ( 'NONE',  ( -12.15720038968843575, -0.1166911823299083412, 1.503895915954261975 ) ) ;
#31749 = EDGE_CURVE ( 'NONE', #26892, #6017, #37664, .T. ) ;
#31750 = EDGE_CURVE ( 'NONE', #22811, #40865, #16935, .T. ) ;
#31751 = EDGE_CURVE ( 'NONE', #47218, #50133, #38492, .T. ) ;
#31752 = ORIENTED_EDGE ( 'NONE', *, *, #6151, .F. ) ;
#31753 = EDGE_CURVE ( 'NONE', #39017, #36677, #28578, .T. ) ;
#31754 = ORIENTED_EDGE ( 'NONE', *, *, #46138, .T. ) ;
#31755 = ORIENTED_EDGE ( 'NONE', *, *, #33930, .T. ) ;
#31756 = VERTEX_POINT ( 'NONE', #24578 ) ;
#31757 = VERTEX_POINT ( 'NONE', #45903 ) ;
#31758 = CARTESIAN_POINT ( 'NONE',  ( -18.76354595665420177, -0.1191753592594177458, 14.21882498613976331 ) ) ;
#31759 = CARTESIAN_POINT ( 'NONE',  ( -67.81506811452879901, 0.000000000000000000, -7.454891809856698970 ) ) ;
#31760 = ORIENTED_EDGE ( 'NONE', *, *, #6156, .F. ) ;
#31761 = VERTEX_POINT ( 'NONE', #7020 ) ;
#31762 = ORIENTED_EDGE ( 'NONE', *, *, #46878, .F. ) ;
#31763 = AXIS2_PLACEMENT_3D ( 'NONE', #52979, #45039, #32255 ) ;
#31764 = EDGE_CURVE ( 'NONE', #38002, #26378, #24323, .T. ) ;
#31765 = CARTESIAN_POINT ( 'NONE',  ( -14.20280369269832832, 0.000000000000000000, 12.40765738797303719 ) ) ;
#31766 = EDGE_CURVE ( 'NONE', #46034, #19226, #2711, .T. ) ;
#31767 = PLANE ( 'NONE',  #10114 ) ;
#31768 = LINE ( 'NONE', #550, #47718 ) ;
#31769 = VERTEX_POINT ( 'NONE', #7551 ) ;
#31770 = CARTESIAN_POINT ( 'NONE',  ( -18.86354292863559579, 0.000000000000000000, 14.21804678658176080 ) ) ;
#31771 = ORIENTED_EDGE ( 'NONE', *, *, #26546, .T. ) ;
#31772 = EDGE_CURVE ( 'NONE', #24424, #34779, #16085, .T. ) ;
#31773 = PLANE ( 'NONE',  #50890 ) ;
#31774 = DIRECTION ( 'NONE',  ( 0.9999697198139515519, 0.000000000000000000, 0.007781995580013368816 ) ) ;
#31775 = EDGE_CURVE ( 'NONE', #23847, #49612, #20327, .T. ) ;
#31776 = LINE ( 'NONE', #49081, #40904 ) ;
#31777 = DIRECTION ( 'NONE',  ( 0.6427681459581294776, -0.7660444431189769032, 0.005002170337467562802 ) ) ;
#31778 = DIRECTION ( 'NONE',  ( -0.5449076811759708816, 0.6444004775717707689, 0.5364919789714475140 ) ) ;
#31779 = DIRECTION ( 'NONE',  ( 0.7660212471507180654, -0.6427876096865404731, 0.005961354470445141482 ) ) ;
#31780 = DIRECTION ( 'NONE',  ( 0.005002170337468016433, -0.7660444431189770143, -0.6427681459581293666 ) ) ;
#31781 = ORIENTED_EDGE ( 'NONE', *, *, #27381, .T. ) ;
#31782 = DIRECTION ( 'NONE',  ( 0.007781995580012662783, 0.000000000000000000, -0.9999697198139514409 ) ) ;
#31783 = VERTEX_POINT ( 'NONE', #13505 ) ;
#31784 = CARTESIAN_POINT ( 'NONE',  ( -17.74560456716937296, 0.000000000000000000, 3.774316574337878372 ) ) ;
#31785 = CARTESIAN_POINT ( 'NONE',  ( -17.46532115785441519, 0.000000000000000000, 13.67492996699914265 ) ) ;
#31786 = LINE ( 'NONE', #574, #20403 ) ;
#31787 = DIRECTION ( 'NONE',  ( 0.6427681459581294776, -0.7660444431189769032, 0.005002170337467562802 ) ) ;
#31788 = DIRECTION ( 'NONE',  ( 0.6427681459581294776, -0.7660444431189769032, 0.005002170337467562802 ) ) ;
#31789 = PLANE ( 'NONE',  #24926 ) ;
#31790 = LINE ( 'NONE', #10202, #45193 ) ;
#31791 = LINE ( 'NONE', #23287, #6554 ) ;
#31792 = DIRECTION ( 'NONE',  ( 0.007781995580012662783, 0.000000000000000000, -0.9999697198139514409 ) ) ;
#31793 = EDGE_LOOP ( 'NONE', ( #30702, #55753, #15576, #39614 ) ) ;
#31794 = DIRECTION ( 'NONE',  ( 0.007781995580012663651, -3.146120232559066537E-19, -0.9999697198139514409 ) ) ;
#31795 = FACE_OUTER_BOUND ( 'NONE', #32176, .T. ) ;
#31796 = CARTESIAN_POINT ( 'NONE',  ( -12.60458797795435615, 0.000000000000000000, 11.86609696750642229 ) ) ;
#31797 = DIRECTION ( 'NONE',  ( 0.005961354470445682716, -0.6427876096865404731, -0.7660212471507180654 ) ) ;
#31798 = FACE_OUTER_BOUND ( 'NONE', #6279, .T. ) ;
#31799 = DIRECTION ( 'NONE',  ( -0.3583679495452925523, -0.9335804264972047406, -0.000000000000000000 ) ) ;
#31800 = DIRECTION ( 'NONE',  ( 0.9999697198139515519, 0.000000000000000000, 0.007781995580013368816 ) ) ;
#31801 = VERTEX_POINT ( 'NONE', #17772 ) ;
#31802 = AXIS2_PLACEMENT_3D ( 'NONE', #18165, #52797, #13905 ) ;
#31803 = ORIENTED_EDGE ( 'NONE', *, *, #54497, .F. ) ;
#31804 = DIRECTION ( 'NONE',  ( -0.5449076811759708816, 0.6444004775717707689, 0.5364919789714475140 ) ) ;
#31805 = CARTESIAN_POINT ( 'NONE',  ( -18.86354292863559579, 0.000000000000000000, 14.21804678658176080 ) ) ;
#31806 = EDGE_CURVE ( 'NONE', #3481, #46828, #30820, .T. ) ;
#31807 = EDGE_CURVE ( 'NONE', #8140, #13801, #21741, .T. ) ;
#31808 = ORIENTED_EDGE ( 'NONE', *, *, #12662, .T. ) ;
#31809 = CARTESIAN_POINT ( 'NONE',  ( 2.072287782118878319, 0.000000000000000000, -2.950529333540147015 ) ) ;
#31810 = ORIENTED_EDGE ( 'NONE', *, *, #1578, .F. ) ;
#31811 = FACE_OUTER_BOUND ( 'NONE', #24473, .T. ) ;
#31812 = ADVANCED_FACE ( 'NONE', ( #12933 ), #22313, .F. ) ;
#31813 = ORIENTED_EDGE ( 'NONE', *, *, #54287, .T. ) ;
#31814 = ORIENTED_EDGE ( 'NONE', *, *, #39639, .F. ) ;
#31815 = ORIENTED_EDGE ( 'NONE', *, *, #52886, .F. ) ;
#31816 = CARTESIAN_POINT ( 'NONE',  ( -15.05682940326283514, -1.327505506330655782, 4.709178299313876437 ) ) ;
#31817 = CARTESIAN_POINT ( 'NONE',  ( -20.90639117353077125, -1.651309408375658760, 4.949388017332537970 ) ) ;
#31818 = PLANE ( 'NONE',  #3053 ) ;
#31819 = VECTOR ( 'NONE', #48594, 1000.000000000000114 ) ;
#31820 = CARTESIAN_POINT ( 'NONE',  ( -19.60990026154428278, 0.000000000000000000, 4.498472333781370125 ) ) ;
#31821 = ORIENTED_EDGE ( 'NONE', *, *, #26546, .F. ) ;
#31822 = ORIENTED_EDGE ( 'NONE', *, *, #20953, .F. ) ;
#31823 = LINE ( 'NONE', #15080, #55394 ) ;
#31824 = ORIENTED_EDGE ( 'NONE', *, *, #42151, .T. ) ;
#31825 = DIRECTION ( 'NONE',  ( -0.6427681459581293666, -0.7660444431189770143, -0.005002170337467561935 ) ) ;
#31826 = VERTEX_POINT ( 'NONE', #31085 ) ;
#31827 = CARTESIAN_POINT ( 'NONE',  ( -17.24632744471935908, 4.819660872929012463, 3.227218583223867121 ) ) ;
#31828 = PLANE ( 'NONE',  #7678 ) ;
#31829 = ORIENTED_EDGE ( 'NONE', *, *, #19334, .F. ) ;
#31830 = VECTOR ( 'NONE', #16751, 1000.000000000000000 ) ;
#31831 = CARTESIAN_POINT ( 'NONE',  ( -16.86886672269117682, -0.1191753592594181482, 9.590449639766383427 ) ) ;
#31832 = ORIENTED_EDGE ( 'NONE', *, *, #42466, .T. ) ;
#31833 = ADVANCED_FACE ( 'NONE', ( #8700 ), #22586, .F. ) ;
#31834 = VECTOR ( 'NONE', #40556, 1000.000000000000227 ) ;
#31835 = CARTESIAN_POINT ( 'NONE',  ( 2.072287782118878319, 0.000000000000000000, -2.950529333540147015 ) ) ;
#31837 = EDGE_CURVE ( 'NONE', #39606, #20246, #17464, .T. ) ;
#31836 = ORIENTED_EDGE ( 'NONE', *, *, #21151, .T. ) ;
#31838 = DIRECTION ( 'NONE',  ( 0.000000000000000000, -0.000000000000000000, -1.000000000000000000 ) ) ;
#31839 = DIRECTION ( 'NONE',  ( -0.5364919789714478471, 0.6444004775717705469, -0.5449076811759709926 ) ) ;
#31840 = DIRECTION ( 'NONE',  ( 0.5449076811759707706, 0.6444004775717708799, -0.5364919789714476250 ) ) ;
#31841 = ORIENTED_EDGE ( 'NONE', *, *, #55088, .T. ) ;
#31842 = CARTESIAN_POINT ( 'NONE',  ( -30.79411802867772607, 0.000000000000000000, 8.643412946479525516 ) ) ;
#31843 = CARTESIAN_POINT ( 'NONE',  ( -19.72297463321369548, 0.000000000000000000, 5.236256502488546793 ) ) ;
#31844 = EDGE_CURVE ( 'NONE', #48219, #3085, #52408, .T. ) ;
#31845 = DIRECTION ( 'NONE',  ( 0.000000000000000000, -1.000000000000000000, 0.000000000000000000 ) ) ;
#31846 = DIRECTION ( 'NONE',  ( -0.005961354470445682716, -0.6427876096865404731, 0.7660212471507180654 ) ) ;
#31847 = DIRECTION ( 'NONE',  ( 0.7660212471507180654, -0.6427876096865404731, 0.005961354470445141482 ) ) ;
#31848 = CARTESIAN_POINT ( 'NONE',  ( -12.67829634397052097, -0.1159828484229817602, 8.143054432418114885 ) ) ;
#31849 = CARTESIAN_POINT ( 'NONE',  ( -67.67563256367881763, -11.46835534393823686, -5.350280945795687693 ) ) ;
#31850 = EDGE_LOOP ( 'NONE', ( #52758, #7306, #25955, #37819 ) ) ;
#31851 = CARTESIAN_POINT ( 'NONE',  ( -20.54204810873173415, 0.000000000000000000, 4.860550213503115558 ) ) ;
#31852 = CARTESIAN_POINT ( 'NONE',  ( -28.92982233430281980, 0.000000000000000000, 7.919257187036034651 ) ) ;
#31853 = CARTESIAN_POINT ( 'NONE',  ( -65.91359709181411120, -3.035766082959412415E-14, 3.032081494009100986 ) ) ;
#31854 = ORIENTED_EDGE ( 'NONE', *, *, #40489, .F. ) ;
#31855 = DIRECTION ( 'NONE',  ( 0.5449076811759707706, 0.6444004775717708799, -0.5364919789714476250 ) ) ;
#31856 = LINE ( 'NONE', #27902, #11837 ) ;
#31857 = ORIENTED_EDGE ( 'NONE', *, *, #7068, .T. ) ;
#31858 = CIRCLE ( 'NONE', #7361, 0.5000000000000004441 ) ;
#31859 = VECTOR ( 'NONE', #7059, 999.9999999999998863 ) ;
#31860 = CARTESIAN_POINT ( 'NONE',  ( -12.08148583366696727, 0.000000000000000000, 4.357054139414387350 ) ) ;
#31861 = CARTESIAN_POINT ( 'NONE',  ( -2.428019651919397948, -4.270454567941153634, -2.275248286963848177 ) ) ;
#31862 = PLANE ( 'NONE',  #48331 ) ;
#31863 = ORIENTED_EDGE ( 'NONE', *, *, #43055, .T. ) ;
#31864 = VERTEX_POINT ( 'NONE', #56108 ) ;
#31865 = FACE_OUTER_BOUND ( 'NONE', #42346, .T. ) ;
#31866 = LINE ( 'NONE', #49484, #29638 ) ;
#31867 = EDGE_CURVE ( 'NONE', #2943, #10990, #34509, .T. ) ;
#31868 = DIRECTION ( 'NONE',  ( -0.5449076811759708816, 0.6444004775717707689, 0.5364919789714475140 ) ) ;
#31869 = ADVANCED_FACE ( 'NONE', ( #125 ), #43337, .F. ) ;
#31870 = CARTESIAN_POINT ( 'NONE',  ( -22.40634380310664397, 0.000000000000000000, 5.584705972946605534 ) ) ;
#31871 = EDGE_LOOP ( 'NONE', ( #46867, #33985, #30163, #9199 ) ) ;
#31872 = DIRECTION ( 'NONE',  ( 0.9999697198139515519, 0.000000000000000000, 0.007781995580013368816 ) ) ;
#31873 = ORIENTED_EDGE ( 'NONE', *, *, #38978, .T. ) ;
#31874 = PLANE ( 'NONE',  #26535 ) ;
#31875 = ADVANCED_FACE ( 'NONE', ( #4982 ), #43583, .F. ) ;
#31876 = ADVANCED_FACE ( 'NONE', ( #35107 ), #13230, .T. ) ;
#31877 = VECTOR ( 'NONE', #55352, 1000.000000000000227 ) ;
#31878 = DIRECTION ( 'NONE',  ( 0.9999697198139515519, 0.000000000000000000, 0.007781995580013368816 ) ) ;
#31879 = ORIENTED_EDGE ( 'NONE', *, *, #22664, .T. ) ;
#31880 = CARTESIAN_POINT ( 'NONE',  ( -14.38135624321859218, -1.651309408375658760, 2.414842859280319054 ) ) ;
#31881 = CARTESIAN_POINT ( 'NONE',  ( -20.10484237718952727, -0.1046793181814243412, 5.884109821959732756 ) ) ;
#31882 = LINE ( 'NONE', #6076, #19397 ) ;
#31883 = ORIENTED_EDGE ( 'NONE', *, *, #23618, .T. ) ;
#31884 = FACE_OUTER_BOUND ( 'NONE', #20831, .T. ) ;
#31885 = VERTEX_POINT ( 'NONE', #13764 ) ;
#31886 = EDGE_CURVE ( 'NONE', #48900, #35085, #22009, .T. ) ;
#31887 = ORIENTED_EDGE ( 'NONE', *, *, #44312, .F. ) ;
#31888 = EDGE_LOOP ( 'NONE', ( #43029, #29860, #55782, #11111 ) ) ;
#31889 = CARTESIAN_POINT ( 'NONE',  ( -13.77905473773374645, -1.489407457353156827, 2.186054020192172320 ) ) ;
#31890 = ORIENTED_EDGE ( 'NONE', *, *, #45354, .T. ) ;
#31891 = LINE ( 'NONE', #35596, #3944 ) ;
#31892 = PRODUCT ( 'Upper Lever Press Arm', 'Upper Lever Press Arm', '', ( #34319 ) ) ;
#31893 = ORIENTED_EDGE ( 'NONE', *, *, #34127, .F. ) ;
#31894 = DIRECTION ( 'NONE',  ( -0.5449076811759708816, 0.6444004775717707689, 0.5364919789714475140 ) ) ;
#31895 = CARTESIAN_POINT ( 'NONE',  ( -22.40634380310664397, 0.000000000000000000, 5.584705972946605534 ) ) ;
#31896 = VECTOR ( 'NONE', #17201, 999.9999999999998863 ) ;
#31897 = AXIS2_PLACEMENT_3D ( 'NONE', #46938, #28780, #15686 ) ;
#31898 = ORIENTED_EDGE ( 'NONE', *, *, #13665, .T. ) ;
#31899 = DIRECTION ( 'NONE',  ( 0.7660212471507180654, -0.6427876096865404731, 0.005961354470445141482 ) ) ;
#31900 = EDGE_LOOP ( 'NONE', ( #25024, #51146, #2483, #40510, #35931 ) ) ;
#31901 = DIRECTION ( 'NONE',  ( -0.005961354470445682716, -0.6427876096865404731, 0.7660212471507180654 ) ) ;
#31902 = LINE ( 'NONE', #13738, #22963 ) ;
#31903 = AXIS2_PLACEMENT_3D ( 'NONE', #11159, #24782, #29329 ) ;
#31904 = CARTESIAN_POINT ( 'NONE',  ( -12.33850799832341849, 0.000000000000000000, 11.68350162852954632 ) ) ;
#31905 = CARTESIAN_POINT ( 'NONE',  ( -1.246832498358330099E-15, 0.000000000000000000, 0.000000000000000000 ) ) ;
#31906 = DIRECTION ( 'NONE',  ( -0.5364919789714478471, 0.6444004775717705469, -0.5449076811759709926 ) ) ;
#31907 = FACE_OUTER_BOUND ( 'NONE', #36991, .T. ) ;
#31908 = CARTESIAN_POINT ( 'NONE',  ( -17.18674359190834977, 0.000000000000000000, 3.578659703450752350 ) ) ;
#31909 = ORIENTED_EDGE ( 'NONE', *, *, #4717, .T. ) ;
#31910 = VERTEX_POINT ( 'NONE', #48410 ) ;
#31911 = DIRECTION ( 'NONE',  ( 0.000000000000000000, -0.000000000000000000, -1.000000000000000000 ) ) ;
#31912 = ADVANCED_FACE ( 'NONE', ( #426 ), #9522, .F. ) ;
#31913 = LINE ( 'NONE', #39878, #2193 ) ;
#31914 = AXIS2_PLACEMENT_3D ( 'NONE', #39685, #26598, #4472 ) ;
#31915 = VECTOR ( 'NONE', #11452, 1000.000000000000227 ) ;
#31916 = PLANE ( 'NONE',  #54161 ) ;
#31917 = DIRECTION ( 'NONE',  ( 0.9321478471874540261, 0.000000000000000000, -0.3620778797217457101 ) ) ;
#31918 = EDGE_LOOP ( 'NONE', ( #51140, #3600, #15221, #24468 ) ) ;
#31919 = DIRECTION ( 'NONE',  ( 0.005002170337468016433, -0.7660444431189770143, -0.6427681459581293666 ) ) ;
#31920 = CARTESIAN_POINT ( 'NONE',  ( 2.072287782118878319, 0.000000000000000000, -2.950529333540147015 ) ) ;
#31921 = EDGE_LOOP ( 'NONE', ( #25952, #16545, #35501, #49498 ) ) ;
#31922 = FACE_OUTER_BOUND ( 'NONE', #51237, .T. ) ;
#31923 = DIRECTION ( 'NONE',  ( -0.5449076811759708816, 0.6444004775717707689, 0.5364919789714475140 ) ) ;
#31924 = ORIENTED_EDGE ( 'NONE', *, *, #14264, .F. ) ;
#31925 = EDGE_CURVE ( 'NONE', #54860, #12684, #1509, .T. ) ;
#31926 = CARTESIAN_POINT ( 'NONE',  ( -21.47419595591918906, 0.000000000000000000, 5.222628093224860102 ) ) ;
#31927 = DIRECTION ( 'NONE',  ( -0.7660212471507179544, -0.6427876096865405842, -0.005961354470445141482 ) ) ;
#31928 = DIRECTION ( 'NONE',  ( 0.005002170337468016433, -0.7660444431189770143, -0.6427681459581293666 ) ) ;
#31929 = EDGE_CURVE ( 'NONE', #5535, #19882, #51822, .T. ) ;
#31930 = EDGE_CURVE ( 'NONE', #33244, #4850, #8390, .T. ) ;
#31931 = CARTESIAN_POINT ( 'NONE',  ( -15.03495456790438389, -0.1191753592594197858, 12.77051346725278158 ) ) ;
#31932 = DIRECTION ( 'NONE',  ( 0.000000000000000000, 0.000000000000000000, -1.000000000000000000 ) ) ;
#31933 = EDGE_LOOP ( 'NONE', ( #36289, #54898, #13684, #35068 ) ) ;
#31934 = EDGE_LOOP ( 'NONE', ( #33131, #33626, #30898, #13709 ) ) ;
#31935 = PLANE ( 'NONE',  #24849 ) ;
#31936 = LINE ( 'NONE', #10368, #19511 ) ;
#31937 = CARTESIAN_POINT ( 'NONE',  ( -19.10230891376690110, -0.1191753592594169270, 8.465072266782243560 ) ) ;
#31938 = ADVANCED_FACE ( 'NONE', ( #21475 ), #15192, .F. ) ;
#31939 = AXIS2_PLACEMENT_3D ( 'NONE', #2401, #6962, #28514 ) ;
#31940 = AXIS2_PLACEMENT_3D ( 'NONE', #4537, #17900, #51941 ) ;
#31941 = DIRECTION ( 'NONE',  ( -0.6427681459581293666, -0.7660444431189770143, -0.005002170337467561935 ) ) ;
#31942 = EDGE_CURVE ( 'NONE', #2953, #25391, #1812, .T. ) ;
#31943 = CARTESIAN_POINT ( 'NONE',  ( -14.93495759592298988, 0.000000000000000000, 12.77129166681078409 ) ) ;
#31944 = ORIENTED_EDGE ( 'NONE', *, *, #29966, .F. ) ;
#31945 = CARTESIAN_POINT ( 'NONE',  ( 2.072287782118878319, 0.000000000000000000, -2.950529333540147015 ) ) ;
#31946 = PLANE ( 'NONE',  #2082 ) ;
#31947 = ADVANCED_FACE ( 'NONE', ( #23964 ), #10361, .F. ) ;
#31948 = LINE ( 'NONE', #49266, #22327 ) ;
#31949 = VECTOR ( 'NONE', #16101, 1000.000000000000114 ) ;
#31950 = PLANE ( 'NONE',  #52325 ) ;
#31951 = AXIS2_PLACEMENT_3D ( 'NONE', #23053, #44347, #35842 ) ;
#31952 = ORIENTED_EDGE ( 'NONE', *, *, #23920, .T. ) ;
#31953 = DIRECTION ( 'NONE',  ( 0.9999697198139515519, 0.000000000000000000, 0.007781995580013368816 ) ) ;
#31954 = ORIENTED_EDGE ( 'NONE', *, *, #14750, .F. ) ;
#31955 = DIRECTION ( 'NONE',  ( -0.005961354470445682716, -0.6427876096865404731, 0.7660212471507180654 ) ) ;
#31956 = PLANE ( 'NONE',  #47454 ) ;
#31957 = EDGE_CURVE ( 'NONE', #35444, #40739, #27685, .T. ) ;
#31958 = ORIENTED_EDGE ( 'NONE', *, *, #32768, .F. ) ;
#31959 = CARTESIAN_POINT ( 'NONE',  ( -10.66076323225010469, 0.000000000000000000, 0.9226289047854381309 ) ) ;
#31960 = STYLED_ITEM ( 'NONE', ( #37636 ), #2411 ) ;
#31961 = ORIENTED_EDGE ( 'NONE', *, *, #19560, .T. ) ;
#31962 = ADVANCED_FACE ( 'NONE', ( #18298 ), #1566, .F. ) ;
#31963 = VERTEX_POINT ( 'NONE', #27121 ) ;
#31964 = VERTEX_POINT ( 'NONE', #36463 ) ;
#31965 = CARTESIAN_POINT ( 'NONE',  ( -15.05648729026585819, 0.000000000000000000, 2.687247697364291366 ) ) ;
#31966 = ORIENTED_EDGE ( 'NONE', *, *, #15574, .F. ) ;
#31967 = ORIENTED_EDGE ( 'NONE', *, *, #7648, .F. ) ;
#31968 = DIRECTION ( 'NONE',  ( 0.007781995580012662783, 0.000000000000000000, -0.9999697198139514409 ) ) ;
#31969 = CARTESIAN_POINT ( 'NONE',  ( -1.086233639165236964, 0.000000000000000000, -2.796443541562362078 ) ) ;
#31970 = ORIENTED_EDGE ( 'NONE', *, *, #8100, .T. ) ;
#31971 = ORIENTED_EDGE ( 'NONE', *, *, #6384, .F. ) ;
#31972 = DIRECTION ( 'NONE',  ( 0.5364919789714477361, 0.6444004775717706579, 0.5449076811759711036 ) ) ;
#31973 = ORIENTED_EDGE ( 'NONE', *, *, #46894, .T. ) ;
#31974 = VECTOR ( 'NONE', #53782, 999.9999999999998863 ) ;
#31975 = ORIENTED_EDGE ( 'NONE', *, *, #12667, .F. ) ;
#31976 = CARTESIAN_POINT ( 'NONE',  ( -17.26532721389163072, 0.000000000000000000, 13.67648636611514590 ) ) ;
#31977 = PLANE ( 'NONE',  #7838 ) ;
#31978 = LINE ( 'NONE', #45880, #612 ) ;
#31979 = AXIS2_PLACEMENT_3D ( 'NONE', #36992, #27922, #45224 ) ;
#31980 = ORIENTED_EDGE ( 'NONE', *, *, #31640, .F. ) ;
#31981 = LINE ( 'NONE', #28553, #39201 ) ;
#31982 = ORIENTED_EDGE ( 'NONE', *, *, #49922, .F. ) ;
#31983 = VECTOR ( 'NONE', #32015, 1000.000000000000000 ) ;
#31984 = AXIS2_PLACEMENT_3D ( 'NONE', #22641, #39696, #14135 ) ;
#31985 = ADVANCED_FACE ( 'NONE', ( #44427 ), #14064, .F. ) ;
#31986 = PLANE ( 'NONE',  #32130 ) ;
#31987 = DIRECTION ( 'NONE',  ( -0.6427681459581293666, -0.7660444431189770143, -0.005002170337467561935 ) ) ;
#31988 = AXIS2_PLACEMENT_3D ( 'NONE', #27073, #44382, #5481 ) ;
#31989 = VECTOR ( 'NONE', #31154, 1000.000000000000227 ) ;
#31990 = CARTESIAN_POINT ( 'NONE',  ( -18.25990335970915268, -0.1191753592594171213, 9.210292201204588025 ) ) ;
#31991 = PLANE ( 'NONE',  #11425 ) ;
#31992 = DIRECTION ( 'NONE',  ( 0.9999697198139515519, 0.000000000000000000, 0.007781995580013368816 ) ) ;
#31993 = CARTESIAN_POINT ( 'NONE',  ( -11.20636620717317378, 0.000000000000000000, 11.32298014792380414 ) ) ;
#31994 = ORIENTED_EDGE ( 'NONE', *, *, #44141, .F. ) ;
#31995 = DIRECTION ( 'NONE',  ( 0.9999697198139515519, 0.000000000000000000, 0.007781995580013368816 ) ) ;
#31996 = ORIENTED_EDGE ( 'NONE', *, *, #1158, .T. ) ;
#31997 = FACE_OUTER_BOUND ( 'NONE', #22051, .T. ) ;
#31998 = CARTESIAN_POINT ( 'NONE',  ( -14.20280369269832832, 0.000000000000000000, 12.40765738797303719 ) ) ;
#31999 = DIRECTION ( 'NONE',  ( 0.000000000000000000, -0.000000000000000000, -1.000000000000000000 ) ) ;
#32000 = AXIS2_PLACEMENT_3D ( 'NONE', #27663, #6356, #44989 ) ;
#32001 = DIRECTION ( 'NONE',  ( 0.9999697198139515519, 0.000000000000000000, 0.007781995580013368816 ) ) ;
#32002 = VECTOR ( 'NONE', #29935, 1000.000000000000227 ) ;
#32003 = ADVANCED_FACE ( 'NONE', ( #45278 ), #40169, .F. ) ;
#32004 = CARTESIAN_POINT ( 'NONE',  ( -11.61397488332059602, 0.000000000000000000, 3.991360347924631125 ) ) ;
#32005 = CARTESIAN_POINT ( 'NONE',  ( -67.98273966911209243, -0.9999999999999983347, -3.909888324369924284 ) ) ;
#32006 = ORIENTED_EDGE ( 'NONE', *, *, #55504, .T. ) ;
#32007 = CARTESIAN_POINT ( 'NONE',  ( -33.75052341732683914, 11.44035125802762032, 4.909800093382857611 ) ) ;
#32008 = CARTESIAN_POINT ( 'NONE',  ( -15.74363206212979094, -3.270328918600661439, 2.892341851553068999 ) ) ;
#32009 = CARTESIAN_POINT ( 'NONE',  ( -14.01701317841955508, 0.000000000000000000, 2.326005055450897085 ) ) ;
#32010 = VECTOR ( 'NONE', #50689, 1000.000000000000227 ) ;
#32011 = CARTESIAN_POINT ( 'NONE',  ( -70.00279782826048347, 0.1332992376639058896, -7.501782499249456393 ) ) ;
#32012 = ADVANCED_FACE ( 'NONE', ( #41299 ), #14897, .F. ) ;
#32013 = DIRECTION ( 'NONE',  ( -0.6427681459581293666, -0.7660444431189770143, -0.005002170337467561935 ) ) ;
#32014 = VECTOR ( 'NONE', #4559, 1000.000000000000000 ) ;
#32015 = DIRECTION ( 'NONE',  ( -0.9321478471874541372, -0.000000000000000000, 0.3620778797217454326 ) ) ;
#32016 = EDGE_CURVE ( 'NONE', #56039, #3193, #45014, .T. ) ;
#32017 = DIRECTION ( 'NONE',  ( 0.5364919789714477361, 0.6444004775717706579, 0.5449076811759711036 ) ) ;
#32018 = VECTOR ( 'NONE', #45996, 999.9999999999998863 ) ;
#32019 = LINE ( 'NONE', #49341, #46432 ) ;
#32020 = VECTOR ( 'NONE', #44440, 999.9999999999998863 ) ;
#32021 = ADVANCED_FACE ( 'NONE', ( #2088 ), #28221, .F. ) ;
#32022 = VECTOR ( 'NONE', #21859, 999.9999999999998863 ) ;
#32023 = ORIENTED_EDGE ( 'NONE', *, *, #23206, .F. ) ;
#32024 = EDGE_CURVE ( 'NONE', #13096, #12755, #48713, .T. ) ;
#32025 = VECTOR ( 'NONE', #53725, 999.9999999999998863 ) ;
#32026 = ORIENTED_EDGE ( 'NONE', *, *, #56114, .T. ) ;
#32027 = ORIENTED_EDGE ( 'NONE', *, *, #18757, .F. ) ;
#32028 = AXIS2_PLACEMENT_3D ( 'NONE', #13440, #17972, #652 ) ;
#32029 = EDGE_LOOP ( 'NONE', ( #55016, #37205, #33570, #39938 ) ) ;
#32030 = ORIENTED_EDGE ( 'NONE', *, *, #49518, .T. ) ;
#32031 = FACE_OUTER_BOUND ( 'NONE', #48163, .T. ) ;
#32032 = DIRECTION ( 'NONE',  ( 0.000000000000000000, -0.000000000000000000, -1.000000000000000000 ) ) ;
#32033 = ORIENTED_EDGE ( 'NONE', *, *, #28198, .T. ) ;
#32034 = ORIENTED_EDGE ( 'NONE', *, *, #24819, .F. ) ;
#32035 = VECTOR ( 'NONE', #48223, 1000.000000000000227 ) ;
#32036 = ORIENTED_EDGE ( 'NONE', *, *, #22498, .F. ) ;
#32037 = VECTOR ( 'NONE', #43072, 1000.000000000000227 ) ;
#32038 = DIRECTION ( 'NONE',  ( 0.7660212471507180654, -0.6427876096865404731, 0.005961354470445141482 ) ) ;
#32039 = DIRECTION ( 'NONE',  ( 0.007781995580012662783, 0.000000000000000000, -0.9999697198139514409 ) ) ;
#32040 = LINE ( 'NONE', #9916, #45837 ) ;
#32041 = ORIENTED_EDGE ( 'NONE', *, *, #27857, .F. ) ;
#32042 = CARTESIAN_POINT ( 'NONE',  ( -17.26532721389163072, 0.000000000000000000, 13.67648636611514590 ) ) ;
#32043 = EDGE_CURVE ( 'NONE', #35922, #55515, #32226, .T. ) ;
#32044 = VECTOR ( 'NONE', #5253, 1000.000000000000227 ) ;
#32045 = ORIENTED_EDGE ( 'NONE', *, *, #12667, .T. ) ;
#32046 = DIRECTION ( 'NONE',  ( 0.7660212471507180654, -0.6427876096865404731, 0.005961354470445141482 ) ) ;
#32047 = EDGE_CURVE ( 'NONE', #41786, #428, #27970, .T. ) ;
#32049 = VECTOR ( 'NONE', #23079, 1000.000000000000227 ) ;
#32048 = CARTESIAN_POINT ( 'NONE',  ( 2.072287782118878319, 0.000000000000000000, -2.950529333540147015 ) ) ;
#32050 = CARTESIAN_POINT ( 'NONE',  ( -12.87254409838392810, 2.391131607591507002, 1.605775395510381287 ) ) ;
#32051 = LINE ( 'NONE', #9341, #47806 ) ;
#32052 = EDGE_CURVE ( 'NONE', #42377, #41065, #23429, .T. ) ;
#32053 = PLANE ( 'NONE',  #55805 ) ;
#32054 = LINE ( 'NONE', #15841, #18406 ) ;
#32055 = DIRECTION ( 'NONE',  ( -0.7660212471507179544, -0.6427876096865405842, -0.005961354470445141482 ) ) ;
#32056 = EDGE_CURVE ( 'NONE', #36173, #41663, #6651, .T. ) ;
#32057 = AXIS2_PLACEMENT_3D ( 'NONE', #27076, #4932, #44116 ) ;
#32058 = ORIENTED_EDGE ( 'NONE', *, *, #54155, .T. ) ;
#32059 = DIRECTION ( 'NONE',  ( 0.000000000000000000, -1.000000000000000000, 0.000000000000000000 ) ) ;
#32060 = ORIENTED_EDGE ( 'NONE', *, *, #30324, .T. ) ;
#32061 = ADVANCED_FACE ( 'NONE', ( #40745 ), #14357, .F. ) ;
#32062 = EDGE_CURVE ( 'NONE', #15806, #28385, #24512, .T. ) ;
#32063 = ADVANCED_FACE ( 'NONE', ( #55188 ), #7478, .F. ) ;
#32064 = AXIS2_PLACEMENT_3D ( 'NONE', #5444, #9726, #44069 ) ;
#32065 = VECTOR ( 'NONE', #34876, 1000.000000000000227 ) ;
#32066 = DIRECTION ( 'NONE',  ( 0.5449076811759707706, 0.6444004775717708799, -0.5364919789714476250 ) ) ;
#32067 = PLANE ( 'NONE',  #19611 ) ;
#32068 = DIRECTION ( 'NONE',  ( 0.5449076811759707706, 0.6444004775717708799, -0.5364919789714476250 ) ) ;
#32069 = CARTESIAN_POINT ( 'NONE',  ( -17.88873712828089424, 0.000000000000000000, 8.374513534917676694 ) ) ;
#32070 = CARTESIAN_POINT ( 'NONE',  ( -16.51274120858988681, -5.213152330870661544, 11.65171230228703969 ) ) ;
#32071 = LINE ( 'NONE', #36074, #17672 ) ;
#32072 = CARTESIAN_POINT ( 'NONE',  ( -15.60102546347950536, 0.000000000000000000, 12.95077420755565356 ) ) ;
#32073 = VECTOR ( 'NONE', #11424, 999.9999999999998863 ) ;
#32074 = FACE_OUTER_BOUND ( 'NONE', #42537, .T. ) ;
#32075 = AXIS2_PLACEMENT_3D ( 'NONE', #45906, #28293, #7023 ) ;
#32076 = SURFACE_SIDE_STYLE ('',( #1106 ) ) ;
#32077 = LINE ( 'NONE', #11032, #4771 ) ;
#32078 = EDGE_LOOP ( 'NONE', ( #43332, #321, #33639, #31752 ) ) ;
#32079 = FACE_OUTER_BOUND ( 'NONE', #52546, .T. ) ;
#32080 = CARTESIAN_POINT ( 'NONE',  ( -14.63931068118123591, -4.727446477803164626, 2.416896245294180012 ) ) ;
#32081 = PLANE ( 'NONE',  #13711 ) ;
#32082 = LINE ( 'NONE', #49106, #24029 ) ;
#32083 = CARTESIAN_POINT ( 'NONE',  ( -16.70141711715487887, 4.172053068839010947, 3.036218986314767943 ) ) ;
#32084 = EDGE_CURVE ( 'NONE', #46919, #53826, #37586, .T. ) ;
#32085 = CARTESIAN_POINT ( 'NONE',  ( -19.79569077582305070, 0.000000000000000000, 14.58012466630350445 ) ) ;
#32086 = LINE ( 'NONE', #53115, #32373 ) ;
#32087 = CARTESIAN_POINT ( 'NONE',  ( 1.710209902397132220, -1.000000000000000000, -3.882677180727601041 ) ) ;
#32088 = VERTEX_POINT ( 'NONE', #33346 ) ;
#32089 = ADVANCED_FACE ( 'NONE', ( #20820 ), #38138, .F. ) ;
#32090 = ORIENTED_EDGE ( 'NONE', *, *, #21748, .F. ) ;
#32091 = AXIS2_PLACEMENT_3D ( 'NONE', #14577, #1219, #45239 ) ;
#32092 = ADVANCED_FACE ( 'NONE', ( #45824 ), #11746, .F. ) ;
#32093 = CARTESIAN_POINT ( 'NONE',  ( -14.86643316120819591, 0.000000000000000000, 3.966048965548564453 ) ) ;
#32094 = CARTESIAN_POINT ( 'NONE',  ( -10.22868635331318643, 0.000000000000000000, 5.110137193001952127 ) ) ;
#32095 = AXIS2_PLACEMENT_3D ( 'NONE', #4475, #47066, #38841 ) ;
#32096 = ADVANCED_FACE ( 'NONE', ( #41828 ), #24262, .F. ) ;
#32097 = EDGE_LOOP ( 'NONE', ( #5578, #40852, #18022, #55108 ) ) ;
#32098 = DIRECTION ( 'NONE',  ( -0.6427681459581293666, -0.7660444431189770143, -0.005002170337467561935 ) ) ;
#32099 = VECTOR ( 'NONE', #40233, 999.9999999999998863 ) ;
#32100 = ORIENTED_EDGE ( 'NONE', *, *, #42452, .F. ) ;
#32101 = CARTESIAN_POINT ( 'NONE',  ( -12.99794575893872839, 0.000000000000000000, 2.703267743552332014 ) ) ;
#32102 = EDGE_LOOP ( 'NONE', ( #8055, #45545, #47044, #40313 ) ) ;
#32103 = ORIENTED_EDGE ( 'NONE', *, *, #43314, .T. ) ;
#32104 = ORIENTED_EDGE ( 'NONE', *, *, #40505, .F. ) ;
#32105 = DIRECTION ( 'NONE',  ( 0.9999697198139515519, 0.000000000000000000, 0.007781995580013368816 ) ) ;
#32106 = AXIS2_PLACEMENT_3D ( 'NONE', #7724, #38374, #51457 ) ;
#32107 = LINE ( 'NONE', #15335, #31396 ) ;
#32108 = DIRECTION ( 'NONE',  ( -0.5364919789714478471, 0.6444004775717705469, -0.5449076811759709926 ) ) ;
#32109 = VECTOR ( 'NONE', #49973, 999.9999999999998863 ) ;
#32110 = ORIENTED_EDGE ( 'NONE', *, *, #54553, .T. ) ;
#32111 = EDGE_LOOP ( 'NONE', ( #7730, #6693, #40339, #27549 ) ) ;
#32112 = AXIS2_PLACEMENT_3D ( 'NONE', #21554, #21809, #30055 ) ;
#32113 = VECTOR ( 'NONE', #15720, 999.9999999999998863 ) ;
#32114 = FACE_OUTER_BOUND ( 'NONE', #22721, .T. ) ;
#32115 = ORIENTED_EDGE ( 'NONE', *, *, #3653, .F. ) ;
#32116 = PLANE ( 'NONE',  #23004 ) ;
#32117 = VERTEX_POINT ( 'NONE', #29061 ) ;
#32118 = CARTESIAN_POINT ( 'NONE',  ( -10.30934315031560544, -0.1191753592594188005, 2.624188042620991368 ) ) ;
#32119 = LINE ( 'NONE', #40902, #53001 ) ;
#32120 = ORIENTED_EDGE ( 'NONE', *, *, #31925, .T. ) ;
#32121 = DIRECTION ( 'NONE',  ( 0.007781995580012663651, 0.000000000000000000, -0.9999697198139515519 ) ) ;
#32122 = VECTOR ( 'NONE', #45183, 999.9999999999998863 ) ;
#32123 = LINE ( 'NONE', #1462, #37249 ) ;
#32124 = AXIS2_PLACEMENT_3D ( 'NONE', #42441, #21429, #43298 ) ;
#32125 = ORIENTED_EDGE ( 'NONE', *, *, #11093, .T. ) ;
#32126 = FACE_OUTER_BOUND ( 'NONE', #37221, .T. ) ;
#32127 = DIRECTION ( 'NONE',  ( 0.9999697198139515519, 0.000000000000000000, 0.007781995580013368816 ) ) ;
#32128 = LINE ( 'NONE', #49451, #29209 ) ;
#32129 = ORIENTED_EDGE ( 'NONE', *, *, #23846, .T. ) ;
#32130 = AXIS2_PLACEMENT_3D ( 'NONE', #27747, #19189, #27438 ) ;
#32131 = EDGE_CURVE ( 'NONE', #36758, #3085, #41570, .T. ) ;
#32132 = EDGE_CURVE ( 'NONE', #23151, #53142, #2652, .T. ) ;
#32133 = LINE ( 'NONE', #1169, #29217 ) ;
#32134 = CARTESIAN_POINT ( 'NONE',  ( -17.74560456716937296, 0.000000000000000000, 3.774316574337878372 ) ) ;
#32135 = DIRECTION ( 'NONE',  ( -0.005002170337468016433, -0.7660444431189770143, 0.6427681459581293666 ) ) ;
#32136 = VECTOR ( 'NONE', #18716, 999.9999999999998863 ) ;
#32137 = DIRECTION ( 'NONE',  ( -0.3313982828793700097, 0.4028455766673915694, -0.8531650599175529814 ) ) ;
#32138 = EDGE_CURVE ( 'NONE', #33548, #41210, #28805, .T. ) ;
#32139 = FACE_OUTER_BOUND ( 'NONE', #25347, .T. ) ;
#32140 = CARTESIAN_POINT ( 'NONE',  ( -56.70083583094844926, 4.876814673940706335, 2.999999999999993339 ) ) ;
#32141 = CARTESIAN_POINT ( 'NONE',  ( -66.44890184452549420, -11.32768097537891272, 0.7018102913113006824 ) ) ;
#32142 = ORIENTED_EDGE ( 'NONE', *, *, #38249, .T. ) ;
#32143 = CARTESIAN_POINT ( 'NONE',  ( -15.75281958048178232, 1.905425754524005200, 6.127379490061689360 ) ) ;
#32144 = DIRECTION ( 'NONE',  ( 0.005002170337468016433, -0.7660444431189770143, -0.6427681459581293666 ) ) ;
#32145 = CARTESIAN_POINT ( 'NONE',  ( -66.91114292034374955, -1.627825983345676869E-11, 3.533109812942180739 ) ) ;
#32146 = ORIENTED_EDGE ( 'NONE', *, *, #44909, .T. ) ;
#32147 = AXIS2_PLACEMENT_3D ( 'NONE', #44516, #41402, #28314 ) ;
#32148 = CARTESIAN_POINT ( 'NONE',  ( -16.53317331066696383, 0.000000000000000000, 13.31285208727739899 ) ) ;
#32149 = LINE ( 'NONE', #54002, #51727 ) ;
#32150 = VECTOR ( 'NONE', #33332, 1000.000000000000227 ) ;
#32151 = CARTESIAN_POINT ( 'NONE',  ( -19.60990026154428278, 0.000000000000000000, 4.498472333781370125 ) ) ;
#32152 = DIRECTION ( 'NONE',  ( -0.5449076811759708816, 0.6444004775717707689, 0.5364919789714475140 ) ) ;
#32153 = ADVANCED_FACE ( 'NONE', ( #16555 ), #46960, .F. ) ;
#32154 = PLANE ( 'NONE',  #43792 ) ;
#32155 = ORIENTED_EDGE ( 'NONE', *, *, #26168, .F. ) ;
#32156 = VECTOR ( 'NONE', #14432, 999.9999999999998863 ) ;
#32157 = AXIS2_PLACEMENT_3D ( 'NONE', #3083, #51063, #20706 ) ;
#32158 = VERTEX_POINT ( 'NONE', #7785 ) ;
#32159 = ADVANCED_FACE ( 'NONE', ( #12322 ), #2919, .F. ) ;
#32160 = DIRECTION ( 'NONE',  ( -0.005961354470445682716, -0.6427876096865404731, 0.7660212471507180654 ) ) ;
#32161 = LINE ( 'NONE', #35873, #17840 ) ;
#32162 = DIRECTION ( 'NONE',  ( -0.9999697198139514409, -0.000000000000000000, -0.007781995580013368816 ) ) ;
#32163 = ADVANCED_FACE ( 'NONE', ( #29661 ), #25372, .F. ) ;
#32164 = ORIENTED_EDGE ( 'NONE', *, *, #10539, .T. ) ;
#32165 = FACE_OUTER_BOUND ( 'NONE', #42880, .T. ) ;
#32166 = EDGE_LOOP ( 'NONE', ( #41339, #45995, #23398, #34047 ) ) ;
#32167 = FACE_OUTER_BOUND ( 'NONE', #44320, .T. ) ;
#32168 = VECTOR ( 'NONE', #38863, 1000.000000000000227 ) ;
#32169 = ORIENTED_EDGE ( 'NONE', *, *, #4522, .T. ) ;
#32170 = VECTOR ( 'NONE', #28396, 999.9999999999998863 ) ;
#32171 = CARTESIAN_POINT ( 'NONE',  ( -16.81345671998191449, 0.000000000000000000, 3.412238694616132495 ) ) ;
#32172 = CARTESIAN_POINT ( 'NONE',  ( -24.96676581047183063, 18.24370688441070953, -4.657437592157546824 ) ) ;
#32173 = EDGE_CURVE ( 'NONE', #55867, #49289, #3227, .T. ) ;
#32174 = VECTOR ( 'NONE', #47721, 1000.000000000000114 ) ;
#32175 = FACE_OUTER_BOUND ( 'NONE', #158, .T. ) ;
#32176 = EDGE_LOOP ( 'NONE', ( #35110, #19169, #22413, #50955, #2409 ) ) ;
#32177 = CARTESIAN_POINT ( 'NONE',  ( -19.98224170412465028, 0.000000000000000000, 4.543407702002897786 ) ) ;
#32178 = VECTOR ( 'NONE', #4533, 1000.000000000000227 ) ;
#32179 = ORIENTED_EDGE ( 'NONE', *, *, #6827, .F. ) ;
#32180 = ORIENTED_EDGE ( 'NONE', *, *, #40608, .F. ) ;
#32181 = ORIENTED_EDGE ( 'NONE', *, *, #19403, .T. ) ;
#32182 = DIRECTION ( 'NONE',  ( -0.005961354470445682716, -0.6427876096865404731, 0.7660212471507180654 ) ) ;
#32183 = VECTOR ( 'NONE', #27108, 1000.000000000000000 ) ;
#32184 = ORIENTED_EDGE ( 'NONE', *, *, #23733, .T. ) ;
#32185 = VECTOR ( 'NONE', #40513, 1000.000000000000000 ) ;
#32186 = FACE_OUTER_BOUND ( 'NONE', #30535, .T. ) ;
#32187 = ORIENTED_EDGE ( 'NONE', *, *, #15200, .F. ) ;
#32188 = DIRECTION ( 'NONE',  ( 0.7660212471507180654, -0.6427876096865404731, 0.005961354470445141482 ) ) ;
#32189 = DIRECTION ( 'NONE',  ( 0.9999697198139515519, 0.000000000000000000, 0.007781995580013368816 ) ) ;
#32190 = AXIS2_PLACEMENT_3D ( 'NONE', #24434, #42031, #6860 ) ;
#32191 = VERTEX_POINT ( 'NONE', #29349 ) ;
#32192 = CARTESIAN_POINT ( 'NONE',  ( -18.36487023914310512, 0.000000000000000000, 9.848136436180725539 ) ) ;
#32193 = ORIENTED_EDGE ( 'NONE', *, *, #18421, .F. ) ;
#32194 = VECTOR ( 'NONE', #45544, 999.9999999999998863 ) ;
#32195 = PLANE ( 'NONE',  #23762 ) ;
#32196 = VECTOR ( 'NONE', #7538, 1000.000000000000000 ) ;
#32197 = CARTESIAN_POINT ( 'NONE',  ( -12.55187083751861721, 0.000000000000000000, 5.092057634161903934 ) ) ;
#32198 = FACE_OUTER_BOUND ( 'NONE', #27989, .T. ) ;
#32199 = CARTESIAN_POINT ( 'NONE',  ( -12.10922913985712412, 0.000000000000000000, 7.922009404736876981 ) ) ;
#32200 = LINE ( 'NONE', #19954, #32363 ) ;
#32201 = CARTESIAN_POINT ( 'NONE',  ( 2.072287782118878319, 0.000000000000000000, -2.950529333540147015 ) ) ;
#32202 = LINE ( 'NONE', #31650, #8399 ) ;
#32203 = ORIENTED_EDGE ( 'NONE', *, *, #24520, .F. ) ;
#32204 = ADVANCED_FACE ( 'NONE', ( #54344 ), #15435, .F. ) ;
#32205 = VERTEX_POINT ( 'NONE', #33050 ) ;
#32206 = CARTESIAN_POINT ( 'NONE',  ( -14.94916102560700821, 0.000000000000000000, 2.688082935172642962 ) ) ;
#32207 = DIRECTION ( 'NONE',  ( 0.007781995580012663651, 0.000000000000000000, -0.9999697198139515519 ) ) ;
#32208 = EDGE_CURVE ( 'NONE', #33959, #34435, #39265, .T. ) ;
#32209 = ADVANCED_FACE ( 'NONE', ( #34723 ), #8619, .F. ) ;
#32210 = DIRECTION ( 'NONE',  ( -0.9999697198139514409, -0.000000000000000000, -0.007781995580013368816 ) ) ;
#32211 = AXIS2_PLACEMENT_3D ( 'NONE', #9533, #43046, #980 ) ;
#32212 = CARTESIAN_POINT ( 'NONE',  ( -24.56000334535257679, 18.39573966706334929, 4.548402587786432250 ) ) ;
#32213 = ORIENTED_EDGE ( 'NONE', *, *, #53096, .F. ) ;
#32214 = VECTOR ( 'NONE', #19464, 999.9999999999998863 ) ;
#32215 = DIRECTION ( 'NONE',  ( -0.005961354470445682716, -0.6427876096865404731, 0.7660212471507180654 ) ) ;
#32216 = CARTESIAN_POINT ( 'NONE',  ( 2.072287782118878319, 0.000000000000000000, -2.950529333540147015 ) ) ;
#32217 = ORIENTED_EDGE ( 'NONE', *, *, #56147, .T. ) ;
#32218 = FACE_OUTER_BOUND ( 'NONE', #5988, .T. ) ;
#32219 = LINE ( 'NONE', #23139, #28554 ) ;
#32220 = VECTOR ( 'NONE', #43331, 999.9999999999998863 ) ;
#32221 = ORIENTED_EDGE ( 'NONE', *, *, #49474, .T. ) ;
#32222 = CARTESIAN_POINT ( 'NONE',  ( -68.44026216309750055, -1.000000000000000000, 5.059064008999124340 ) ) ;
#32223 = FACE_OUTER_BOUND ( 'NONE', #46455, .T. ) ;
#32224 = VECTOR ( 'NONE', #25226, 1000.000000000000114 ) ;
#32225 = FACE_OUTER_BOUND ( 'NONE', #18896, .T. ) ;
#32226 = LINE ( 'NONE', #53264, #37755 ) ;
#32227 = ADVANCED_FACE ( 'NONE', ( #13155 ), #43793, .F. ) ;
#32228 = DIRECTION ( 'NONE',  ( -0.3620778797217457101, 0.000000000000000000, -0.9321478471874540261 ) ) ;
#32229 = ORIENTED_EDGE ( 'NONE', *, *, #41123, .F. ) ;
#32230 = VECTOR ( 'NONE', #6091, 1000.000000000000000 ) ;
#32231 = VECTOR ( 'NONE', #5243, 1000.000000000000227 ) ;
#32232 = ORIENTED_EDGE ( 'NONE', *, *, #7859, .T. ) ;
#32233 = VECTOR ( 'NONE', #10284, 1000.000000000000000 ) ;
#32234 = LINE ( 'NONE', #33057, #3066 ) ;
#32235 = PLANE ( 'NONE',  #34975 ) ;
#32236 = DIRECTION ( 'NONE',  ( 0.005002170337468016433, -0.7660444431189770143, -0.6427681459581293666 ) ) ;
#32237 = AXIS2_PLACEMENT_3D ( 'NONE', #13305, #30631, #9030 ) ;
#32239 = CARTESIAN_POINT ( 'NONE',  ( 6.001673287911728494, 0.0004827855869357527193, -0.7726386493456292026 ) ) ;
#32238 = VECTOR ( 'NONE', #35142, 1000.000000000000000 ) ;
#32240 = DIRECTION ( 'NONE',  ( -0.5364919789714478471, 0.6444004775717705469, -0.5449076811759709926 ) ) ;
#32241 = VERTEX_POINT ( 'NONE', #47507 ) ;
#32242 = DIRECTION ( 'NONE',  ( -0.05705673239519650636, 0.9983709377222390602, 2.351258244848514932E-16 ) ) ;
#32243 = ADVANCED_FACE ( 'NONE', ( #30763 ), #9160, .F. ) ;
#32244 = AXIS2_PLACEMENT_3D ( 'NONE', #29278, #51447, #42620 ) ;
#32245 = CARTESIAN_POINT ( 'NONE',  ( -56.66762604419704985, 5.055998648713356580, 2.999999999999993339 ) ) ;
#32246 = VECTOR ( 'NONE', #33528, 1000.000000000000227 ) ;
#32247 = LINE ( 'NONE', #23694, #55933 ) ;
#32248 = ORIENTED_EDGE ( 'NONE', *, *, #49388, .F. ) ;
#32249 = EDGE_CURVE ( 'NONE', #19711, #40042, #4910, .T. ) ;
#32250 = PLANE ( 'NONE',  #17512 ) ;
#32251 = ORIENTED_EDGE ( 'NONE', *, *, #29648, .F. ) ;
#32252 = DIRECTION ( 'NONE',  ( -0.5364919789714478471, 0.6444004775717705469, -0.5449076811759709926 ) ) ;
#32253 = CARTESIAN_POINT ( 'NONE',  ( -14.61484282146703251, 0.000000000000000000, 5.645341235194416107 ) ) ;
#32254 = EDGE_LOOP ( 'NONE', ( #36234, #8860, #13675, #9471 ) ) ;
#32255 = DIRECTION ( 'NONE',  ( 0.005002170337468016433, -0.7660444431189770143, -0.6427681459581293666 ) ) ;
#32256 = EDGE_CURVE ( 'NONE', #5924, #29543, #658, .T. ) ;
#32257 = ORIENTED_EDGE ( 'NONE', *, *, #18491, .F. ) ;
#32258 = AXIS2_PLACEMENT_3D ( 'NONE', #30194, #4918, #12604 ) ;
#32259 = EDGE_LOOP ( 'NONE', ( #42190, #23465, #39857, #33175, #55131, #53175, #45353, #49803 ) ) ;
#32260 = ORIENTED_EDGE ( 'NONE', *, *, #48746, .F. ) ;
#32261 = CARTESIAN_POINT ( 'NONE',  ( -29.08986725154028363, 15.86323315751366358, 4.728329674295676632 ) ) ;
#32262 = EDGE_LOOP ( 'NONE', ( #7943, #50868, #12826, #38648 ) ) ;
#32263 = AXIS2_PLACEMENT_3D ( 'NONE', #45869, #54956, #28841 ) ;
#32264 = ORIENTED_EDGE ( 'NONE', *, *, #26646, .T. ) ;
#32265 = FACE_OUTER_BOUND ( 'NONE', #35495, .T. ) ;
#32266 = AXIS2_PLACEMENT_3D ( 'NONE', #25945, #42668, #38987 ) ;
#32267 = ORIENTED_EDGE ( 'NONE', *, *, #43242, .T. ) ;
#32268 = VERTEX_POINT ( 'NONE', #21095 ) ;
#32269 = FACE_OUTER_BOUND ( 'NONE', #10406, .T. ) ;
#32270 = ORIENTED_EDGE ( 'NONE', *, *, #47652, .F. ) ;
#32271 = AXIS2_PLACEMENT_3D ( 'NONE', #42030, #3130, #15360 ) ;
#32272 = ORIENTED_EDGE ( 'NONE', *, *, #46888, .T. ) ;
#32273 = ADVANCED_FACE ( 'NONE', ( #52346 ), #17980, .F. ) ;
#32274 = CIRCLE ( 'NONE', #42225, 0.5000000000000004441 ) ;
#32275 = AXIS2_PLACEMENT_3D ( 'NONE', #25392, #30517, #25134 ) ;
#32276 = DIRECTION ( 'NONE',  ( 0.9999697198139515519, 0.000000000000000000, 0.007781995580013368816 ) ) ;
#32277 = CARTESIAN_POINT ( 'NONE',  ( -15.42897117608339741, -0.1191753592594185229, 3.692342122946178584 ) ) ;
#32278 = DIRECTION ( 'NONE',  ( 0.9999697198139515519, 0.000000000000000000, 0.007781995580013368816 ) ) ;
#32279 = DIRECTION ( 'NONE',  ( 0.005961354470445682716, -0.6427876096865404731, -0.7660212471507180654 ) ) ;
#32280 = EDGE_CURVE ( 'NONE', #10313, #36287, #52040, .T. ) ;
#32281 = ORIENTED_EDGE ( 'NONE', *, *, #21580, .T. ) ;
#32282 = DIRECTION ( 'NONE',  ( -0.7660212471507179544, -0.6427876096865405842, -0.005961354470445141482 ) ) ;
#32283 = EDGE_LOOP ( 'NONE', ( #36317, #16313, #15375, #47643 ) ) ;
#32284 = VECTOR ( 'NONE', #20819, 999.9999999999998863 ) ;
#32285 = VECTOR ( 'NONE', #13808, 999.9999999999998863 ) ;
#32286 = EDGE_CURVE ( 'NONE', #33398, #8024, #13698, .T. ) ;
#32287 = AXIS2_PLACEMENT_3D ( 'NONE', #45541, #43949, #1054 ) ;
#32288 = CARTESIAN_POINT ( 'NONE',  ( -17.46532115785441519, 0.000000000000000000, 13.67492996699914265 ) ) ;
#32289 = EDGE_CURVE ( 'NONE', #21088, #40269, #12598, .T. ) ;
#32290 = AXIS2_PLACEMENT_3D ( 'NONE', #35318, #9182, #52616 ) ;
#32291 = CARTESIAN_POINT ( 'NONE',  ( -13.08330893211609869, 0.000000000000000000, 1.763933231766363630 ) ) ;
#32292 = VECTOR ( 'NONE', #6722, 1000.000000000000227 ) ;
#32293 = DIRECTION ( 'NONE',  ( -0.005961354470445682716, -0.6427876096865404731, 0.7660212471507180654 ) ) ;
#32294 = LINE ( 'NONE', #49861, #6720 ) ;
#32295 = DIRECTION ( 'NONE',  ( -0.6427681459581293666, -0.7660444431189770143, -0.005002170337467561935 ) ) ;
#32296 = VERTEX_POINT ( 'NONE', #21680 ) ;
#32297 = DIRECTION ( 'NONE',  ( 0.9999697198139515519, 0.000000000000000000, 0.007781995580013368816 ) ) ;
#32298 = ORIENTED_EDGE ( 'NONE', *, *, #24328, .T. ) ;
#32299 = EDGE_CURVE ( 'NONE', #24601, #47628, #31011, .T. ) ;
#32300 = LINE ( 'NONE', #54673, #40127 ) ;
#32301 = LINE ( 'NONE', #53325, #13308 ) ;
#32302 = CARTESIAN_POINT ( 'NONE',  ( -26.13337879274045505, 0.000000000000000000, 6.833023547870798353 ) ) ;
#32303 = CARTESIAN_POINT ( 'NONE',  ( -21.47341775636118655, -0.1191753592594197858, 5.122631121243466090 ) ) ;
#32304 = CARTESIAN_POINT ( 'NONE',  ( -10.86457665906423919, 0.000000000000000000, 1.411867849540296094 ) ) ;
#32305 = AXIS2_PLACEMENT_3D ( 'NONE', #48989, #10088, #23163 ) ;
#32306 = EDGE_CURVE ( 'NONE', #37808, #636, #43521, .T. ) ;
#32307 = ORIENTED_EDGE ( 'NONE', *, *, #38449, .T. ) ;
#32308 = CARTESIAN_POINT ( 'NONE',  ( -11.91475904335884017, -1.489407457353156827, 1.461898260748682787 ) ) ;
#32309 = DIRECTION ( 'NONE',  ( -0.5449076811759708816, 0.6444004775717707689, 0.5364919789714475140 ) ) ;
#32310 = CARTESIAN_POINT ( 'NONE',  ( -12.33850799832341849, 0.000000000000000000, 11.68350162852954632 ) ) ;
#32311 = AXIS2_PLACEMENT_3D ( 'NONE', #32501, #14887, #23670 ) ;
#32312 = FACE_OUTER_BOUND ( 'NONE', #31934, .T. ) ;
#32313 = VECTOR ( 'NONE', #11025, 1000.000000000000227 ) ;
#32314 = CARTESIAN_POINT ( 'NONE',  ( -11.20636620717317378, 0.000000000000000000, 11.32298014792380414 ) ) ;
#32315 = CARTESIAN_POINT ( 'NONE',  ( -10.31221720382088947, -0.1191753592594183703, 2.993497745878755278 ) ) ;
#32316 = LINE ( 'NONE', #49632, #2931 ) ;
#32317 = VECTOR ( 'NONE', #23541, 1000.000000000000114 ) ;
#32318 = VECTOR ( 'NONE', #26251, 999.9999999999998863 ) ;
#32319 = CARTESIAN_POINT ( 'NONE',  ( -17.67981966024466800, -0.03228989815065527041, 3.747733265616297160 ) ) ;
#32320 = CARTESIAN_POINT ( 'NONE',  ( -21.45016440283565373, -5.536956232915663634, 14.10099251443048729 ) ) ;
#32321 = ORIENTED_EDGE ( 'NONE', *, *, #40844, .F. ) ;
#32322 = AXIS2_PLACEMENT_3D ( 'NONE', #16021, #33345, #35490 ) ;
#32323 = VERTEX_POINT ( 'NONE', #34193 ) ;
#32324 = AXIS2_PLACEMENT_3D ( 'NONE', #403, #27360, #18019 ) ;
#32325 = EDGE_CURVE ( 'NONE', #54313, #17993, #30493, .T. ) ;
#32326 = VECTOR ( 'NONE', #12262, 999.9999999999998863 ) ;
#32327 = EDGE_LOOP ( 'NONE', ( #35908, #12327, #32217, #19803 ) ) ;
#32328 = VECTOR ( 'NONE', #27317, 1000.000000000000227 ) ;
#32329 = EDGE_LOOP ( 'NONE', ( #35201, #26437, #13045, #18463, #17257 ) ) ;
#32330 = ORIENTED_EDGE ( 'NONE', *, *, #52157, .T. ) ;
#32331 = ORIENTED_EDGE ( 'NONE', *, *, #34231, .F. ) ;
#32332 = LINE ( 'NONE', #36042, #51408 ) ;
#32333 = PLANE ( 'NONE',  #8594 ) ;
#32334 = EDGE_CURVE ( 'NONE', #12044, #29102, #29916, .T. ) ;
#32335 = ORIENTED_EDGE ( 'NONE', *, *, #16285, .T. ) ;
#32336 = LINE ( 'NONE', #11284, #55795 ) ;
#32337 = ORIENTED_EDGE ( 'NONE', *, *, #52736, .F. ) ;
#32338 = ADVANCED_FACE ( 'NONE', ( #4625 ), #38732, .F. ) ;
#32339 = ADVANCED_FACE ( 'NONE', ( #12866 ), #30189, .F. ) ;
#32340 = AXIS2_PLACEMENT_3D ( 'NONE', #24705, #12778, #38333 ) ;
#32341 = DIRECTION ( 'NONE',  ( -0.7660212471507179544, -0.6427876096865405842, -0.005961354470445141482 ) ) ;
#32342 = CARTESIAN_POINT ( 'NONE',  ( -23.33849165029409889, 0.000000000000000000, 5.946783852668351855 ) ) ;
#32343 = CARTESIAN_POINT ( 'NONE',  ( -14.46888367232926420, 0.000000000000000000, 12.59025272694991315 ) ) ;
#32344 = ORIENTED_EDGE ( 'NONE', *, *, #15506, .T. ) ;
#32345 = VECTOR ( 'NONE', #38069, 999.9999999999998863 ) ;
#32346 = DIRECTION ( 'NONE',  ( 0.5364919789714477361, 0.6444004775717706579, 0.5449076811759711036 ) ) ;
#32347 = CARTESIAN_POINT ( 'NONE',  ( -18.39746900504187010, 0.000000000000000000, 14.03700784672088808 ) ) ;
#32348 = EDGE_CURVE ( 'NONE', #18224, #49166, #10593, .T. ) ;
#32349 = VECTOR ( 'NONE', #50075, 999.9999999999998863 ) ;
#32350 = FACE_OUTER_BOUND ( 'NONE', #10595, .T. ) ;
#32351 = EDGE_CURVE ( 'NONE', #50681, #34828, #31312, .T. ) ;
#32352 = CARTESIAN_POINT ( 'NONE',  ( -24.27063949748155380, 0.000000000000000000, 6.308861732390097288 ) ) ;
#32353 = DIRECTION ( 'NONE',  ( 0.5449076811759707706, 0.6444004775717708799, -0.5364919789714476250 ) ) ;
#32354 = AXIS2_PLACEMENT_3D ( 'NONE', #47347, #13002, #44236 ) ;
#32355 = FACE_OUTER_BOUND ( 'NONE', #10874, .T. ) ;
#32356 = DIRECTION ( 'NONE',  ( -0.9999697198139514409, -0.000000000000000000, -0.007781995580013368816 ) ) ;
#32357 = DIRECTION ( 'NONE',  ( 0.8531650599175529814, -0.4028455766673920135, -0.3313982828793697877 ) ) ;
#32358 = CARTESIAN_POINT ( 'NONE',  ( -10.16199474375293299, 7.791337327497334542, 0.7288902856039674027 ) ) ;
#32359 = ORIENTED_EDGE ( 'NONE', *, *, #10148, .T. ) ;
#32360 = CARTESIAN_POINT ( 'NONE',  ( -20.54049170961573267, 0.000000000000000000, 4.660556269540326646 ) ) ;
#32361 = ORIENTED_EDGE ( 'NONE', *, *, #49833, .T. ) ;
#32362 = EDGE_CURVE ( 'NONE', #30431, #52995, #40680, .T. ) ;
#32363 = VECTOR ( 'NONE', #46083, 1000.000000000000227 ) ;
#32364 = CARTESIAN_POINT ( 'NONE',  ( -30.79489622823572859, -0.1191753592594197858, 8.743409918460921304 ) ) ;
#32365 = PLANE ( 'NONE',  #28652 ) ;
#32366 = DIRECTION ( 'NONE',  ( 0.7660212471507180654, -0.6427876096865404731, 0.005961354470445141482 ) ) ;
#32367 = LINE ( 'NONE', #45385, #54067 ) ;
#32368 = CARTESIAN_POINT ( 'NONE',  ( -7.804705230638511182, -7.507922520789255039, -0.1867610151785078776 ) ) ;
#32369 = CARTESIAN_POINT ( 'NONE',  ( -11.94039625119647141, 2.391131607591507002, 1.243697515788635632 ) ) ;
#32370 = DIRECTION ( 'NONE',  ( -0.6427681459581293666, -0.7660444431189770143, -0.005002170337467561935 ) ) ;
#32371 = VECTOR ( 'NONE', #8800, 999.9999999999998863 ) ;
#32372 = EDGE_CURVE ( 'NONE', #8391, #46530, #10005, .T. ) ;
#32373 = VECTOR ( 'NONE', #49403, 999.9999999999998863 ) ;
#32374 = CARTESIAN_POINT ( 'NONE',  ( 2.072287782118878319, 0.000000000000000000, -2.950529333540147015 ) ) ;
#32375 = CARTESIAN_POINT ( 'NONE',  ( -5.443235082016203208, 5.083326917256436595, -1.371155520332597323E-13 ) ) ;
#32376 = FACE_OUTER_BOUND ( 'NONE', #50411, .T. ) ;
#32377 = CARTESIAN_POINT ( 'NONE',  ( -18.67619601524082285, 0.000000000000000000, 3.936400510096834893 ) ) ;
#32378 = CARTESIAN_POINT ( 'NONE',  ( -33.59056157024009082, 0.000000000000000000, 9.729646585644761814 ) ) ;
#32379 = DIRECTION ( 'NONE',  ( 0.000000000000000000, 1.000000000000000000, 0.000000000000000000 ) ) ;
#32380 = CARTESIAN_POINT ( 'NONE',  ( -24.27063949748155380, 0.000000000000000000, 6.308861732390097288 ) ) ;
#32381 = LINE ( 'NONE', #36085, #30038 ) ;
#32382 = DIRECTION ( 'NONE',  ( 0.6427681459581294776, -0.7660444431189769032, 0.005002170337467562802 ) ) ;
#32383 = CARTESIAN_POINT ( 'NONE',  ( -13.08330893211609869, 0.000000000000000000, 1.763933231766363630 ) ) ;
#32384 = DIRECTION ( 'NONE',  ( 0.000000000000000000, 1.000000000000000000, 0.000000000000000000 ) ) ;
#32385 = VECTOR ( 'NONE', #22447, 1000.000000000000227 ) ;
#32386 = VERTEX_POINT ( 'NONE', #5750 ) ;
#32387 = ORIENTED_EDGE ( 'NONE', *, *, #1429, .F. ) ;
#32388 = FACE_OUTER_BOUND ( 'NONE', #20722, .T. ) ;
#32389 = LINE ( 'NONE', #45991, #47565 ) ;
#32390 = ORIENTED_EDGE ( 'NONE', *, *, #37962, .T. ) ;
#32391 = CARTESIAN_POINT ( 'NONE',  ( -23.33849165029409889, 0.000000000000000000, 5.946783852668351855 ) ) ;
#32392 = AXIS2_PLACEMENT_3D ( 'NONE', #45620, #32840, #40821 ) ;
#32393 = EDGE_CURVE ( 'NONE', #24617, #27675, #48658, .T. ) ;
#32394 = ORIENTED_EDGE ( 'NONE', *, *, #41651, .T. ) ;
#32395 = DIRECTION ( 'NONE',  ( 0.005961354470445682716, -0.6427876096865404731, -0.7660212471507180654 ) ) ;
#32396 = VECTOR ( 'NONE', #6376, 1000.000000000000000 ) ;
#32397 = VERTEX_POINT ( 'NONE', #40099 ) ;
#32398 = EDGE_LOOP ( 'NONE', ( #34504, #31718, #38875, #25597 ) ) ;
#32399 = ADVANCED_FACE ( 'NONE', ( #40393 ), #36398, .F. ) ;
#32400 = VERTEX_POINT ( 'NONE', #1490 ) ;
#32401 = CARTESIAN_POINT ( 'NONE',  ( -18.26277741321443671, -0.1191753592594162470, 9.579601904462350603 ) ) ;
#32402 = CARTESIAN_POINT ( 'NONE',  ( -17.20343699261858816, 2.553033558614008047, 3.282875753485510195 ) ) ;
#32403 = CARTESIAN_POINT ( 'NONE',  ( -15.96710241509184058, -0.1191753592594218814, 13.13259134697452879 ) ) ;
#32404 = EDGE_CURVE ( 'NONE', #39021, #11131, #19351, .T. ) ;
#32405 = ADVANCED_FACE ( 'NONE', ( #49476 ), #44933, .F. ) ;
#32406 = EDGE_CURVE ( 'NONE', #35922, #37629, #6313, .T. ) ;
#32407 = AXIS2_PLACEMENT_3D ( 'NONE', #13288, #3622, #8172 ) ;
#32408 = ORIENTED_EDGE ( 'NONE', *, *, #15912, .T. ) ;
#32409 = ORIENTED_EDGE ( 'NONE', *, *, #30139, .T. ) ;
#32410 = EDGE_CURVE ( 'NONE', #20361, #20373, #53447, .T. ) ;
#32411 = DIRECTION ( 'NONE',  ( -0.2426528472758542054, 0.7422098413412800966, -0.6246952433987894571 ) ) ;
#32412 = VERTEX_POINT ( 'NONE', #27056 ) ;
#32413 = CARTESIAN_POINT ( 'NONE',  ( -15.89648212642976510, -0.1191753592594206462, 4.058035914435935254 ) ) ;
#32414 = ORIENTED_EDGE ( 'NONE', *, *, #11241, .T. ) ;
#32415 = DIRECTION ( 'NONE',  ( 0.2426528472758542054, 0.7422098413412800966, 0.6246952433987894571 ) ) ;
#32416 = CARTESIAN_POINT ( 'NONE',  ( 5.385059872733033437, 0.000000000000000000, 0.6896135826588394302 ) ) ;
#32417 = ORIENTED_EDGE ( 'NONE', *, *, #35694, .T. ) ;
#32418 = CARTESIAN_POINT ( 'NONE',  ( -24.66083326546969801, 18.30078199617196688, -4.553899816365563957 ) ) ;
#32419 = EDGE_CURVE ( 'NONE', #40411, #16890, #13985, .T. ) ;
#32420 = EDGE_CURVE ( 'NONE', #44220, #47606, #23363, .T. ) ;
#32421 = FACE_OUTER_BOUND ( 'NONE', #26277, .T. ) ;
#32422 = ORIENTED_EDGE ( 'NONE', *, *, #17978, .F. ) ;
#32423 = FACE_OUTER_BOUND ( 'NONE', #4464, .T. ) ;
#32424 = EDGE_CURVE ( 'NONE', #25263, #32502, #40932, .T. ) ;
#32425 = LINE ( 'NONE', #49727, #4741 ) ;
#32426 = VERTEX_POINT ( 'NONE', #22780 ) ;
#32427 = EDGE_CURVE ( 'NONE', #34236, #37134, #2016, .T. ) ;
#32428 = DIRECTION ( 'NONE',  ( 0.000000000000000000, -0.000000000000000000, -1.000000000000000000 ) ) ;
#32429 = DIRECTION ( 'NONE',  ( -0.8531650599175527594, 0.4028455766673922356, 0.3313982828793700652 ) ) ;
#32430 = CARTESIAN_POINT ( 'NONE',  ( -11.30636317915456779, -0.1191753592594197858, 11.32220194836580340 ) ) ;
#32431 = DIRECTION ( 'NONE',  ( 0.7660212471507180654, -0.6427876096865404731, 0.005961354470445141482 ) ) ;
#32432 = LINE ( 'NONE', #7138, #6810 ) ;
#32433 = DIRECTION ( 'NONE',  ( -0.005002170337468016433, -0.7660444431189770143, 0.6427681459581293666 ) ) ;
#32434 = AXIS2_PLACEMENT_3D ( 'NONE', #726, #30269, #38500 ) ;
#32435 = CARTESIAN_POINT ( 'NONE',  ( -64.65687102648206519, -11.12218126798172690, -1.598589950288901385 ) ) ;
#32436 = ORIENTED_EDGE ( 'NONE', *, *, #45917, .F. ) ;
#32437 = CARTESIAN_POINT ( 'NONE',  ( -19.12962290826653700, 0.000000000000000000, 14.40064212555863854 ) ) ;
#32438 = PLANE ( 'NONE',  #53160 ) ;
#32439 = CARTESIAN_POINT ( 'NONE',  ( -65.59416307815027380, 4.336808689942017736E-15, 0.3806443636350875237 ) ) ;
#32440 = ORIENTED_EDGE ( 'NONE', *, *, #19801, .F. ) ;
#32441 = CARTESIAN_POINT ( 'NONE',  ( -12.44241612666018071, 0.7721120973665049902, 1.490354282959377441 ) ) ;
#32442 = DIRECTION ( 'NONE',  ( -0.5364919789714478471, 0.6444004775717705469, -0.5449076811759709926 ) ) ;
#32443 = VECTOR ( 'NONE', #28488, 1000.000000000000227 ) ;
#32444 = LINE ( 'NONE', #41508, #7738 ) ;
#32445 = PLANE ( 'NONE',  #45972 ) ;
#32446 = DIRECTION ( 'NONE',  ( 0.000000000000000000, -1.000000000000000000, 0.000000000000000000 ) ) ;
#32447 = EDGE_LOOP ( 'NONE', ( #14441, #12551, #36127, #6073 ) ) ;
#32448 = ORIENTED_EDGE ( 'NONE', *, *, #30287, .T. ) ;
#32449 = CARTESIAN_POINT ( 'NONE',  ( -20.47626320180702919, -0.03228989815065526348, 4.833966904781533458 ) ) ;
#32450 = ADVANCED_FACE ( 'NONE', ( #15124 ), #32445, .F. ) ;
#32451 = LINE ( 'NONE', #53198, #51980 ) ;
#32452 = ORIENTED_EDGE ( 'NONE', *, *, #4015, .T. ) ;
#32453 = DIRECTION ( 'NONE',  ( -0.9999697198139514409, -0.000000000000000000, -0.007781995580013368816 ) ) ;
#32454 = EDGE_CURVE ( 'NONE', #46860, #606, #14295, .T. ) ;
#32455 = ORIENTED_EDGE ( 'NONE', *, *, #52200, .F. ) ;
#32456 = LINE ( 'NONE', #40692, #20151 ) ;
#32457 = ORIENTED_EDGE ( 'NONE', *, *, #20747, .F. ) ;
#32458 = ORIENTED_EDGE ( 'NONE', *, *, #47523, .T. ) ;
#32459 = FACE_OUTER_BOUND ( 'NONE', #25340, .T. ) ;
#32460 = LINE ( 'NONE', #41240, #48609 ) ;
#32461 = DIRECTION ( 'NONE',  ( -0.005002170337468016433, -0.7660444431189770143, 0.6427681459581293666 ) ) ;
#32462 = EDGE_CURVE ( 'NONE', #47104, #48938, #1188, .T. ) ;
#32463 = ADVANCED_FACE ( 'NONE', ( #53188 ), #48911, .F. ) ;
#32464 = ADVANCED_FACE ( 'NONE', ( #55128 ), #16216, .F. ) ;
#32465 = ORIENTED_EDGE ( 'NONE', *, *, #7648, .T. ) ;
#32466 = DIRECTION ( 'NONE',  ( 0.005961354470445682716, -0.6427876096865404731, -0.7660212471507180654 ) ) ;
#32467 = VERTEX_POINT ( 'NONE', #49998 ) ;
#32468 = ADVANCED_FACE ( 'NONE', ( #11107 ), #15373, .F. ) ;
#32469 = EDGE_LOOP ( 'NONE', ( #50302, #8355, #34893, #12351 ) ) ;
#32470 = EDGE_LOOP ( 'NONE', ( #30219, #226, #24086, #46055 ) ) ;
#32471 = DIRECTION ( 'NONE',  ( 0.5449076811759707706, 0.6444004775717708799, -0.5364919789714476250 ) ) ;
#32472 = ORIENTED_EDGE ( 'NONE', *, *, #33166, .F. ) ;
#32473 = DIRECTION ( 'NONE',  ( 0.000000000000000000, -0.000000000000000000, -1.000000000000000000 ) ) ;
#32474 = VERTEX_POINT ( 'NONE', #11941 ) ;
#32475 = FACE_OUTER_BOUND ( 'NONE', #29766, .T. ) ;
#32476 = CARTESIAN_POINT ( 'NONE',  ( -18.59658094907401704, 0.000000000000000000, 5.614354428398334207 ) ) ;
#32477 = AXIS2_PLACEMENT_3D ( 'NONE', #15362, #11094, #49735 ) ;
#32478 = VERTEX_POINT ( 'NONE', #2847 ) ;
#32479 = CARTESIAN_POINT ( 'NONE',  ( -14.16589384654164441, 0.000000000000000000, 7.664821422546224561 ) ) ;
#32480 = ORIENTED_EDGE ( 'NONE', *, *, #28232, .T. ) ;
#32481 = EDGE_CURVE ( 'NONE', #7084, #46706, #46584, .T. ) ;
#32482 = DIRECTION ( 'NONE',  ( -0.005002170337468016433, -0.7660444431189770143, 0.6427681459581293666 ) ) ;
#32483 = DIRECTION ( 'NONE',  ( 0.6427681459581294776, -0.7660444431189769032, 0.005002170337467562802 ) ) ;
#32484 = FACE_OUTER_BOUND ( 'NONE', #16675, .T. ) ;
#32485 = FACE_OUTER_BOUND ( 'NONE', #34756, .T. ) ;
#32486 = EDGE_CURVE ( 'NONE', #29459, #10313, #33537, .T. ) ;
#32487 = LINE ( 'NONE', #40978, #42320 ) ;
#32488 = FACE_OUTER_BOUND ( 'NONE', #3416, .T. ) ;
#32489 = DIRECTION ( 'NONE',  ( 0.007781995580012663651, -3.146120232559066537E-19, -0.9999697198139514409 ) ) ;
#32490 = ORIENTED_EDGE ( 'NONE', *, *, #19920, .T. ) ;
#32492 = ORIENTED_EDGE ( 'NONE', *, *, #40344, .F. ) ;
#32491 = EDGE_CURVE ( 'NONE', #19751, #40803, #20485, .T. ) ;
#32493 = CARTESIAN_POINT ( 'NONE',  ( -56.63016842841614817, 4.129031330634377994, 2.385144069838411873 ) ) ;
#32494 = DIRECTION ( 'NONE',  ( 0.005961354470445682716, -0.6427876096865404731, -0.7660212471507180654 ) ) ;
#32495 = CARTESIAN_POINT ( 'NONE',  ( -19.98318713347071096, 0.000000000000000000, 4.664893342615989091 ) ) ;
#32496 = ADVANCED_FACE ( 'NONE', ( #7701 ), #25033, .F. ) ;
#32497 = DIRECTION ( 'NONE',  ( 0.5364919789714477361, 0.6444004775717706579, 0.5449076811759711036 ) ) ;
#32498 = DIRECTION ( 'NONE',  ( 0.6427681459581294776, -0.7660444431189769032, 0.005002170337467562802 ) ) ;
#32499 = ORIENTED_EDGE ( 'NONE', *, *, #9707, .T. ) ;
#32500 = FACE_OUTER_BOUND ( 'NONE', #38736, .T. ) ;
#32501 = CARTESIAN_POINT ( 'NONE',  ( 2.072287782118878319, 0.000000000000000000, -2.950529333540147015 ) ) ;
#32502 = VERTEX_POINT ( 'NONE', #50842 ) ;
#32503 = LINE ( 'NONE', #6940, #13016 ) ;
#32504 = CARTESIAN_POINT ( 'NONE',  ( -3.184760737835581335, 4.114927023055928501, -1.981304350158550776 ) ) ;
#32505 = ORIENTED_EDGE ( 'NONE', *, *, #2928, .T. ) ;
#32506 = CARTESIAN_POINT ( 'NONE',  ( -20.54204810873173415, 0.000000000000000000, 4.860550213503115558 ) ) ;
#32507 = DIRECTION ( 'NONE',  ( -0.005961354470445682716, -0.6427876096865404731, 0.7660212471507180654 ) ) ;
#32508 = CARTESIAN_POINT ( 'NONE',  ( -14.66887761629205222, 0.000000000000000000, 12.58869632783390990 ) ) ;
#32509 = CARTESIAN_POINT ( 'NONE',  ( -14.46888367232926420, 0.000000000000000000, 12.59025272694991315 ) ) ;
#32510 = FACE_BOUND ( 'NONE', #4927, .T. ) ;
#32511 = VERTEX_POINT ( 'NONE', #36982 ) ;
#32512 = VERTEX_POINT ( 'NONE', #3443 ) ;
#32513 = CARTESIAN_POINT ( 'NONE',  ( -17.74404816805336793, 0.000000000000000000, 3.574322630375089460 ) ) ;
#32514 = CARTESIAN_POINT ( 'NONE',  ( -10.37421533196711465, -0.1191753592594197858, 10.96012406864405975 ) ) ;
#32515 = LINE ( 'NONE', #23435, #2494 ) ;
#32516 = VECTOR ( 'NONE', #37804, 1000.000000000000227 ) ;
#32517 = CARTESIAN_POINT ( 'NONE',  ( -23.33693525117809386, 0.000000000000000000, 5.746789908705562944 ) ) ;
#32518 = CARTESIAN_POINT ( 'NONE',  ( -9.946799079403195520, 0.000000000000000000, 2.896338486107371324 ) ) ;
#32519 = ORIENTED_EDGE ( 'NONE', *, *, #39586, .F. ) ;
#32520 = FACE_OUTER_BOUND ( 'NONE', #11125, .T. ) ;
#32521 = FACE_OUTER_BOUND ( 'NONE', #24129, .T. ) ;
#32522 = CARTESIAN_POINT ( 'NONE',  ( -19.92277643783922869, 21.15585550648971491, -4.281362112901368810 ) ) ;
#32523 = EDGE_LOOP ( 'NONE', ( #3829, #26163, #22178, #7863 ) ) ;
#32524 = DIRECTION ( 'NONE',  ( 0.9999697198139515519, 0.000000000000000000, 0.007781995580013368816 ) ) ;
#32525 = FACE_OUTER_BOUND ( 'NONE', #40002, .T. ) ;
#32526 = LINE ( 'NONE', #20280, #25735 ) ;
#32527 = ADVANCED_FACE ( 'NONE', ( #15942 ), #41755, .F. ) ;
#32528 = ORIENTED_EDGE ( 'NONE', *, *, #32419, .F. ) ;
#32529 = CARTESIAN_POINT ( 'NONE',  ( -26.13337879274045505, 0.000000000000000000, 6.833023547870798353 ) ) ;
#32530 = ORIENTED_EDGE ( 'NONE', *, *, #19893, .F. ) ;
#32531 = ADVANCED_FACE ( 'NONE', ( #7403 ), #16482, .F. ) ;
#32532 = ADVANCED_FACE ( 'NONE', ( #28154 ), #42045, .F. ) ;
#32533 = EDGE_LOOP ( 'NONE', ( #33326, #5638, #20207, #39215 ) ) ;
#32534 = ORIENTED_EDGE ( 'NONE', *, *, #43659, .F. ) ;
#32535 = CARTESIAN_POINT ( 'NONE',  ( -29.16342252716179928, 15.82076599933325944, 4.730794752401083159 ) ) ;
#32536 = ORIENTED_EDGE ( 'NONE', *, *, #31181, .F. ) ;
#32537 = ORIENTED_EDGE ( 'NONE', *, *, #12316, .T. ) ;
#32538 = DIRECTION ( 'NONE',  ( 0.9999697198139515519, 0.000000000000000000, 0.007781995580013368816 ) ) ;
#32539 = ORIENTED_EDGE ( 'NONE', *, *, #13665, .F. ) ;
#32540 = ORIENTED_EDGE ( 'NONE', *, *, #23774, .F. ) ;
#32541 = DIRECTION ( 'NONE',  ( -0.005961354470445682716, -0.6427876096865404731, 0.7660212471507180654 ) ) ;
#32542 = ORIENTED_EDGE ( 'NONE', *, *, #9954, .T. ) ;
#32543 = ORIENTED_EDGE ( 'NONE', *, *, #54830, .T. ) ;
#32544 = EDGE_LOOP ( 'NONE', ( #22316, #22964, #49830 ) ) ;
#32545 = CARTESIAN_POINT ( 'NONE',  ( -12.74192496657627949, 0.000000000000000000, 3.813256365977633067 ) ) ;
#32546 = PLANE ( 'NONE',  #1304 ) ;
#32547 = PLANE ( 'NONE',  #1498 ) ;
#32548 = DIRECTION ( 'NONE',  ( -0.005002170337468016433, -0.7660444431189770143, 0.6427681459581293666 ) ) ;
#32549 = ORIENTED_EDGE ( 'NONE', *, *, #41880, .F. ) ;
#32550 = CARTESIAN_POINT ( 'NONE',  ( -13.47120481629566058, 0.000000000000000000, 3.807580941557616949 ) ) ;
#32551 = VERTEX_POINT ( 'NONE', #19651 ) ;
#32552 = AXIS2_PLACEMENT_3D ( 'NONE', #35023, #8904, #52333 ) ;
#32553 = ORIENTED_EDGE ( 'NONE', *, *, #49173, .T. ) ;
#32554 = DIRECTION ( 'NONE',  ( 0.007781995580012663651, 0.000000000000000000, -0.9999697198139515519 ) ) ;
#32555 = EDGE_CURVE ( 'NONE', #4269, #26373, #54278, .T. ) ;
#32556 = CARTESIAN_POINT ( 'NONE',  ( -32.77407650832405750, 13.73615395135863970, -4.840648455043430332 ) ) ;
#32557 = CARTESIAN_POINT ( 'NONE',  ( -15.81552396586975640, -0.03228989815065647778, 3.023577506172806739 ) ) ;
#32558 = EDGE_CURVE ( 'NONE', #8547, #23151, #24449, .T. ) ;
#32559 = DIRECTION ( 'NONE',  ( 0.9999697198139515519, 0.000000000000000000, 0.007781995580013368816 ) ) ;
#32560 = CARTESIAN_POINT ( 'NONE',  ( -14.87661172084004946, 0.000000000000000000, 5.273972019284645540 ) ) ;
#32561 = ORIENTED_EDGE ( 'NONE', *, *, #26676, .F. ) ;
#32562 = PLANE ( 'NONE',  #48295 ) ;
#32563 = ORIENTED_EDGE ( 'NONE', *, *, #19834, .T. ) ;
#32564 = DIRECTION ( 'NONE',  ( 0.6427681459581294776, -0.7660444431189769032, 0.005002170337467562802 ) ) ;
#32565 = DIRECTION ( 'NONE',  ( 0.9999697198139515519, 0.000000000000000000, 0.007781995580013368816 ) ) ;
#32566 = CARTESIAN_POINT ( 'NONE',  ( -24.24106128977693331, 18.66269258478600079, -4.531817629136046577 ) ) ;
#32567 = EDGE_CURVE ( 'NONE', #16295, #22163, #24194, .T. ) ;
#32568 = DIRECTION ( 'NONE',  ( -0.5449076811759708816, 0.6444004775717707689, 0.5364919789714475140 ) ) ;
#32569 = CARTESIAN_POINT ( 'NONE',  ( -13.63251841181027402, 3.848249166794011522, 1.854485548694981611 ) ) ;
#32570 = ORIENTED_EDGE ( 'NONE', *, *, #529, .F. ) ;
#32571 = LINE ( 'NONE', #24046, #30293 ) ;
#32572 = DIRECTION ( 'NONE',  ( 0.5364919789714477361, 0.6444004775717706579, 0.5449076811759711036 ) ) ;
#32573 = PLANE ( 'NONE',  #49058 ) ;
#32574 = CARTESIAN_POINT ( 'NONE',  ( -69.54161822237450963, 1.150459406892988756, -7.491897809418650134 ) ) ;
#32575 = CARTESIAN_POINT ( 'NONE',  ( -20.46460680255002984, 1.419719901456506728, 7.160471608229209473 ) ) ;
#32576 = DIRECTION ( 'NONE',  ( 0.005961354470445682716, -0.6427876096865404731, -0.7660212471507180654 ) ) ;
#32577 = LINE ( 'NONE', #53339, #35586 ) ;
#32578 = CARTESIAN_POINT ( 'NONE',  ( -10.68757514314370916, 0.000000000000000000, 4.367901874718414845 ) ) ;
#32579 = CARTESIAN_POINT ( 'NONE',  ( -3.789853545709553462, 5.589773622088367588, -1.746265754542047910 ) ) ;
#32580 = EDGE_CURVE ( 'NONE', #30608, #47582, #15638, .T. ) ;
#32581 = STYLED_ITEM ( 'NONE', ( #1405 ), #27288 ) ;
#32582 = EDGE_CURVE ( 'NONE', #35922, #49529, #11404, .T. ) ;
#32583 = ORIENTED_EDGE ( 'NONE', *, *, #16667, .F. ) ;
#32584 = EDGE_CURVE ( 'NONE', #34233, #46872, #21325, .T. ) ;
#32585 = VERTEX_POINT ( 'NONE', #56235 ) ;
#32586 = ORIENTED_EDGE ( 'NONE', *, *, #32956, .T. ) ;
#32587 = VERTEX_POINT ( 'NONE', #17323 ) ;
#32588 = EDGE_LOOP ( 'NONE', ( #47954, #5361, #48037, #28534 ) ) ;
#32589 = CARTESIAN_POINT ( 'NONE',  ( -19.63656972920071198, -0.1191753592594160388, 6.983586246353969962 ) ) ;
#32590 = DIRECTION ( 'NONE',  ( 0.007781995580012662783, 0.000000000000000000, -0.9999697198139514409 ) ) ;
#32591 = ORIENTED_EDGE ( 'NONE', *, *, #213, .T. ) ;
#32592 = VERTEX_POINT ( 'NONE', #34958 ) ;
#32593 = ORIENTED_EDGE ( 'NONE', *, *, #46105, .T. ) ;
#32594 = ORIENTED_EDGE ( 'NONE', *, *, #52966, .T. ) ;
#32595 = ADVANCED_FACE ( 'NONE', ( #277 ), #4302, .F. ) ;
#32596 = CARTESIAN_POINT ( 'NONE',  ( -66.73349045206065000, -9.347208724145792402, -4.549856479217463168 ) ) ;
#32597 = LINE ( 'NONE', #40836, #53671 ) ;
#32598 = LINE ( 'NONE', #28325, #53154 ) ;
#32599 = EDGE_LOOP ( 'NONE', ( #46597, #29051, #43299, #55483 ) ) ;
#32600 = FACE_OUTER_BOUND ( 'NONE', #28, .T. ) ;
#32601 = LINE ( 'NONE', #50751, #22815 ) ;
#32602 = DIRECTION ( 'NONE',  ( 0.8660254037844380415, 0.5000000000000011102, 0.000000000000000000 ) ) ;
#32603 = DIRECTION ( 'NONE',  ( -0.5449076811759708816, 0.6444004775717707689, 0.5364919789714475140 ) ) ;
#32604 = DIRECTION ( 'NONE',  ( 0.9999697198139515519, 0.000000000000000000, 0.007781995580013368816 ) ) ;
#32605 = DIRECTION ( 'NONE',  ( -0.5449076811759708816, 0.6444004775717707689, 0.5364919789714475140 ) ) ;
#32606 = CARTESIAN_POINT ( 'NONE',  ( -19.98893524048127190, 0.000000000000000000, 5.403512749131516024 ) ) ;
#32607 = CARTESIAN_POINT ( 'NONE',  ( -13.95440368855772562, 0.000000000000000000, 6.189139008631170391 ) ) ;
#32608 = DIRECTION ( 'NONE',  ( 0.000000000000000000, -1.000000000000000000, 0.000000000000000000 ) ) ;
#32609 = ORIENTED_EDGE ( 'NONE', *, *, #49879, .F. ) ;
#32610 = PLANE ( 'NONE',  #36519 ) ;
#32611 = ORIENTED_EDGE ( 'NONE', *, *, #47186, .T. ) ;
#32612 = LINE ( 'NONE', #28342, #54623 ) ;
#32613 = DIRECTION ( 'NONE',  ( -0.6427681459581293666, -0.7660444431189770143, -0.005002170337467561935 ) ) ;
#32614 = DIRECTION ( 'NONE',  ( -0.005961354470445682716, -0.6427876096865404731, 0.7660212471507180654 ) ) ;
#32615 = LINE ( 'NONE', #19004, #24110 ) ;
#32616 = EDGE_CURVE ( 'NONE', #46922, #41711, #34116, .T. ) ;
#32617 = CARTESIAN_POINT ( 'NONE',  ( -10.47421230394850866, 0.000000000000000000, 10.95934586908605723 ) ) ;
#32618 = LINE ( 'NONE', #33198, #51278 ) ;
#32619 = DIRECTION ( 'NONE',  ( 0.9999697198139515519, 0.000000000000000000, 0.007781995580013368816 ) ) ;
#32620 = SURFACE_SIDE_STYLE ('',( #28349 ) ) ;
#32621 = CARTESIAN_POINT ( 'NONE',  ( -11.13054826722768098, 24.50000000000005684, 3.000000000000000444 ) ) ;
#32622 = CARTESIAN_POINT ( 'NONE',  ( -11.67244013076689946, 0.000000000000000000, 11.50401908778467863 ) ) ;
#32623 = CARTESIAN_POINT ( 'NONE',  ( -11.37100670409528114, 0.000000000000000000, 6.778581727343776286 ) ) ;
#32624 = FACE_OUTER_BOUND ( 'NONE', #22566, .T. ) ;
#32625 = CARTESIAN_POINT ( 'NONE',  ( 2.072287782118878319, 0.000000000000000000, -2.950529333540147015 ) ) ;
#32626 = EDGE_CURVE ( 'NONE', #19674, #49645, #29851, .T. ) ;
#32627 = CARTESIAN_POINT ( 'NONE',  ( -26.13337879274045505, 0.000000000000000000, 6.833023547870798353 ) ) ;
#32628 = CARTESIAN_POINT ( 'NONE',  ( -61.10213307005876260, 6.758246409053501047, 2.999999999999993339 ) ) ;
#32629 = EDGE_CURVE ( 'NONE', #24940, #33221, #39495, .T. ) ;
#32630 = DIRECTION ( 'NONE',  ( 0.000000000000000000, -0.000000000000000000, -1.000000000000000000 ) ) ;
#32631 = EDGE_CURVE ( 'NONE', #36809, #52840, #21616, .T. ) ;
#32632 = LINE ( 'NONE', #10216, #20154 ) ;
#32633 = ORIENTED_EDGE ( 'NONE', *, *, #26490, .T. ) ;
#32634 = PLANE ( 'NONE',  #3106 ) ;
#32635 = ORIENTED_EDGE ( 'NONE', *, *, #10810, .F. ) ;
#32636 = B_SPLINE_CURVE_WITH_KNOTS ( 'NONE', 3,
 ( #36225, #53527, #36485, #53802, #33365, #50926, #20579, #19991, #42146, #33616, #37609, #50393, #33071, #6670 ),
 .UNSPECIFIED., .F., .F.,
 ( 4, 2, 2, 2, 2, 2, 4 ),
 ( 1.387778780781443673E-17, 0.0008437472854879791203, 0.001265620928231961416, 0.001687494570975943495, 0.002109368213719925791, 0.002531241856463908087, 0.003374989141951898700 ),
 .UNSPECIFIED. ) ;
#32637 = LINE ( 'NONE', #11044, #25979 ) ;
#32638 = DIRECTION ( 'NONE',  ( -0.7660212471507179544, -0.6427876096865405842, -0.005961354470445141482 ) ) ;
#32639 = EDGE_CURVE ( 'NONE', #29014, #53080, #51129, .T. ) ;
#32640 = ORIENTED_EDGE ( 'NONE', *, *, #55662, .F. ) ;
#32641 = EDGE_CURVE ( 'NONE', #29959, #14373, #21869, .T. ) ;
#32642 = DIRECTION ( 'NONE',  ( -0.005961354470445682716, -0.6427876096865404731, 0.7660212471507180654 ) ) ;
#32643 = ORIENTED_EDGE ( 'NONE', *, *, #40716, .F. ) ;
#32644 = DIRECTION ( 'NONE',  ( 0.5449076811759707706, 0.6444004775717708799, -0.5364919789714476250 ) ) ;
#32645 = EDGE_CURVE ( 'NONE', #53603, #33755, #8848, .T. ) ;
#32646 = AXIS2_PLACEMENT_3D ( 'NONE', #43646, #5057, #34572 ) ;
#32647 = ORIENTED_EDGE ( 'NONE', *, *, #21905, .F. ) ;
#32648 = ORIENTED_EDGE ( 'NONE', *, *, #17398, .T. ) ;
#32649 = ORIENTED_EDGE ( 'NONE', *, *, #1491, .T. ) ;
#32650 = PLANE ( 'NONE',  #20259 ) ;
#32651 = PLANE ( 'NONE',  #21421 ) ;
#32652 = DIRECTION ( 'NONE',  ( 0.7660212471507180654, -0.6427876096865404731, 0.005961354470445141482 ) ) ;
#32653 = ADVANCED_FACE ( 'NONE', ( #51969 ), #7996, .F. ) ;
#32654 = ORIENTED_EDGE ( 'NONE', *, *, #41373, .F. ) ;
#32655 = VERTEX_POINT ( 'NONE', #17071 ) ;
#32656 = ADVANCED_FACE ( 'NONE', ( #12535 ), #42610, .F. ) ;
#32657 = DIRECTION ( 'NONE',  ( 0.9999697198139515519, 0.000000000000000000, 0.007781995580013368816 ) ) ;
#32658 = ORIENTED_EDGE ( 'NONE', *, *, #54975, .T. ) ;
#32659 = DIRECTION ( 'NONE',  ( -0.5364919789714478471, 0.6444004775717705469, -0.5449076811759709926 ) ) ;
#32660 = ORIENTED_EDGE ( 'NONE', *, *, #13384, .F. ) ;
#32661 = DIRECTION ( 'NONE',  ( 0.000000000000000000, -1.000000000000000000, 0.000000000000000000 ) ) ;
#32662 = CARTESIAN_POINT ( 'NONE',  ( -10.88469503360121848, 0.000000000000000000, 3.997035772344645910 ) ) ;
#32663 = ORIENTED_EDGE ( 'NONE', *, *, #53792, .F. ) ;
#32664 = CARTESIAN_POINT ( 'NONE',  ( -15.88130887279446490, 0.000000000000000000, 3.050160814894388839 ) ) ;
#32665 = CARTESIAN_POINT ( 'NONE',  ( -19.60834386242827776, 0.000000000000000000, 4.298478389818581213 ) ) ;
#32666 = VERTEX_POINT ( 'NONE', #26151 ) ;
#32667 = CARTESIAN_POINT ( 'NONE',  ( -10.22006419279734146, 0.000000000000000000, 4.002208083228659063 ) ) ;
#32668 = CARTESIAN_POINT ( 'NONE',  ( -15.10628516568717572, 0.000000000000000000, 9.086167745620324254 ) ) ;
#32669 = LINE ( 'NONE', #2570, #8385 ) ;
#32670 = ORIENTED_EDGE ( 'NONE', *, *, #36293, .T. ) ;
#32671 = DIRECTION ( 'NONE',  ( 0.000000000000000000, -0.000000000000000000, -1.000000000000000000 ) ) ;
#32672 = CARTESIAN_POINT ( 'NONE',  ( -18.67619601524082285, 0.000000000000000000, 3.936400510096834893 ) ) ;
#32673 = CARTESIAN_POINT ( 'NONE',  ( -14.88367748223989118, 0.000000000000000000, 6.181907185095151469 ) ) ;
#32674 = EDGE_CURVE ( 'NONE', #55170, #8704, #3703, .T. ) ;
#32675 = DIRECTION ( 'NONE',  ( -0.5449076811759708816, 0.6444004775717707689, 0.5364919789714475140 ) ) ;
#32676 = LINE ( 'NONE', #25018, #44866 ) ;
#32677 = CARTESIAN_POINT ( 'NONE',  ( -27.06708303904391144, 0.000000000000000000, 7.395095371555332697 ) ) ;
#32678 = AXIS2_PLACEMENT_3D ( 'NONE', #17913, #48252, #56232 ) ;
#32679 = CARTESIAN_POINT ( 'NONE',  ( -65.54473273541158562, -11.22399610260319314, 5.092367036313483197 ) ) ;
#32680 = ORIENTED_EDGE ( 'NONE', *, *, #2651, .F. ) ;
#32681 = FACE_OUTER_BOUND ( 'NONE', #32869, .T. ) ;
#32682 = DIRECTION ( 'NONE',  ( -0.5449076811759708816, 0.6444004775717707689, 0.5364919789714475140 ) ) ;
#32683 = CARTESIAN_POINT ( 'NONE',  ( -67.03785620394307898, -0.6009241746136663176, 0.6802539881083679019 ) ) ;
#32684 = VERTEX_POINT ( 'NONE', #34387 ) ;
#32685 = LINE ( 'NONE', #11677, #25661 ) ;
#32686 = CARTESIAN_POINT ( 'NONE',  ( -17.74560456716937296, 0.000000000000000000, 3.774316574337878372 ) ) ;
#32687 = ADVANCED_FACE ( 'NONE', ( #47147 ), #21023, .F. ) ;
#32688 = LINE ( 'NONE', #14824, #3184 ) ;
#32689 = CARTESIAN_POINT ( 'NONE',  ( -18.19747506107908563, 0.000000000000000000, 14.03856424583689311 ) ) ;
#32690 = EDGE_CURVE ( 'NONE', #34394, #25528, #26405, .T. ) ;
#32691 = LINE ( 'NONE', #7151, #13877 ) ;
#32692 = ORIENTED_EDGE ( 'NONE', *, *, #35463, .F. ) ;
#32693 = VERTEX_POINT ( 'NONE', #12796 ) ;
#32694 = CARTESIAN_POINT ( 'NONE',  ( -25.83906187201940341, 17.72030447104181050, 4.604772761472839981 ) ) ;
#32695 = CARTESIAN_POINT ( 'NONE',  ( -25.20123094555300369, 0.000000000000000000, 6.470945668149052032 ) ) ;
#32696 = EDGE_LOOP ( 'NONE', ( #3162, #49414, #40553, #40372 ) ) ;
#32697 = ADVANCED_FACE ( 'NONE', ( #25873 ), #25567, .F. ) ;
#32698 = CARTESIAN_POINT ( 'NONE',  ( -12.60458797795435615, 0.000000000000000000, 11.86609696750642229 ) ) ;
#32699 = ORIENTED_EDGE ( 'NONE', *, *, #18647, .T. ) ;
#32700 = DIRECTION ( 'NONE',  ( -0.005002170337468016433, -0.7660444431189770143, 0.6427681459581293666 ) ) ;
#32701 = EDGE_CURVE ( 'NONE', #20126, #52593, #38929, .T. ) ;
#32702 = EDGE_LOOP ( 'NONE', ( #35076, #5775, #4306, #4423 ) ) ;
#32703 = EDGE_LOOP ( 'NONE', ( #32417, #17421, #30949, #45176 ) ) ;
#32704 = DIRECTION ( 'NONE',  ( 0.005961354470445682716, -0.6427876096865404731, -0.7660212471507180654 ) ) ;
#32705 = LINE ( 'NONE', #18844, #10564 ) ;
#32706 = DIRECTION ( 'NONE',  ( 0.3583679495452925523, 0.9335804264972047406, 0.000000000000000000 ) ) ;
#32707 = VERTEX_POINT ( 'NONE', #18762 ) ;
#32708 = ADVANCED_FACE ( 'NONE', ( #36338 ), #1117, .F. ) ;
#32710 = CARTESIAN_POINT ( 'NONE',  ( -15.90832530584190785, -5.051250379848162275, 11.15122795565880587 ) ) ;
#32709 = VECTOR ( 'NONE', #48300, 1000.000000000000000 ) ;
#32711 = EDGE_LOOP ( 'NONE', ( #13857, #8940, #26000, #5382, #26299, #7222 ) ) ;
#32712 = VECTOR ( 'NONE', #13625, 1000.000000000000227 ) ;
#32713 = ORIENTED_EDGE ( 'NONE', *, *, #25648, .F. ) ;
#32714 = ADVANCED_FACE ( 'NONE', ( #5409 ), #22716, .F. ) ;
#32715 = ORIENTED_EDGE ( 'NONE', *, *, #23636, .F. ) ;
#32716 = CARTESIAN_POINT ( 'NONE',  ( -19.42910703681909368, 21.15220053346460816, -4.255330291692488665 ) ) ;
#32717 = VERTEX_POINT ( 'NONE', #23559 ) ;
#32718 = CARTESIAN_POINT ( 'NONE',  ( -19.52872879626147196, 0.000000000000000000, 5.976432308120079639 ) ) ;
#32719 = ORIENTED_EDGE ( 'NONE', *, *, #15443, .T. ) ;
#32720 = CARTESIAN_POINT ( 'NONE',  ( -30.79567442779373110, 0.000000000000000000, 8.843406890442315316 ) ) ;
#32721 = PLANE ( 'NONE',  #53975 ) ;
#32722 = ORIENTED_EDGE ( 'NONE', *, *, #6377, .T. ) ;
#32723 = PLANE ( 'NONE',  #7788 ) ;
#32724 = VERTEX_POINT ( 'NONE', #48566 ) ;
#32725 = CARTESIAN_POINT ( 'NONE',  ( -14.10280672071693431, -0.1191753592594197858, 12.40843558753103792 ) ) ;
#32726 = LINE ( 'NONE', #50341, #44729 ) ;
#32727 = DIRECTION ( 'NONE',  ( 0.9999697198139515519, 0.000000000000000000, 0.007781995580013368816 ) ) ;
#32728 = DIRECTION ( 'NONE',  ( -0.005961354470445682716, -0.6427876096865404731, 0.7660212471507180654 ) ) ;
#32729 = PLANE ( 'NONE',  #6947 ) ;
#32730 = CARTESIAN_POINT ( 'NONE',  ( -20.94784447234964730, -4.403642575758159872, 12.04591360691983581 ) ) ;
#32731 = DIRECTION ( 'NONE',  ( -0.6427681459581293666, -0.7660444431189770143, -0.005002170337467561935 ) ) ;
#32732 = ORIENTED_EDGE ( 'NONE', *, *, #22715, .F. ) ;
#32733 = EDGE_CURVE ( 'NONE', #47190, #17834, #26367, .T. ) ;
#32734 = VECTOR ( 'NONE', #44561, 999.9999999999998863 ) ;
#32735 = ORIENTED_EDGE ( 'NONE', *, *, #13620, .T. ) ;
#32736 = VECTOR ( 'NONE', #18790, 1000.000000000000000 ) ;
#32737 = PLANE ( 'NONE',  #38252 ) ;
#32738 = DIRECTION ( 'NONE',  ( -0.6427681459581293666, -0.7660444431189770143, -0.005002170337467561935 ) ) ;
#32739 = ADVANCED_FACE ( 'NONE', ( #18452 ), #44306, .F. ) ;
#32740 = CARTESIAN_POINT ( 'NONE',  ( -29.86352658060627618, 0.000000000000000000, 8.481329010720569883 ) ) ;
#32741 = CARTESIAN_POINT ( 'NONE',  ( -30.79489622823572859, -0.1191753592594197858, 8.743409918460921304 ) ) ;
#32742 = DIRECTION ( 'NONE',  ( -0.8531650599175529814, -0.4028455766673920135, 0.3313982828793697877 ) ) ;
#32743 = ORIENTED_EDGE ( 'NONE', *, *, #730, .T. ) ;
#32744 = ADVANCED_FACE ( 'NONE', ( #26997 ), #27253, .F. ) ;
#32745 = FACE_OUTER_BOUND ( 'NONE', #49040, .T. ) ;
#32746 = DIRECTION ( 'NONE',  ( 0.000000000000000000, -0.000000000000000000, -1.000000000000000000 ) ) ;
#32747 = VERTEX_POINT ( 'NONE', #53390 ) ;
#32748 = CARTESIAN_POINT ( 'NONE',  ( -24.26908309836554878, 0.000000000000000000, 6.108867788427308376 ) ) ;
#32749 = CARTESIAN_POINT ( 'NONE',  ( -9.440078302826643508, -0.04820958850348456420, 2.690502017889039976 ) ) ;
#32750 = ORIENTED_EDGE ( 'NONE', *, *, #36436, .T. ) ;
#32751 = EDGE_CURVE ( 'NONE', #11552, #26953, #19018, .T. ) ;
#32752 = EDGE_CURVE ( 'NONE', #37228, #3166, #35242, .T. ) ;
#32753 = ADVANCED_FACE ( 'NONE', ( #52538 ), #30946, .F. ) ;
#32754 = DIRECTION ( 'NONE',  ( 0.5449076811759707706, 0.6444004775717708799, -0.5364919789714476250 ) ) ;
#32755 = CARTESIAN_POINT ( 'NONE',  ( -12.15116108492864377, 0.000000000000000000, 1.401855352044617975 ) ) ;
#32756 = VECTOR ( 'NONE', #30920, 1000.000000000000227 ) ;
#32757 = DIRECTION ( 'NONE',  ( 0.9999697198139515519, 0.000000000000000000, 0.007781995580013368816 ) ) ;
#32758 = DIRECTION ( 'NONE',  ( 0.005002170337468016433, -0.7660444431189770143, -0.6427681459581293666 ) ) ;
#32759 = VECTOR ( 'NONE', #37197, 999.9999999999998863 ) ;
#32760 = CARTESIAN_POINT ( 'NONE',  ( -12.60458797795435615, 0.000000000000000000, 11.86609696750642229 ) ) ;
#32761 = EDGE_LOOP ( 'NONE', ( #15884, #42907, #51159, #46705 ) ) ;
#32762 = ORIENTED_EDGE ( 'NONE', *, *, #8841, .F. ) ;
#32763 = DIRECTION ( 'NONE',  ( 0.5364919789714477361, 0.6444004775717706579, 0.5449076811759711036 ) ) ;
#32764 = PLANE ( 'NONE',  #14098 ) ;
#32765 = CARTESIAN_POINT ( 'NONE',  ( -24.26908309836554878, 0.000000000000000000, 6.108867788427308376 ) ) ;
#32766 = FACE_OUTER_BOUND ( 'NONE', #19765, .T. ) ;
#32767 = PLANE ( 'NONE',  #31035 ) ;
#32768 = EDGE_CURVE ( 'NONE', #32655, #29728, #1693, .T. ) ;
#32769 = CARTESIAN_POINT ( 'NONE',  ( -19.12962290826653700, 0.000000000000000000, 14.40064212555863854 ) ) ;
#32770 = ORIENTED_EDGE ( 'NONE', *, *, #17158, .F. ) ;
#32771 = DIRECTION ( 'NONE',  ( 0.5364919789714477361, 0.6444004775717706579, 0.5449076811759711036 ) ) ;
#32772 = EDGE_CURVE ( 'NONE', #4025, #20238, #32086, .T. ) ;
#32773 = CARTESIAN_POINT ( 'NONE',  ( -15.60102546347950536, 0.000000000000000000, 12.95077420755565356 ) ) ;
#32774 = CARTESIAN_POINT ( 'NONE',  ( -16.55824503503297151, 0.1245042932765017124, 3.109744084659005203 ) ) ;
#32775 = ORIENTED_EDGE ( 'NONE', *, *, #43951, .F. ) ;
#32776 = EDGE_CURVE ( 'NONE', #25320, #12550, #44563, .T. ) ;
#32777 = CARTESIAN_POINT ( 'NONE',  ( -11.36804826722768524, 24.91136206679766474, -3.000000000000000000 ) ) ;
#32778 = CARTESIAN_POINT ( 'NONE',  ( -15.35561888520754614, 0.000000000000000000, 7.116904623805458741 ) ) ;
#32779 = LINE ( 'NONE', #16043, #11214 ) ;
#32780 = VERTEX_POINT ( 'NONE', #48259 ) ;
#32781 = AXIS2_PLACEMENT_3D ( 'NONE', #39902, #982, #23157 ) ;
#32782 = ADVANCED_FACE ( 'NONE', ( #40321 ), #1418, .F. ) ;
#32783 = VECTOR ( 'NONE', #53617, 999.9999999999998863 ) ;
#32784 = CARTESIAN_POINT ( 'NONE',  ( -10.88912548622250220, 0.000000000000000000, 4.566339419565200508 ) ) ;
#32785 = ORIENTED_EDGE ( 'NONE', *, *, #55382, .T. ) ;
#32786 = EDGE_CURVE ( 'NONE', #47757, #5305, #40874, .T. ) ;
#32787 = ORIENTED_EDGE ( 'NONE', *, *, #26261, .F. ) ;
#32788 = ORIENTED_EDGE ( 'NONE', *, *, #41079, .F. ) ;
#32789 = ORIENTED_EDGE ( 'NONE', *, *, #39150, .T. ) ;
#32790 = VECTOR ( 'NONE', #7760, 999.9999999999998863 ) ;
#32791 = ORIENTED_EDGE ( 'NONE', *, *, #4003, .T. ) ;
#32792 = LINE ( 'NONE', #33087, #26601 ) ;
#32793 = ORIENTED_EDGE ( 'NONE', *, *, #44117, .T. ) ;
#32794 = ORIENTED_EDGE ( 'NONE', *, *, #35122, .T. ) ;
#32795 = FACE_OUTER_BOUND ( 'NONE', #53183, .T. ) ;
#32796 = VERTEX_POINT ( 'NONE', #36086 ) ;
#32797 = ORIENTED_EDGE ( 'NONE', *, *, #46969, .F. ) ;
#32798 = VECTOR ( 'NONE', #6219, 999.9999999999998863 ) ;
#32799 = ORIENTED_EDGE ( 'NONE', *, *, #5427, .T. ) ;
#32800 = CARTESIAN_POINT ( 'NONE',  ( -19.77061338776520216, 21.24370688441071664, -4.270683379717145733 ) ) ;
#32801 = DIRECTION ( 'NONE',  ( -0.005961354470445682716, -0.6427876096865404731, 0.7660212471507180654 ) ) ;
#32802 = DIRECTION ( 'NONE',  ( 0.000000000000000000, -0.000000000000000000, -1.000000000000000000 ) ) ;
#32803 = DIRECTION ( 'NONE',  ( 0.005961354470445682716, -0.6427876096865404731, -0.7660212471507180654 ) ) ;
#32804 = DIRECTION ( 'NONE',  ( -0.5449076811759708816, 0.6444004775717707689, 0.5364919789714475140 ) ) ;
#32805 = ORIENTED_EDGE ( 'NONE', *, *, #41556, .T. ) ;
#32806 = EDGE_LOOP ( 'NONE', ( #50171, #45751, #43008, #25148 ) ) ;
#32807 = CARTESIAN_POINT ( 'NONE',  ( -19.22961988024793101, -0.1191753592594177458, 14.39986392600063603 ) ) ;
#32808 = DIRECTION ( 'NONE',  ( 0.005961354470445682716, -0.6427876096865404731, -0.7660212471507180654 ) ) ;
#32809 = CARTESIAN_POINT ( 'NONE',  ( -29.09713277628012307, 15.85903840484930960, -4.728573048006373014 ) ) ;
#32810 = ADVANCED_FACE ( 'NONE', ( #26695 ), #5142, .F. ) ;
#32811 = CARTESIAN_POINT ( 'NONE',  ( -16.28908438678428183, 0.000000000000000000, 7.648298262822180504 ) ) ;
#32812 = B_SPLINE_CURVE_WITH_KNOTS ( 'NONE', 3,
 ( #43663, #43953, #13025, #26347, #51904, #31486, #48797, #13579, #44252, #4506, #22661, #47946, #9894, #26101, #26941, #4246, #27199, #21559, #26635, #38874, #30646, #30889 ),
 .UNSPECIFIED., .F., .F.,
 ( 4, 2, 2, 2, 2, 2, 2, 2, 2, 2, 4 ),
 ( -5.999998108584347237E-08, 0.0005071597037828261528, 0.001014379407546738259, 0.002028818815074536885, 0.003043258222602335077, 0.004057697630130134570, 0.006086576445185719678, 0.008115455260241304786, 0.01014433407529688989, 0.01217321289035247674, 0.01623097052046364869 ),
 .UNSPECIFIED. ) ;
#32813 = PLANE ( 'NONE',  #21329 ) ;
#32814 = CARTESIAN_POINT ( 'NONE',  ( -19.59569683186026268, 0.000000000000000000, 14.58168106541950948 ) ) ;
#32815 = EDGE_LOOP ( 'NONE', ( #42125, #35682, #16139, #39983 ) ) ;
#32816 = LINE ( 'NONE', #54396, #21105 ) ;
#32817 = EDGE_LOOP ( 'NONE', ( #46075, #16051, #53682, #28888 ) ) ;
#32818 = EDGE_CURVE ( 'NONE', #55170, #48632, #11333, .T. ) ;
#32819 = EDGE_CURVE ( 'NONE', #21126, #7904, #41696, .T. ) ;
#32820 = VECTOR ( 'NONE', #48653, 1000.000000000000000 ) ;
#32821 = VECTOR ( 'NONE', #14804, 1000.000000000000227 ) ;
#32822 = LINE ( 'NONE', #36531, #50087 ) ;
#32823 = LINE ( 'NONE', #24574, #4230 ) ;
#32824 = DIRECTION ( 'NONE',  ( 0.9999697198139515519, 0.000000000000000000, 0.007781995580013368816 ) ) ;
#32825 = FACE_OUTER_BOUND ( 'NONE', #22052, .T. ) ;
#32826 = EDGE_CURVE ( 'NONE', #9089, #19669, #2783, .T. ) ;
#32827 = PLANE ( 'NONE',  #36830 ) ;
#32828 = B_SPLINE_CURVE_WITH_KNOTS ( 'NONE', 3,
 ( #23662, #44409, #39877, #18580 ),
 .UNSPECIFIED., .F., .F.,
 ( 4, 4 ),
 ( 0.3889078242859423939, 0.4131271774438034505 ),
 .UNSPECIFIED. ) ;
#32829 = AXIS2_PLACEMENT_3D ( 'NONE', #638, #17961, #13961 ) ;
#32830 = ORIENTED_EDGE ( 'NONE', *, *, #26362, .T. ) ;
#32831 = LINE ( 'NONE', #50147, #40258 ) ;
#32832 = DIRECTION ( 'NONE',  ( 0.005002170337468016433, -0.7660444431189770143, -0.6427681459581293666 ) ) ;
#32833 = DIRECTION ( 'NONE',  ( -0.005002170337468016433, -0.7660444431189770143, 0.6427681459581293666 ) ) ;
#32834 = CARTESIAN_POINT ( 'NONE',  ( -19.56442468080716068, -2.784623065533158304, 8.851459539246230079 ) ) ;
#32835 = AXIS2_PLACEMENT_3D ( 'NONE', #5635, #14454, #43684 ) ;
#32836 = FACE_OUTER_BOUND ( 'NONE', #12211, .T. ) ;
#32837 = FACE_OUTER_BOUND ( 'NONE', #6345, .T. ) ;
#32838 = DIRECTION ( 'NONE',  ( -0.6427681459581293666, -0.7660444431189770143, -0.005002170337467561935 ) ) ;
#32839 = ADVANCED_FACE ( 'NONE', ( #46512 ), #42283, .T. ) ;
#32840 = DIRECTION ( 'NONE',  ( 0.7660212471507180654, -0.6427876096865404731, 0.005961354470445141482 ) ) ;
#32841 = LINE ( 'NONE', #54415, #22908 ) ;
#32842 = ORIENTED_EDGE ( 'NONE', *, *, #3228, .F. ) ;
#32843 = ORIENTED_EDGE ( 'NONE', *, *, #29741, .F. ) ;
#32844 = EDGE_CURVE ( 'NONE', #33164, #40367, #7630, .T. ) ;
#32845 = VECTOR ( 'NONE', #27057, 1000.000000000000227 ) ;
#32846 = ADVANCED_FACE ( 'NONE', ( #15053 ), #24655, .F. ) ;
#32847 = ORIENTED_EDGE ( 'NONE', *, *, #41715, .F. ) ;
#32848 = ORIENTED_EDGE ( 'NONE', *, *, #47892, .T. ) ;
#32849 = ORIENTED_EDGE ( 'NONE', *, *, #31546, .T. ) ;
#32850 = ADVANCED_FACE ( 'NONE', ( #2245 ), #15868, .F. ) ;
#32851 = ORIENTED_EDGE ( 'NONE', *, *, #6358, .F. ) ;
#32852 = AXIS2_PLACEMENT_3D ( 'NONE', #13479, #30795, #48094 ) ;
#32853 = CARTESIAN_POINT ( 'NONE',  ( 2.072287782118878319, 0.000000000000000000, -2.950529333540147015 ) ) ;
#32854 = CARTESIAN_POINT ( 'NONE',  ( -10.43311074989726173, 0.000000000000000000, 5.677884441106503033 ) ) ;
#32855 = ADVANCED_FACE ( 'NONE', ( #55070 ), #41975, .F. ) ;
#32856 = CARTESIAN_POINT ( 'NONE',  ( -16.96101973371472837, 0.000000000000000000, 8.581739302416485415 ) ) ;
#32857 = AXIS2_PLACEMENT_3D ( 'NONE', #12736, #16713, #21250 ) ;
#32858 = VECTOR ( 'NONE', #55956, 999.9999999999998863 ) ;
#32859 = ORIENTED_EDGE ( 'NONE', *, *, #32690, .T. ) ;
#32860 = CARTESIAN_POINT ( 'NONE',  ( -19.86019089980205266, 1.257817950434005461, 6.659987261600974762 ) ) ;
#32861 = EDGE_CURVE ( 'NONE', #49508, #42567, #37171, .T. ) ;
#32862 = VERTEX_POINT ( 'NONE', #33479 ) ;
#32863 = EDGE_LOOP ( 'NONE', ( #32184, #18971, #12745, #20755 ) ) ;
#32864 = VECTOR ( 'NONE', #37116, 999.9999999999998863 ) ;
#32865 = AXIS2_PLACEMENT_3D ( 'NONE', #35707, #30626, #9026 ) ;
#32866 = CARTESIAN_POINT ( 'NONE',  ( -66.39500965126839560, -9.308393707792198768, 5.887047890946016437 ) ) ;
#32867 = CARTESIAN_POINT ( 'NONE',  ( -7.860905869600908424, 1.712176620043476140E-14, -3.600000000000000089 ) ) ;
#32868 = PLANE ( 'NONE',  #10561 ) ;
#32869 = EDGE_LOOP ( 'NONE', ( #38412, #41484, #10692, #20114 ) ) ;
#32870 = LINE ( 'NONE', #11005, #28298 ) ;
#32871 = ORIENTED_EDGE ( 'NONE', *, *, #19102, .T. ) ;
#32872 = CARTESIAN_POINT ( 'NONE',  ( -13.22512383883834097, 0.000000000000000000, 6.194814433051186064 ) ) ;
#32873 = VECTOR ( 'NONE', #8369, 999.9999999999998863 ) ;
#32874 = CARTESIAN_POINT ( 'NONE',  ( -17.74560456716937296, 0.000000000000000000, 3.774316574337878372 ) ) ;
#32875 = CARTESIAN_POINT ( 'NONE',  ( -23.33771345073609638, -0.1191753592594197858, 5.846786880686956955 ) ) ;
#32876 = DIRECTION ( 'NONE',  ( 0.007781995580012663651, 0.000000000000000000, -0.9999697198139515519 ) ) ;
#32877 = CARTESIAN_POINT ( 'NONE',  ( -11.91804826722769306, 25.86399001096056338, 4.999999999999888978 ) ) ;
#32878 = DIRECTION ( 'NONE',  ( -0.9999697198139514409, -0.000000000000000000, -0.007781995580013368816 ) ) ;
#32879 = CARTESIAN_POINT ( 'NONE',  ( -21.70540433349056642, -3.108426967578157729, 10.21450611222444316 ) ) ;
#32880 = DIRECTION ( 'NONE',  ( -0.005002170337468016433, -0.7660444431189770143, 0.6427681459581293666 ) ) ;
#32881 = LINE ( 'NONE', #2216, #256 ) ;
#32882 = VERTEX_POINT ( 'NONE', #54471 ) ;
#32883 = DIRECTION ( 'NONE',  ( -2.551063935260010306E-17, 4.081702296416016490E-16, -1.000000000000000000 ) ) ;
#32884 = EDGE_LOOP ( 'NONE', ( #14242, #27095, #42772, #5625 ) ) ;
#32885 = ADVANCED_FACE ( 'NONE', ( #45986 ), #50525, .F. ) ;
#32886 = DIRECTION ( 'NONE',  ( 0.007781995580012662783, 0.000000000000000000, -0.9999697198139514409 ) ) ;
#32887 = CARTESIAN_POINT ( 'NONE',  ( -17.42344502812375140, -2.460819163488158878, 7.488412966268020554 ) ) ;
#32888 = PLANE ( 'NONE',  #27777 ) ;
#32889 = AXIS2_PLACEMENT_3D ( 'NONE', #21871, #13382, #34648 ) ;
#32890 = CARTESIAN_POINT ( 'NONE',  ( -20.55929158756503128, 0.4483081953215033444, 4.653555402000536745 ) ) ;
#32891 = FACE_OUTER_BOUND ( 'NONE', #40284, .T. ) ;
#32892 = ADVANCED_FACE ( 'NONE', ( #11875 ), #36624, .F. ) ;
#32893 = ADVANCED_FACE ( 'NONE', ( #37440 ), #28941, .F. ) ;
#32894 = LINE ( 'NONE', #7330, #34778 ) ;
#32895 = ORIENTED_EDGE ( 'NONE', *, *, #42407, .F. ) ;
#32896 = CARTESIAN_POINT ( 'NONE',  ( -10.62894072970072301, -10.24364977037474667, 0.9102679640985203990 ) ) ;
#32897 = AXIS2_PLACEMENT_3D ( 'NONE', #49415, #19029, #18776 ) ;
#32898 = DIRECTION ( 'NONE',  ( 0.000000000000000000, 1.000000000000000000, 0.000000000000000000 ) ) ;
#32899 = DIRECTION ( 'NONE',  ( -0.005961354470445682716, -0.6427876096865404731, 0.7660212471507180654 ) ) ;
#32900 = DIRECTION ( 'NONE',  ( 0.000000000000000000, 0.000000000000000000, 1.000000000000000000 ) ) ;
#32901 = CARTESIAN_POINT ( 'NONE',  ( -17.69736534483395118, 0.000000000000000000, 9.483999043806973006 ) ) ;
#32902 = AXIS2_PLACEMENT_3D ( 'NONE', #26450, #35283, #52579 ) ;
#32903 = AXIS2_PLACEMENT_3D ( 'NONE', #1621, #53844, #49314 ) ;
#32904 = LINE ( 'NONE', #37168, #43642 ) ;
#32905 = PLANE ( 'NONE',  #31176 ) ;
#32906 = DIRECTION ( 'NONE',  ( 0.7660212471507180654, -0.6427876096865404731, 0.005961354470445141482 ) ) ;
#32907 = CARTESIAN_POINT ( 'NONE',  ( -10.29499555079022066, -0.1191753592594194527, 0.7805523157836706805 ) ) ;
#32908 = EDGE_CURVE ( 'NONE', #17489, #17469, #7340, .T. ) ;
#32909 = ORIENTED_EDGE ( 'NONE', *, *, #13463, .T. ) ;
#32910 = AXIS2_PLACEMENT_3D ( 'NONE', #41322, #20838, #55472 ) ;
#32911 = CARTESIAN_POINT ( 'NONE',  ( 0.3240706152708105470, -3.670543518250628079, -2.125000000000001332 ) ) ;
#32912 = VECTOR ( 'NONE', #47428, 1000.000000000000114 ) ;
#32913 = ORIENTED_EDGE ( 'NONE', *, *, #50231, .T. ) ;
#32914 = CARTESIAN_POINT ( 'NONE',  ( -19.45503627000849889, 0.000000000000000000, 7.556996783084074742 ) ) ;
#32915 = LINE ( 'NONE', #1199, #46423 ) ;
#32916 = ORIENTED_EDGE ( 'NONE', *, *, #2237, .T. ) ;
#32917 = VECTOR ( 'NONE', #25227, 1000.000000000000227 ) ;
#32918 = ORIENTED_EDGE ( 'NONE', *, *, #831, .T. ) ;
#32919 = LINE ( 'NONE', #8993, #5704 ) ;
#32920 = VECTOR ( 'NONE', #52989, 1000.000000000000114 ) ;
#32921 = EDGE_CURVE ( 'NONE', #1131, #54123, #45401, .T. ) ;
#32922 = ORIENTED_EDGE ( 'NONE', *, *, #12913, .F. ) ;
#32923 = ORIENTED_EDGE ( 'NONE', *, *, #28331, .T. ) ;
#32924 = EDGE_LOOP ( 'NONE', ( #3720, #29092, #2849, #29752 ) ) ;
#32925 = DIRECTION ( 'NONE',  ( 0.6427681459581294776, -0.7660444431189769032, 0.005002170337467562802 ) ) ;
#32926 = CARTESIAN_POINT ( 'NONE',  ( -65.11529574170205592, -9.161643534026593372, -1.301894315629610555 ) ) ;
#32927 = APPLICATION_CONTEXT ( 'automotive_design' ) ;
#32928 = DIRECTION ( 'NONE',  ( 0.7660212471507180654, -0.6427876096865404731, 0.005961354470445141482 ) ) ;
#32929 = CIRCLE ( 'NONE', #12091, 1.000000000000000444 ) ;
#32930 = ORIENTED_EDGE ( 'NONE', *, *, #53313, .T. ) ;
#32931 = ADVANCED_FACE ( 'NONE', ( #41153 ), #19584, .F. ) ;
#32932 = ORIENTED_EDGE ( 'NONE', *, *, #13222, .T. ) ;
#32933 = AXIS2_PLACEMENT_3D ( 'NONE', #48005, #47441, #9105 ) ;
#32934 = DIRECTION ( 'NONE',  ( 0.000000000000000000, -0.000000000000000000, -1.000000000000000000 ) ) ;
#32935 = CARTESIAN_POINT ( 'NONE',  ( -19.32961685222932147, 0.000000000000000000, 14.39908572644263351 ) ) ;
#32936 = ORIENTED_EDGE ( 'NONE', *, *, #15013, .F. ) ;
#32937 = VECTOR ( 'NONE', #16579, 999.9999999999998863 ) ;
#32938 = LINE ( 'NONE', #50253, #30970 ) ;
#32939 = VERTEX_POINT ( 'NONE', #209 ) ;
#32940 = CARTESIAN_POINT ( 'NONE',  ( -50.99228148001754590, 2.341865487272627000, -5.000000000000000000 ) ) ;
#32941 = DIRECTION ( 'NONE',  ( -0.005002170337468016433, -0.7660444431189770143, 0.6427681459581293666 ) ) ;
#32942 = ADVANCED_FACE ( 'NONE', ( #29505 ), #55909, .F. ) ;
#32943 = AXIS2_PLACEMENT_3D ( 'NONE', #6922, #28192, #24236 ) ;
#32944 = VECTOR ( 'NONE', #52105, 999.9999999999998863 ) ;
#32945 = ORIENTED_EDGE ( 'NONE', *, *, #42906, .F. ) ;
#32946 = CARTESIAN_POINT ( 'NONE',  ( -20.44552454186363022, -3.270328918600659218, 9.990834699409186115 ) ) ;
#32947 = EDGE_CURVE ( 'NONE', #47757, #21366, #34328, .T. ) ;
#32948 = ADVANCED_FACE ( 'NONE', ( #42820 ), #34045, .F. ) ;
#32949 = VECTOR ( 'NONE', #30135, 999.9999999999998863 ) ;
#32950 = CARTESIAN_POINT ( 'NONE',  ( -18.14056621274878012, 0.000000000000000000, 6.725899449939636732 ) ) ;
#32951 = VECTOR ( 'NONE', #5902, 1000.000000000000227 ) ;
#32952 = ORIENTED_EDGE ( 'NONE', *, *, #30329, .F. ) ;
#32953 = FACE_OUTER_BOUND ( 'NONE', #4062, .T. ) ;
#32954 = CARTESIAN_POINT ( 'NONE',  ( -16.37548929079726534, -0.1191753592594192307, 5.900968518956748454 ) ) ;
#32955 = LINE ( 'NONE', #15355, #28316 ) ;
#32956 = EDGE_CURVE ( 'NONE', #9006, #14383, #55605, .T. ) ;
#32957 = ORIENTED_EDGE ( 'NONE', *, *, #35407, .T. ) ;
#32958 = ADVANCED_FACE ( 'NONE', ( #56179 ), #47362, .F. ) ;
#32959 = DIRECTION ( 'NONE',  ( -0.005961354470445682716, -0.6427876096865404731, 0.7660212471507180654 ) ) ;
#32960 = DIRECTION ( 'NONE',  ( 0.9999697198139515519, 0.000000000000000000, 0.007781995580013368816 ) ) ;
#32961 = LINE ( 'NONE', #37801, #46670 ) ;
#32962 = CARTESIAN_POINT ( 'NONE',  ( -19.68560291375552040, -0.03739765774599557863, 4.466501887183837560 ) ) ;
#32963 = CARTESIAN_POINT ( 'NONE',  ( -14.90567268141948531, 0.000000000000000000, 9.008243043902110614 ) ) ;
#32964 = EDGE_CURVE ( 'NONE', #13331, #42326, #26098, .T. ) ;
#32965 = DIRECTION ( 'NONE',  ( -0.005961354470445682716, -0.6427876096865404731, 0.7660212471507180654 ) ) ;
#32966 = DIRECTION ( 'NONE',  ( -0.7660212471507179544, -0.6427876096865405842, -0.005961354470445141482 ) ) ;
#32967 = AXIS2_PLACEMENT_3D ( 'NONE', #18854, #36174, #49509 ) ;
#32968 = VERTEX_POINT ( 'NONE', #12735 ) ;
#32969 = DIRECTION ( 'NONE',  ( 0.9999697198139515519, 0.000000000000000000, 0.007781995580013368816 ) ) ;
#32970 = CARTESIAN_POINT ( 'NONE',  ( -67.30955648132578517, -0.6009093778043306244, 2.715629364103489873 ) ) ;
#32971 = ORIENTED_EDGE ( 'NONE', *, *, #34420, .F. ) ;
#32972 = FACE_OUTER_BOUND ( 'NONE', #51535, .T. ) ;
#32973 = DIRECTION ( 'NONE',  ( -0.9321478471874540261, 0.000000000000000000, 0.3620778797217457656 ) ) ;
#32974 = AXIS2_PLACEMENT_3D ( 'NONE', #31512, #1381, #5379 ) ;
#32975 = ADVANCED_FACE ( 'NONE', ( #8476 ), #51369, .F. ) ;
#32976 = CARTESIAN_POINT ( 'NONE',  ( -50.02554558092695913, 3.776013638374817294, 5.000000000000000000 ) ) ;
#32977 = AXIS2_PLACEMENT_3D ( 'NONE', #41720, #38040, #2811 ) ;
#32978 = CARTESIAN_POINT ( 'NONE',  ( -13.56079194166738944, 2.067327705546507133, 5.541630197524685997 ) ) ;
#32979 = CARTESIAN_POINT ( 'NONE',  ( -56.47915852223218280, 6.634043282999704694, 2.292377755077263934 ) ) ;
#32980 = EDGE_CURVE ( 'NONE', #21349, #49949, #4240, .T. ) ;
#32981 = ORIENTED_EDGE ( 'NONE', *, *, #29286, .T. ) ;
#32982 = EDGE_LOOP ( 'NONE', ( #8563, #2485, #34800, #48358 ) ) ;
#32983 = LINE ( 'NONE', #11946, #12306 ) ;
#32984 = VECTOR ( 'NONE', #15457, 1000.000000000000000 ) ;
#32985 = AXIS2_PLACEMENT_3D ( 'NONE', #22442, #26671, #49085 ) ;
#32986 = PLANE ( 'NONE',  #51085 ) ;
#32987 = DIRECTION ( 'NONE',  ( 0.007781995580012663651, 0.000000000000000000, -0.9999697198139515519 ) ) ;
#32988 = ORIENTED_EDGE ( 'NONE', *, *, #32751, .F. ) ;
#32989 = DIRECTION ( 'NONE',  ( -0.005002170337468016433, -0.7660444431189770143, 0.6427681459581293666 ) ) ;
#32990 = VERTEX_POINT ( 'NONE', #34886 ) ;
#32991 = CARTESIAN_POINT ( 'NONE',  ( 3.520599301005862269, -1.000000000000000000, 0.7780620552096689790 ) ) ;
#32992 = AXIS2_PLACEMENT_3D ( 'NONE', #52985, #51648, #12492 ) ;
#32993 = ORIENTED_EDGE ( 'NONE', *, *, #2846, .F. ) ;
#32994 = AXIS2_PLACEMENT_3D ( 'NONE', #21745, #4437, #25719 ) ;
#32995 = VERTEX_POINT ( 'NONE', #21555 ) ;
#32996 = CARTESIAN_POINT ( 'NONE',  ( -16.45902014130496482, 0.000000000000000000, 3.784329071833556046 ) ) ;
#32997 = CARTESIAN_POINT ( 'NONE',  ( -18.77489909422165582, 2.714935509636507316, 8.629801223202855809 ) ) ;
#32998 = CARTESIAN_POINT ( 'NONE',  ( -29.86197018149027116, 0.000000000000000000, 8.281335066757780083 ) ) ;
#32999 = ORIENTED_EDGE ( 'NONE', *, *, #40581, .T. ) ;
#33000 = EDGE_CURVE ( 'NONE', #32426, #46062, #8196, .T. ) ;
#33001 = ORIENTED_EDGE ( 'NONE', *, *, #40515, .T. ) ;
#33002 = ORIENTED_EDGE ( 'NONE', *, *, #38249, .F. ) ;
#33003 = VERTEX_POINT ( 'NONE', #51633 ) ;
#33004 = PLANE ( 'NONE',  #55820 ) ;
#33005 = VECTOR ( 'NONE', #303, 999.9999999999998863 ) ;
#33006 = FACE_OUTER_BOUND ( 'NONE', #37362, .T. ) ;
#33007 = ORIENTED_EDGE ( 'NONE', *, *, #1711, .F. ) ;
#33008 = CARTESIAN_POINT ( 'NONE',  ( -11.20636620717317378, 0.000000000000000000, 11.32298014792380414 ) ) ;
#33009 = VERTEX_POINT ( 'NONE', #25505 ) ;
#33010 = AXIS2_PLACEMENT_3D ( 'NONE', #44411, #5261, #23410 ) ;
#33011 = DIRECTION ( 'NONE',  ( 0.2426528472758541499, 0.7422098413412800966, 0.6246952433987894571 ) ) ;
#33012 = LINE ( 'NONE', #50331, #45829 ) ;
#33013 = EDGE_CURVE ( 'NONE', #3665, #35650, #52205, .T. ) ;
#33014 = ORIENTED_EDGE ( 'NONE', *, *, #26433, .F. ) ;
#33015 = DIRECTION ( 'NONE',  ( -0.02128905125521658726, -0.002441305003917799629, -0.9997703818010066357 ) ) ;
#33016 = VECTOR ( 'NONE', #33386, 1000.000000000000227 ) ;
#33017 = ORIENTED_EDGE ( 'NONE', *, *, #8016, .F. ) ;
#33018 = EDGE_CURVE ( 'NONE', #3168, #10121, #3384, .T. ) ;
#33019 = CARTESIAN_POINT ( 'NONE',  ( -23.33771345073609638, -0.1191753592594197858, 5.846786880686956955 ) ) ;
#33020 = LINE ( 'NONE', #6623, #47440 ) ;
#33021 = DIRECTION ( 'NONE',  ( -0.5449076811759708816, 0.6444004775717707689, 0.5364919789714475140 ) ) ;
#33022 = LINE ( 'NONE', #54574, #51991 ) ;
#33023 = CARTESIAN_POINT ( 'NONE',  ( -9.756139500593079106, -1.014955843830462667, 1.876821366356609344 ) ) ;
#33024 = AXIS2_PLACEMENT_3D ( 'NONE', #52553, #5426, #5162 ) ;
#33025 = DIRECTION ( 'NONE',  ( 0.000000000000000000, -1.000000000000000000, 0.000000000000000000 ) ) ;
#33026 = EDGE_LOOP ( 'NONE', ( #16568, #4266, #6838, #16814 ) ) ;
#33027 = VECTOR ( 'NONE', #24786, 1000.000000000000227 ) ;
#33028 = EDGE_LOOP ( 'NONE', ( #35886, #17043, #1389 ) ) ;
#33029 = ADVANCED_FACE ( 'NONE', ( #29794 ), #21810, .F. ) ;
#33030 = PLANE ( 'NONE',  #47298 ) ;
#33031 = DIRECTION ( 'NONE',  ( 0.7660212471507180654, -0.6427876096865404731, 0.005961354470445141482 ) ) ;
#33032 = CARTESIAN_POINT ( 'NONE',  ( -30.79567442779373110, 0.000000000000000000, 8.843406890442315316 ) ) ;
#33033 = DIRECTION ( 'NONE',  ( -0.5364919789714478471, 0.6444004775717705469, -0.5449076811759709926 ) ) ;
#33034 = EDGE_CURVE ( 'NONE', #1901, #722, #33740, .T. ) ;
#33035 = CARTESIAN_POINT ( 'NONE',  ( -16.42896195337263521, 3.848249166794011522, 2.940719187860218575 ) ) ;
#33036 = VECTOR ( 'NONE', #1343, 999.9999999999998863 ) ;
#33037 = AXIS2_PLACEMENT_3D ( 'NONE', #8480, #38583, #47365 ) ;
#33038 = DIRECTION ( 'NONE',  ( 0.005002170337468016433, -0.7660444431189770143, -0.6427681459581293666 ) ) ;
#33039 = EDGE_LOOP ( 'NONE', ( #31002, #8029, #5286, #28215 ) ) ;
#33040 = FACE_OUTER_BOUND ( 'NONE', #34490, .T. ) ;
#33041 = CARTESIAN_POINT ( 'NONE',  ( -62.23823698199103660, 6.658783344088820222, 3.000000000000000000 ) ) ;
#33042 = VERTEX_POINT ( 'NONE', #9041 ) ;
#33043 = LINE ( 'NONE', #10899, #9352 ) ;
#33044 = DIRECTION ( 'NONE',  ( 0.007781995580012663651, -3.146120232559066537E-19, -0.9999697198139514409 ) ) ;
#33045 = ORIENTED_EDGE ( 'NONE', *, *, #38789, .T. ) ;
#33046 = EDGE_CURVE ( 'NONE', #44540, #33054, #26344, .T. ) ;
#33047 = CARTESIAN_POINT ( 'NONE',  ( -14.93495759592298988, 0.000000000000000000, 12.77129166681078409 ) ) ;
#33048 = FACE_OUTER_BOUND ( 'NONE', #42861, .T. ) ;
#33049 = LINE ( 'NONE', #18891, #527 ) ;
#33050 = CARTESIAN_POINT ( 'NONE',  ( -16.03174594003255038, 0.000000000000000000, 8.588971125952504337 ) ) ;
#33051 = DIRECTION ( 'NONE',  ( 0.007781995580012663651, 0.000000000000000000, -0.9999697198139515519 ) ) ;
#33052 = VECTOR ( 'NONE', #28845, 1000.000000000000227 ) ;
#33053 = EDGE_CURVE ( 'NONE', #28751, #3861, #55324, .T. ) ;
#33054 = VERTEX_POINT ( 'NONE', #7937 ) ;
#33055 = ORIENTED_EDGE ( 'NONE', *, *, #1104, .T. ) ;
#33056 = VECTOR ( 'NONE', #16518, 999.9999999999998863 ) ;
#33057 = CARTESIAN_POINT ( 'NONE',  ( -20.84338673312048940, 0.7721120973665037690, 6.244767860881510479 ) ) ;
#33058 = CARTESIAN_POINT ( 'NONE',  ( 5.551076415483179538, -1.058033566259081848, 2.420903282225134401 ) ) ;
#33059 = LINE ( 'NONE', #41576, #17922 ) ;
#33060 = VECTOR ( 'NONE', #48835, 999.9999999999998863 ) ;
#33061 = CARTESIAN_POINT ( 'NONE',  ( -10.29784693629447467, -0.1191753592594200495, 1.146949229589934616 ) ) ;
#33062 = CARTESIAN_POINT ( 'NONE',  ( -18.35780447774326518, 0.000000000000000000, 8.940201270370220499 ) ) ;
#33063 = CARTESIAN_POINT ( 'NONE',  ( -18.88442267121436302, -0.3560938001956556742, 4.205310943792594180 ) ) ;
#33064 = VERTEX_POINT ( 'NONE', #25248 ) ;
#33065 = FACE_OUTER_BOUND ( 'NONE', #38595, .T. ) ;
#33066 = CARTESIAN_POINT ( 'NONE',  ( -21.08970118930990978, 3.848249166794010634, 4.751108586468945738 ) ) ;
#33067 = LINE ( 'NONE', #50391, #50495 ) ;
#33069 = EDGE_LOOP ( 'NONE', ( #33318, #21394, #33430, #1143 ) ) ;
#33068 = VECTOR ( 'NONE', #22300, 1000.000000000000114 ) ;
#33070 = AXIS2_PLACEMENT_3D ( 'NONE', #7956, #55623, #33234 ) ;
#33071 = CARTESIAN_POINT ( 'NONE',  ( -69.37797197704281871, -10.07236156554400353, 7.501241569353456207 ) ) ;
#33072 = FACE_OUTER_BOUND ( 'NONE', #50750, .T. ) ;
#33073 = CARTESIAN_POINT ( 'NONE',  ( -13.27065584551087163, 0.000000000000000000, 12.04557950825129176 ) ) ;
#33074 = VECTOR ( 'NONE', #16005, 1000.000000000000114 ) ;
#33075 = ORIENTED_EDGE ( 'NONE', *, *, #40018, .T. ) ;
#33076 = DIRECTION ( 'NONE',  ( 0.5449076811759707706, 0.6444004775717708799, -0.5364919789714476250 ) ) ;
#33077 = ADVANCED_FACE ( 'NONE', ( #32766 ), #5610, .F. ) ;
#33078 = ORIENTED_EDGE ( 'NONE', *, *, #41555, .T. ) ;
#33079 = AXIS2_PLACEMENT_3D ( 'NONE', #8631, #17406, #18244 ) ;
#33080 = VERTEX_POINT ( 'NONE', #13577 ) ;
#33081 = VERTEX_POINT ( 'NONE', #15445 ) ;
#33082 = VECTOR ( 'NONE', #6802, 999.9999999999998863 ) ;
#33083 = EDGE_CURVE ( 'NONE', #3168, #31521, #40255, .T. ) ;
#33084 = ORIENTED_EDGE ( 'NONE', *, *, #12599, .F. ) ;
#33085 = ADVANCED_FACE ( 'NONE', ( #44501 ), #35724, .F. ) ;
#33086 = ORIENTED_EDGE ( 'NONE', *, *, #7779, .F. ) ;
#33087 = CARTESIAN_POINT ( 'NONE',  ( -17.74560456716937296, 0.000000000000000000, 3.774316574337878372 ) ) ;
#33089 = ADVANCED_FACE ( 'NONE', ( #9616 ), #35186, .F. ) ;
#33088 = ORIENTED_EDGE ( 'NONE', *, *, #38050, .F. ) ;
#33090 = EDGE_CURVE ( 'NONE', #6826, #48632, #43658, .T. ) ;
#33091 = EDGE_CURVE ( 'NONE', #32088, #14924, #14157, .T. ) ;
#33092 = ORIENTED_EDGE ( 'NONE', *, *, #34491, .F. ) ;
#33093 = DIRECTION ( 'NONE',  ( 0.7660212471507180654, -0.6427876096865404731, 0.005961354470445141482 ) ) ;
#33094 = EDGE_LOOP ( 'NONE', ( #20, #14702, #21727, #13875 ) ) ;
#33095 = VERTEX_POINT ( 'NONE', #22934 ) ;
#33096 = VECTOR ( 'NONE', #29497, 999.9999999999998863 ) ;
#33097 = CARTESIAN_POINT ( 'NONE',  ( -20.06177075545399191, 0.000000000000000000, 14.76272000528038220 ) ) ;
#33098 = VECTOR ( 'NONE', #42516, 999.9999999999998863 ) ;
#33099 = LINE ( 'NONE', #24851, #22148 ) ;
#33100 = DIRECTION ( 'NONE',  ( 0.9999697198139515519, 0.000000000000000000, 0.007781995580013368816 ) ) ;
#33101 = DIRECTION ( 'NONE',  ( 0.5364919789714477361, 0.6444004775717706579, 0.5449076811759711036 ) ) ;
#33102 = ORIENTED_EDGE ( 'NONE', *, *, #52495, .T. ) ;
#33103 = CARTESIAN_POINT ( 'NONE',  ( -17.39384106964635990, -5.698858183938163791, 12.79108746244999395 ) ) ;
#33104 = CIRCLE ( 'NONE', #12263, 0.5000000000000004441 ) ;
#33105 = ORIENTED_EDGE ( 'NONE', *, *, #55058, .F. ) ;
#33106 = ORIENTED_EDGE ( 'NONE', *, *, #19595, .F. ) ;
#33107 = EDGE_CURVE ( 'NONE', #10405, #51867, #18690, .T. ) ;
#33108 = DIRECTION ( 'NONE',  ( -0.5364919789714478471, 0.6444004775717705469, -0.5449076811759709926 ) ) ;
#33109 = DIRECTION ( 'NONE',  ( -0.6427681459581293666, -0.7660444431189770143, -0.005002170337467561935 ) ) ;
#33110 = VECTOR ( 'NONE', #44342, 999.9999999999998863 ) ;
#33111 = EDGE_CURVE ( 'NONE', #50858, #21631, #18112, .T. ) ;
#33112 = LINE ( 'NONE', #50431, #28784 ) ;
#33113 = VECTOR ( 'NONE', #22274, 999.9999999999998863 ) ;
#33114 = AXIS2_PLACEMENT_3D ( 'NONE', #12307, #42108, #50356 ) ;
#33115 = CARTESIAN_POINT ( 'NONE',  ( -10.00813838035478298, 0.000000000000000000, 10.77830692922518452 ) ) ;
#33116 = EDGE_CURVE ( 'NONE', #44540, #41193, #39969, .T. ) ;
#33117 = AXIS2_PLACEMENT_3D ( 'NONE', #46999, #48100, #13202 ) ;
#33118 = DIRECTION ( 'NONE',  ( 0.9999697198139515519, 0.000000000000000000, 0.007781995580013368816 ) ) ;
#33119 = CARTESIAN_POINT ( 'NONE',  ( -12.10735231521451283, 0.000000000000000000, 7.680841468734264765 ) ) ;
#33120 = VERTEX_POINT ( 'NONE', #28231 ) ;
#33121 = CARTESIAN_POINT ( 'NONE',  ( -14.89960414888230744, 0.000000000000000000, 8.228449645346760377 ) ) ;
#33122 = EDGE_LOOP ( 'NONE', ( #12484, #49737, #55613, #11133 ) ) ;
#33123 = VECTOR ( 'NONE', #28987, 1000.000000000000000 ) ;
#33124 = ADVANCED_FACE ( 'NONE', ( #39426 ), #30887, .F. ) ;
#33125 = LINE ( 'NONE', #24037, #25612 ) ;
#33126 = LINE ( 'NONE', #45899, #35981 ) ;
#33127 = CARTESIAN_POINT ( 'NONE',  ( -9.439064187057317312, -1.805665653504137769, 2.693112798287724541 ) ) ;
#33128 = DIRECTION ( 'NONE',  ( 0.005002170337468016433, -0.7660444431189770143, -0.6427681459581293666 ) ) ;
#33129 = DIRECTION ( 'NONE',  ( -0.5364919789714478471, 0.6444004775717705469, -0.5449076811759709926 ) ) ;
#33130 = VECTOR ( 'NONE', #15648, 999.9999999999998863 ) ;
#33131 = ORIENTED_EDGE ( 'NONE', *, *, #5244, .F. ) ;
#33132 = VECTOR ( 'NONE', #30546, 999.9999999999998863 ) ;
#33133 = EDGE_LOOP ( 'NONE', ( #17212, #38387, #1766, #567 ) ) ;
#33134 = CARTESIAN_POINT ( 'NONE',  ( -19.45503627000849889, 0.000000000000000000, 7.556996783084074742 ) ) ;
#33135 = CARTESIAN_POINT ( 'NONE',  ( -15.88130887279446490, 0.000000000000000000, 3.050160814894388839 ) ) ;
#33136 = DIRECTION ( 'NONE',  ( 0.9999697198139515519, 0.000000000000000000, 0.007781995580013368816 ) ) ;
#33137 = CARTESIAN_POINT ( 'NONE',  ( -10.27421835998572064, 0.000000000000000000, 10.96090226820206048 ) ) ;
#33138 = CARTESIAN_POINT ( 'NONE',  ( -9.754109641566973465, 0.000000000000000000, 3.836508235701692637 ) ) ;
#33139 = CARTESIAN_POINT ( 'NONE',  ( -13.17065887352947762, -0.1191753592594197858, 12.04635770780929427 ) ) ;
#33140 = DIRECTION ( 'NONE',  ( 0.5449076811759707706, 0.6444004775717708799, -0.5364919789714476250 ) ) ;
#33141 = AXIS2_PLACEMENT_3D ( 'NONE', #29668, #11188, #12329 ) ;
#33142 = DIRECTION ( 'NONE',  ( 0.9999697198139515519, 0.000000000000000000, 0.007781995580013368816 ) ) ;
#33143 = VECTOR ( 'NONE', #52082, 1000.000000000000227 ) ;
#33144 = CARTESIAN_POINT ( 'NONE',  ( -14.51119359642235374, -0.1191753592594179401, 5.176812759513254036 ) ) ;
#33145 = VECTOR ( 'NONE', #40540, 1000.000000000000227 ) ;
#33146 = ORIENTED_EDGE ( 'NONE', *, *, #21144, .T. ) ;
#33147 = VECTOR ( 'NONE', #4747, 999.9999999999998863 ) ;
#33148 = VERTEX_POINT ( 'NONE', #53039 ) ;
#33149 = ORIENTED_EDGE ( 'NONE', *, *, #18824, .T. ) ;
#33150 = VECTOR ( 'NONE', #36956, 1000.000000000000114 ) ;
#33151 = VECTOR ( 'NONE', #54044, 1000.000000000000227 ) ;
#33152 = ORIENTED_EDGE ( 'NONE', *, *, #12877, .F. ) ;
#33153 = ORIENTED_EDGE ( 'NONE', *, *, #37235, .F. ) ;
#33154 = DIRECTION ( 'NONE',  ( -0.9999697198139514409, -0.000000000000000000, -0.007781995580013368816 ) ) ;
#33155 = CARTESIAN_POINT ( 'NONE',  ( -18.66354898467281132, 0.000000000000000000, 14.21960318569776582 ) ) ;
#33156 = DIRECTION ( 'NONE',  ( 0.007781995580012662783, 0.000000000000000000, -0.9999697198139514409 ) ) ;
#33157 = VECTOR ( 'NONE', #14141, 1000.000000000000227 ) ;
#33158 = EDGE_CURVE ( 'NONE', #370, #51735, #54351, .T. ) ;
#33159 = EDGE_CURVE ( 'NONE', #36173, #35938, #5073, .T. ) ;
#33160 = VECTOR ( 'NONE', #8222, 999.9999999999998863 ) ;
#33161 = VERTEX_POINT ( 'NONE', #19725 ) ;
#33162 = DIRECTION ( 'NONE',  ( -0.005961354470445682716, -0.6427876096865404731, 0.7660212471507180654 ) ) ;
#33163 = VECTOR ( 'NONE', #28513, 999.9999999999998863 ) ;
#33164 = VERTEX_POINT ( 'NONE', #37051 ) ;
#33165 = LINE ( 'NONE', #50482, #51267 ) ;
#33166 = EDGE_CURVE ( 'NONE', #53467, #6270, #18383, .T. ) ;
#33167 = ORIENTED_EDGE ( 'NONE', *, *, #55868, .F. ) ;
#33168 = VECTOR ( 'NONE', #1281, 1000.000000000000227 ) ;
#33169 = VECTOR ( 'NONE', #31596, 1000.000000000000227 ) ;
#33170 = CARTESIAN_POINT ( 'NONE',  ( -68.22449927491872756, -8.912924279275781458, 6.175865180868210125 ) ) ;
#33171 = CARTESIAN_POINT ( 'NONE',  ( -24.26908309836554878, 0.000000000000000000, 6.108867788427308376 ) ) ;
#33172 = CARTESIAN_POINT ( 'NONE',  ( -19.32961685222932147, 0.000000000000000000, 14.39908572644263351 ) ) ;
#33173 = ORIENTED_EDGE ( 'NONE', *, *, #13321, .F. ) ;
#33174 = DIRECTION ( 'NONE',  ( 0.9999697198139515519, 0.000000000000000000, 0.007781995580013368816 ) ) ;
#33175 = ORIENTED_EDGE ( 'NONE', *, *, #27842, .T. ) ;
#33176 = LINE ( 'NONE', #46203, #47288 ) ;
#33177 = LINE ( 'NONE', #50496, #3949 ) ;
#33178 = EDGE_CURVE ( 'NONE', #42084, #41830, #35434, .T. ) ;
#33179 = PLANE ( 'NONE',  #38184 ) ;
#33180 = CARTESIAN_POINT ( 'NONE',  ( -11.18898947068464800, 8.786147236437516383, 1.127809914431977978 ) ) ;
#33181 = CARTESIAN_POINT ( 'NONE',  ( -19.27270800389901950, 0.000000000000000000, 7.086420930545378027 ) ) ;
#33182 = FACE_OUTER_BOUND ( 'NONE', #55082, .T. ) ;
#33184 = AXIS2_PLACEMENT_3D ( 'NONE', #52810, #13916, #31548 ) ;
#33183 = DIRECTION ( 'NONE',  ( 0.007781995580012663651, -3.146120232559066537E-19, -0.9999697198139514409 ) ) ;
#33185 = EDGE_CURVE ( 'NONE', #36655, #10808, #26937, .T. ) ;
#33186 = FACE_OUTER_BOUND ( 'NONE', #55678, .T. ) ;
#33187 = DIRECTION ( 'NONE',  ( 0.000000000000000000, -0.000000000000000000, -1.000000000000000000 ) ) ;
#33188 = ORIENTED_EDGE ( 'NONE', *, *, #32362, .F. ) ;
#33189 = DIRECTION ( 'NONE',  ( 0.007781995580012662783, 0.000000000000000000, -0.9999697198139514409 ) ) ;
#33190 = VERTEX_POINT ( 'NONE', #44250 ) ;
#33191 = VECTOR ( 'NONE', #11734, 1000.000000000000227 ) ;
#33192 = EDGE_CURVE ( 'NONE', #12359, #18681, #31482, .T. ) ;
#33193 = DIRECTION ( 'NONE',  ( 0.000000000000000000, -0.000000000000000000, -1.000000000000000000 ) ) ;
#33194 = LINE ( 'NONE', #42542, #34179 ) ;
#33195 = DIRECTION ( 'NONE',  ( -0.7660212471507179544, -0.6427876096865405842, -0.005961354470445141482 ) ) ;
#33196 = VECTOR ( 'NONE', #9426, 1000.000000000000114 ) ;
#33197 = DIRECTION ( 'NONE',  ( -0.5364919789714478471, 0.6444004775717705469, -0.5449076811759709926 ) ) ;
#33198 = CARTESIAN_POINT ( 'NONE',  ( -0.9975486161969306931, 4.078988103069860038, 3.605855335088290925 ) ) ;
#33199 = ADVANCED_FACE ( 'NONE', ( #50660 ), #37598, .F. ) ;
#33200 = AXIS2_PLACEMENT_3D ( 'NONE', #53093, #6499, #15305 ) ;
#33202 = AXIS2_PLACEMENT_3D ( 'NONE', #31904, #23118, #1233 ) ;
#33201 = PLANE ( 'NONE',  #48387 ) ;
#33203 = DIRECTION ( 'NONE',  ( 0.9981347984218673641, -0.06104853953485028795, -1.074405531565219116E-17 ) ) ;
#33204 = ORIENTED_EDGE ( 'NONE', *, *, #38278, .T. ) ;
#33205 = FACE_OUTER_BOUND ( 'NONE', #55399, .T. ) ;
#33206 = FACE_OUTER_BOUND ( 'NONE', #49872, .T. ) ;
#33207 = CARTESIAN_POINT ( 'NONE',  ( -19.17480688586491056, -0.1191753592594168992, 7.356511861379745554 ) ) ;
#33208 = CARTESIAN_POINT ( 'NONE',  ( -27.99767448711536133, 0.000000000000000000, 7.557179307314289218 ) ) ;
#33210 = VECTOR ( 'NONE', #29976, 999.9999999999998863 ) ;
#33209 = CARTESIAN_POINT ( 'NONE',  ( -23.29661890453421691, 19.01267837833611551, -4.488312987714206059 ) ) ;
#33211 = VECTOR ( 'NONE', #50420, 1000.000000000000227 ) ;
#33212 = DIRECTION ( 'NONE',  ( 0.9999697198139515519, 0.000000000000000000, 0.007781995580013368816 ) ) ;
#33213 = PLANE ( 'NONE',  #52043 ) ;
#33214 = CARTESIAN_POINT ( 'NONE',  ( -14.66887761629205222, 0.000000000000000000, 12.58869632783390990 ) ) ;
#33215 = PLANE ( 'NONE',  #32857 ) ;
#33216 = VERTEX_POINT ( 'NONE', #33900 ) ;
#33217 = VECTOR ( 'NONE', #869, 1000.000000000000227 ) ;
#33219 = CARTESIAN_POINT ( 'NONE',  ( -33.59133976979808978, -0.1191753592594197858, 9.829643557626155825 ) ) ;
#33218 = VECTOR ( 'NONE', #37359, 999.9999999999998863 ) ;
#33220 = CARTESIAN_POINT ( 'NONE',  ( -18.12108411398644492, 5.305366725996514710, 3.551507220766565442 ) ) ;
#33221 = VERTEX_POINT ( 'NONE', #54612 ) ;
#33222 = DIRECTION ( 'NONE',  ( 0.007781995580012662783, 0.000000000000000000, -0.9999697198139514409 ) ) ;
#33223 = DIRECTION ( 'NONE',  ( 0.000000000000000000, -0.000000000000000000, -1.000000000000000000 ) ) ;
#33224 = VERTEX_POINT ( 'NONE', #12021 ) ;
#33225 = VERTEX_POINT ( 'NONE', #33061 ) ;
#33226 = CARTESIAN_POINT ( 'NONE',  ( -18.39746900504187010, 0.000000000000000000, 14.03700784672088808 ) ) ;
#33227 = VECTOR ( 'NONE', #47884, 1000.000000000000000 ) ;
#33228 = ORIENTED_EDGE ( 'NONE', *, *, #23577, .F. ) ;
#33229 = ORIENTED_EDGE ( 'NONE', *, *, #37507, .T. ) ;
#33230 = ORIENTED_EDGE ( 'NONE', *, *, #36244, .F. ) ;
#33231 = DIRECTION ( 'NONE',  ( 0.005002170337468016433, -0.7660444431189770143, -0.6427681459581293666 ) ) ;
#33232 = CARTESIAN_POINT ( 'NONE',  ( -9.506711009720374861, 0.000000000000000000, 6.054425967900286309 ) ) ;
#33233 = AXIS2_PLACEMENT_3D ( 'NONE', #42038, #21013, #7694 ) ;
#33234 = DIRECTION ( 'NONE',  ( 0.005002170337468016433, -0.7660444431189770143, -0.6427681459581293666 ) ) ;
#33235 = EDGE_CURVE ( 'NONE', #32088, #43237, #16873, .T. ) ;
#33236 = VECTOR ( 'NONE', #43528, 999.9999999999998863 ) ;
#33237 = ORIENTED_EDGE ( 'NONE', *, *, #44705, .T. ) ;
#33238 = ORIENTED_EDGE ( 'NONE', *, *, #53990, .F. ) ;
#33239 = EDGE_CURVE ( 'NONE', #50886, #36877, #46968, .T. ) ;
#33240 = ADVANCED_FACE ( 'NONE', ( #15723 ), #24269, .F. ) ;
#33241 = VECTOR ( 'NONE', #9290, 1000.000000000000227 ) ;
#33242 = FACE_OUTER_BOUND ( 'NONE', #50483, .T. ) ;
#33243 = LINE ( 'NONE', #29229, #24545 ) ;
#33244 = VERTEX_POINT ( 'NONE', #55759 ) ;
#33245 = PLANE ( 'NONE',  #44553 ) ;
#33246 = VERTEX_POINT ( 'NONE', #55463 ) ;
#33247 = CARTESIAN_POINT ( 'NONE',  ( 2.072287782118878319, 0.000000000000000000, -2.950529333540147015 ) ) ;
#33248 = CARTESIAN_POINT ( 'NONE',  ( -14.50346148664584156, -0.6798977022406551551, 3.431396672244436008 ) ) ;
#33249 = VECTOR ( 'NONE', #29098, 1000.000000000000227 ) ;
#33250 = VERTEX_POINT ( 'NONE', #54924 ) ;
#33251 = VECTOR ( 'NONE', #48690, 999.9999999999998863 ) ;
#33252 = DIRECTION ( 'NONE',  ( 0.6427681459581294776, -0.7660444431189769032, 0.005002170337467562802 ) ) ;
#33253 = AXIS2_PLACEMENT_3D ( 'NONE', #20976, #37188, #20719 ) ;
#33254 = DIRECTION ( 'NONE',  ( 0.005961354470445682716, -0.6427876096865404731, -0.7660212471507180654 ) ) ;
#33255 = VECTOR ( 'NONE', #54912, 1000.000000000000227 ) ;
#33256 = ORIENTED_EDGE ( 'NONE', *, *, #47304, .F. ) ;
#33257 = CARTESIAN_POINT ( 'NONE',  ( -19.05834379240982202, 0.000000000000000000, 5.241428813372559503 ) ) ;
#33258 = CARTESIAN_POINT ( 'NONE',  ( -17.79526646286806724, -0.1191753592594177180, 9.213908112972596598 ) ) ;
#33259 = CARTESIAN_POINT ( 'NONE',  ( -13.73672976910459909, 0.000000000000000000, 12.22661844811216270 ) ) ;
#33260 = ORIENTED_EDGE ( 'NONE', *, *, #36619, .T. ) ;
#33261 = DIRECTION ( 'NONE',  ( 0.007781995580012663651, -3.146120232559066537E-19, -0.9999697198139514409 ) ) ;
#33262 = FACE_OUTER_BOUND ( 'NONE', #25038, .T. ) ;
#33263 = LINE ( 'NONE', #53988, #36708 ) ;
#33264 = DIRECTION ( 'NONE',  ( 0.6246952433987894571, -0.7422098413412800966, -0.2426528472758541777 ) ) ;
#33265 = EDGE_CURVE ( 'NONE', #17790, #56189, #29358, .T. ) ;
#33266 = DIRECTION ( 'NONE',  ( 0.005002170337468016433, -0.7660444431189770143, -0.6427681459581293666 ) ) ;
#33267 = CARTESIAN_POINT ( 'NONE',  ( -11.74754423342346321, 1.581621852479005552, 4.040177157639987193 ) ) ;
#33268 = VECTOR ( 'NONE', #46277, 1000.000000000000227 ) ;
#33269 = DIRECTION ( 'NONE',  ( -0.005002170337468016433, -0.7660444431189770143, 0.6427681459581293666 ) ) ;
#33270 = ORIENTED_EDGE ( 'NONE', *, *, #26124, .T. ) ;
#33272 = EDGE_CURVE ( 'NONE', #5918, #11612, #16031, .T. ) ;
#33271 = LINE ( 'NONE', #50579, #12646 ) ;
#33273 = DIRECTION ( 'NONE',  ( 0.6427681459581294776, -0.7660444431189769032, 0.005002170337467562802 ) ) ;
#33274 = CARTESIAN_POINT ( 'NONE',  ( -68.76879270600605309, -7.224796368693941748E-12, 7.369622379056993466 ) ) ;
#33275 = ORIENTED_EDGE ( 'NONE', *, *, #35947, .F. ) ;
#33276 = FACE_OUTER_BOUND ( 'NONE', #45281, .T. ) ;
#33278 = EDGE_CURVE ( 'NONE', #28372, #41541, #12335, .T. ) ;
#33277 = CARTESIAN_POINT ( 'NONE',  ( -20.87463720344803875, 3.038739411681508518, 4.693398030193443482 ) ) ;
#33279 = VECTOR ( 'NONE', #20342, 999.9999999999998863 ) ;
#33280 = EDGE_CURVE ( 'NONE', #37122, #17347, #16564, .T. ) ;
#33281 = LINE ( 'NONE', #16481, #18604 ) ;
#33282 = CARTESIAN_POINT ( 'NONE',  ( 0.1285714285714296967, 0.000000000000000000, 5.998622290806041590 ) ) ;
#33283 = CARTESIAN_POINT ( 'NONE',  ( -17.26532721389163072, 0.000000000000000000, 13.67648636611514590 ) ) ;
#33284 = ORIENTED_EDGE ( 'NONE', *, *, #23980, .T. ) ;
#33285 = VECTOR ( 'NONE', #31231, 1000.000000000000227 ) ;
#33286 = ORIENTED_EDGE ( 'NONE', *, *, #23515, .F. ) ;
#33287 = CARTESIAN_POINT ( 'NONE',  ( -19.32961685222932147, 0.000000000000000000, 14.39908572644263351 ) ) ;
#33288 = CARTESIAN_POINT ( 'NONE',  ( 2.072287782118878319, 0.000000000000000000, -2.950529333540147015 ) ) ;
#33289 = VECTOR ( 'NONE', #6773, 1000.000000000000114 ) ;
#33290 = VERTEX_POINT ( 'NONE', #11491 ) ;
#33291 = PLANE ( 'NONE',  #7748 ) ;
#33292 = ORIENTED_EDGE ( 'NONE', *, *, #31925, .F. ) ;
#33293 = DIRECTION ( 'NONE',  ( -0.6427681459581293666, -0.7660444431189770143, -0.005002170337467561935 ) ) ;
#33294 = AXIS2_PLACEMENT_3D ( 'NONE', #39774, #5980, #44019 ) ;
#33295 = ORIENTED_EDGE ( 'NONE', *, *, #6754, .F. ) ;
#33296 = ORIENTED_EDGE ( 'NONE', *, *, #42760, .T. ) ;
#33297 = VERTEX_POINT ( 'NONE', #24521 ) ;
#33298 = CARTESIAN_POINT ( 'NONE',  ( -11.70037978733358131, -0.1191753592594185229, 2.244030604059197742 ) ) ;
#33299 = ADVANCED_FACE ( 'NONE', ( #34205 ), #33354, .F. ) ;
#33300 = DIRECTION ( 'NONE',  ( 0.7660212471507180654, -0.6427876096865404731, 0.005961354470445141482 ) ) ;
#33301 = LINE ( 'NONE', #4324, #50242 ) ;
#33302 = ORIENTED_EDGE ( 'NONE', *, *, #29672, .F. ) ;
#33303 = DIRECTION ( 'NONE',  ( -0.005961354470445682716, -0.6427876096865404731, 0.7660212471507180654 ) ) ;
#33304 = B_SPLINE_CURVE_WITH_KNOTS ( 'NONE', 3,
 ( #20843, #46690, #17723, #17159 ),
 .UNSPECIFIED., .F., .F.,
 ( 4, 4 ),
 ( 0.000000000000000000, 0.0003538274413750240122 ),
 .UNSPECIFIED. ) ;
#33305 = VERTEX_POINT ( 'NONE', #19982 ) ;
#33306 = EDGE_CURVE ( 'NONE', #54123, #20350, #8070, .T. ) ;
#33307 = ORIENTED_EDGE ( 'NONE', *, *, #40443, .T. ) ;
#33308 = VERTEX_POINT ( 'NONE', #51513 ) ;
#33309 = DIRECTION ( 'NONE',  ( -0.5449076811759708816, 0.6444004775717707689, 0.5364919789714475140 ) ) ;
#33310 = DIRECTION ( 'NONE',  ( 0.7660212471507180654, -0.6427876096865404731, 0.005961354470445141482 ) ) ;
#33311 = ORIENTED_EDGE ( 'NONE', *, *, #31930, .T. ) ;
#33312 = CARTESIAN_POINT ( 'NONE',  ( -21.37940959735528423, -5.536956232915666298, 5.009151959621898520 ) ) ;
#33313 = ORIENTED_EDGE ( 'NONE', *, *, #6426, .F. ) ;
#33314 = LINE ( 'NONE', #45787, #44904 ) ;
#33315 = DIRECTION ( 'NONE',  ( 0.000000000000000000, 1.000000000000000000, 0.000000000000000000 ) ) ;
#33316 = EDGE_LOOP ( 'NONE', ( #6478, #28073, #16535, #43741 ) ) ;
#33317 = CARTESIAN_POINT ( 'NONE',  ( -17.96629124694975488, 4.495856970884008597, 11.23850599833945552 ) ) ;
#33318 = ORIENTED_EDGE ( 'NONE', *, *, #37370, .F. ) ;
#33319 = ADVANCED_FACE ( 'NONE', ( #41835 ), #7487, .F. ) ;
#33320 = VECTOR ( 'NONE', #24584, 1000.000000000000114 ) ;
#33321 = DIRECTION ( 'NONE',  ( 0.000000000000000000, -0.000000000000000000, -1.000000000000000000 ) ) ;
#33322 = CARTESIAN_POINT ( 'NONE',  ( -10.27421835998572064, 0.000000000000000000, 10.96090226820206048 ) ) ;
#33323 = LINE ( 'NONE', #15168, #22348 ) ;
#33324 = LINE ( 'NONE', #29038, #30590 ) ;
#33325 = CARTESIAN_POINT ( 'NONE',  ( -17.74404816805336793, 0.000000000000000000, 3.574322630375089460 ) ) ;
#33326 = ORIENTED_EDGE ( 'NONE', *, *, #22969, .T. ) ;
#33327 = ORIENTED_EDGE ( 'NONE', *, *, #38444, .T. ) ;
#33328 = VECTOR ( 'NONE', #17181, 1000.000000000000000 ) ;
#33329 = LINE ( 'NONE', #55436, #18276 ) ;
#33330 = PLANE ( 'NONE',  #33951 ) ;
#33331 = CARTESIAN_POINT ( 'NONE',  ( -9.359795358673375532, -2.003343105922557488, 2.897185656270504062 ) ) ;
#33332 = DIRECTION ( 'NONE',  ( -0.9999697198139514409, -0.000000000000000000, -0.007781995580013368816 ) ) ;
#33333 = CARTESIAN_POINT ( 'NONE',  ( -17.33547259272246066, -2.946525016555662457, 3.520997812542008720 ) ) ;
#33334 = LINE ( 'NONE', #51492, #24917 ) ;
#33335 = EDGE_LOOP ( 'NONE', ( #23507, #44340, #53422, #50470 ) ) ;
#33336 = LINE ( 'NONE', #46352, #35899 ) ;
#33337 = LINE ( 'NONE', #42666, #20492 ) ;
#33338 = EDGE_LOOP ( 'NONE', ( #4791, #51722, #7177, #28517 ) ) ;
#33339 = FACE_OUTER_BOUND ( 'NONE', #45938, .T. ) ;
#33340 = DIRECTION ( 'NONE',  ( 0.8531650599175527594, 0.4028455766673922356, -0.3313982828793700652 ) ) ;
#33341 = EDGE_LOOP ( 'NONE', ( #33238, #42343, #30860, #40023 ) ) ;
#33342 = CARTESIAN_POINT ( 'NONE',  ( -70.11839600776268355, -1.000000000000000222, -7.555920072494595630 ) ) ;
#33343 = LINE ( 'NONE', #15710, #16985 ) ;
#33344 = EDGE_CURVE ( 'NONE', #32684, #171, #25120, .T. ) ;
#33345 = DIRECTION ( 'NONE',  ( 0.7660212471507180654, -0.6427876096865404731, 0.005961354470445141482 ) ) ;
#33346 = CARTESIAN_POINT ( 'NONE',  ( -16.37836334430254581, -0.1191753592594192307, 6.270278222214512809 ) ) ;
#33347 = CARTESIAN_POINT ( 'NONE',  ( -12.13851405436063047, 0.000000000000000000, 11.68505802764555135 ) ) ;
#33348 = ORIENTED_EDGE ( 'NONE', *, *, #12341, .T. ) ;
#33349 = ORIENTED_EDGE ( 'NONE', *, *, #458, .F. ) ;
#33350 = PLANE ( 'NONE',  #38508 ) ;
#33351 = CARTESIAN_POINT ( 'NONE',  ( -20.44726175016783287, -5.536956232915667186, 4.647074079900152199 ) ) ;
#33352 = DIRECTION ( 'NONE',  ( -0.5364919789714478471, 0.6444004775717705469, -0.5449076811759709926 ) ) ;
#33353 = EDGE_CURVE ( 'NONE', #7607, #37255, #45836, .T. ) ;
#33354 = PLANE ( 'NONE',  #49633 ) ;
#33355 = LINE ( 'NONE', #15446, #25564 ) ;
#33356 = PLANE ( 'NONE',  #14971 ) ;
#33358 = ADVANCED_FACE ( 'NONE', ( #2661 ), #37303, .F. ) ;
#33357 = ORIENTED_EDGE ( 'NONE', *, *, #29506, .T. ) ;
#33359 = CARTESIAN_POINT ( 'NONE',  ( 2.072287782118878319, 0.000000000000000000, -2.950529333540147015 ) ) ;
#33360 = ADVANCED_FACE ( 'NONE', ( #16286 ), #17144, .F. ) ;
#33362 = AXIS2_PLACEMENT_3D ( 'NONE', #52353, #39273, #30770 ) ;
#33361 = DIRECTION ( 'NONE',  ( -0.005002170337468016433, -0.7660444431189770143, 0.6427681459581293666 ) ) ;
#33363 = CARTESIAN_POINT ( 'NONE',  ( -69.66347483736342383, -8.676648739292067702, -7.503912900124009688 ) ) ;
#33364 = ORIENTED_EDGE ( 'NONE', *, *, #42686, .T. ) ;
#33365 = CARTESIAN_POINT ( 'NONE',  ( -67.86660508942482295, -11.27593752063030053, 7.471997583267847354 ) ) ;
#33366 = EDGE_CURVE ( 'NONE', #18631, #10456, #30503, .T. ) ;
#33367 = DIRECTION ( 'NONE',  ( 0.6427681459581294776, -0.7660444431189769032, 0.005002170337467562802 ) ) ;
#33368 = DIRECTION ( 'NONE',  ( 0.007781995580012662783, 0.000000000000000000, -0.9999697198139514409 ) ) ;
#33369 = EDGE_LOOP ( 'NONE', ( #42457, #56083 ) ) ;
#33370 = VECTOR ( 'NONE', #36135, 1000.000000000000227 ) ;
#33371 = DIRECTION ( 'NONE',  ( -0.005002170337468016433, -0.7660444431189770143, 0.6427681459581293666 ) ) ;
#33372 = EDGE_CURVE ( 'NONE', #34449, #30378, #8330, .T. ) ;
#33373 = VERTEX_POINT ( 'NONE', #25650 ) ;
#33374 = ADVANCED_FACE ( 'NONE', ( #22530 ), #362, .F. ) ;
#33375 = ORIENTED_EDGE ( 'NONE', *, *, #4093, .F. ) ;
#33376 = VERTEX_POINT ( 'NONE', #17703 ) ;
#33377 = ORIENTED_EDGE ( 'NONE', *, *, #32334, .F. ) ;
#33378 = LINE ( 'NONE', #7512, #33857 ) ;
#33379 = ORIENTED_EDGE ( 'NONE', *, *, #38661, .T. ) ;
#33380 = EDGE_CURVE ( 'NONE', #34545, #1702, #30199, .T. ) ;
#33381 = ORIENTED_EDGE ( 'NONE', *, *, #7952, .F. ) ;
#33382 = LINE ( 'NONE', #6990, #40398 ) ;
#33383 = ORIENTED_EDGE ( 'NONE', *, *, #1427, .T. ) ;
#33384 = VERTEX_POINT ( 'NONE', #38740 ) ;
#33385 = ADVANCED_FACE ( 'NONE', ( #48342 ), #21415, .F. ) ;
#33386 = DIRECTION ( 'NONE',  ( -0.9999697198139514409, -0.000000000000000000, -0.007781995580013368816 ) ) ;
#33387 = DIRECTION ( 'NONE',  ( 0.5364919789714477361, 0.6444004775717706579, 0.5449076811759711036 ) ) ;
#33388 = LINE ( 'NONE', #15759, #12379 ) ;
#33389 = CARTESIAN_POINT ( 'NONE',  ( -12.71487129044241904, 1.095915999411505526, 1.585854081413927474 ) ) ;
#33390 = ORIENTED_EDGE ( 'NONE', *, *, #314, .T. ) ;
#33391 = ORIENTED_EDGE ( 'NONE', *, *, #47917, .T. ) ;
#33392 = DIRECTION ( 'NONE',  ( -0.7886751345948130876, 0.2113248654051844977, 0.5773502691896263972 ) ) ;
#33393 = DIRECTION ( 'NONE',  ( -0.005002170337468016433, -0.7660444431189770143, 0.6427681459581293666 ) ) ;
#33394 = LINE ( 'NONE', #50700, #5207 ) ;
#33395 = FACE_OUTER_BOUND ( 'NONE', #52749, .T. ) ;
#33396 = LINE ( 'NONE', #28857, #51241 ) ;
#33397 = LINE ( 'NONE', #11793, #34982 ) ;
#33398 = VERTEX_POINT ( 'NONE', #52608 ) ;
#33399 = DIRECTION ( 'NONE',  ( 0.9999697198139515519, 0.000000000000000000, 0.007781995580013368816 ) ) ;
#33400 = VERTEX_POINT ( 'NONE', #39579 ) ;
#33401 = VECTOR ( 'NONE', #13071, 999.9999999999998863 ) ;
#33402 = CARTESIAN_POINT ( 'NONE',  ( -12.81515292046355725, 2.876837460659008361, 1.567986153331332844 ) ) ;
#33403 = LINE ( 'NONE', #50709, #29304 ) ;
#33404 = DIRECTION ( 'NONE',  ( 0.7660212471507180654, -0.6427876096865404731, 0.005961354470445141482 ) ) ;
#33405 = DIRECTION ( 'NONE',  ( 0.005961354470445682716, -0.6427876096865404731, -0.7660212471507180654 ) ) ;
#33406 = EDGE_CURVE ( 'NONE', #18987, #36742, #36648, .T. ) ;
#33407 = CARTESIAN_POINT ( 'NONE',  ( -16.44621519763577666, -5.213152330870664208, 3.103262762558621990 ) ) ;
#33408 = CARTESIAN_POINT ( 'NONE',  ( -20.11466289002168750, 1.581621852479007106, 4.444687877008841603 ) ) ;
#33409 = ORIENTED_EDGE ( 'NONE', *, *, #46909, .F. ) ;
#33410 = ORIENTED_EDGE ( 'NONE', *, *, #16983, .T. ) ;
#33411 = DIRECTION ( 'NONE',  ( 0.9999697198139515519, 0.000000000000000000, 0.007781995580013368816 ) ) ;
#33412 = CARTESIAN_POINT ( 'NONE',  ( -20.59425094460877403, 20.76817951925234951, 4.326372769521754869 ) ) ;
#33413 = LINE ( 'NONE', #25437, #49654 ) ;
#33414 = ADVANCED_FACE ( 'NONE', ( #47816 ), #43287, .F. ) ;
#33415 = ADVANCED_FACE ( 'NONE', ( #21945 ), #17987, .F. ) ;
#33416 = PLANE ( 'NONE',  #43675 ) ;
#33417 = CARTESIAN_POINT ( 'NONE',  ( -15.88130887279446490, 0.000000000000000000, 3.050160814894388839 ) ) ;
#33418 = DIRECTION ( 'NONE',  ( -0.9999697198139514409, -0.000000000000000000, -0.007781995580013368816 ) ) ;
#33419 = LINE ( 'NONE', #50725, #47411 ) ;
#33420 = EDGE_CURVE ( 'NONE', #20361, #24739, #5218, .T. ) ;
#33421 = LINE ( 'NONE', #11818, #36887 ) ;
#33422 = DIRECTION ( 'NONE',  ( 0.007781995580012662783, 0.000000000000000000, -0.9999697198139514409 ) ) ;
#33423 = ORIENTED_EDGE ( 'NONE', *, *, #15200, .T. ) ;
#33424 = ORIENTED_EDGE ( 'NONE', *, *, #13822, .F. ) ;
#33425 = EDGE_CURVE ( 'NONE', #17269, #43836, #26222, .T. ) ;
#33426 = EDGE_CURVE ( 'NONE', #547, #40934, #12606, .T. ) ;
#33427 = EDGE_LOOP ( 'NONE', ( #52912, #4338, #19971, #40431 ) ) ;
#33428 = EDGE_LOOP ( 'NONE', ( #35193, #30610, #13189, #38390 ) ) ;
#33429 = ORIENTED_EDGE ( 'NONE', *, *, #2580, .T. ) ;
#33430 = ORIENTED_EDGE ( 'NONE', *, *, #25713, .T. ) ;
#33431 = CARTESIAN_POINT ( 'NONE',  ( -15.40103151951671734, 0.000000000000000000, 12.95233060667165681 ) ) ;
#33432 = DIRECTION ( 'NONE',  ( 0.5364919789714477361, 0.6444004775717706579, 0.5449076811759711036 ) ) ;
#33433 = CARTESIAN_POINT ( 'NONE',  ( -68.13739796841800000, -7.564004218980900450E-15, 7.461800464507161834 ) ) ;
#33434 = EDGE_CURVE ( 'NONE', #44937, #37525, #17404, .T. ) ;
#33435 = VECTOR ( 'NONE', #30760, 999.9999999999998863 ) ;
#33436 = ORIENTED_EDGE ( 'NONE', *, *, #43243, .T. ) ;
#33437 = CARTESIAN_POINT ( 'NONE',  ( -20.54204810873173415, 0.000000000000000000, 4.860550213503115558 ) ) ;
#33438 = ORIENTED_EDGE ( 'NONE', *, *, #29322, .F. ) ;
#33439 = CARTESIAN_POINT ( 'NONE',  ( -18.11889143909580469, 0.000000000000000000, 3.940737583172497782 ) ) ;
#33440 = ORIENTED_EDGE ( 'NONE', *, *, #7076, .T. ) ;
#33441 = CARTESIAN_POINT ( 'NONE',  ( -67.46750306152793542, -8.826476960856009413, 4.644600239863266644 ) ) ;
#33442 = CARTESIAN_POINT ( 'NONE',  ( -15.60102546347950536, 0.000000000000000000, 12.95077420755565356 ) ) ;
#33443 = CARTESIAN_POINT ( 'NONE',  ( -18.34918231722741666, 0.000000000000000000, 7.832272160596925659 ) ) ;
#33444 = ORIENTED_EDGE ( 'NONE', *, *, #33631, .F. ) ;
#33445 = DIRECTION ( 'NONE',  ( -0.3620778797217457656, 0.000000000000000000, -0.9321478471874539151 ) ) ;
#33446 = ORIENTED_EDGE ( 'NONE', *, *, #26638, .F. ) ;
#33447 = DIRECTION ( 'NONE',  ( 0.9999697198139515519, 0.000000000000000000, 0.007781995580013368816 ) ) ;
#33448 = DIRECTION ( 'NONE',  ( -0.6427681459581293666, -0.7660444431189770143, -0.005002170337467561935 ) ) ;
#33449 = LINE ( 'NONE', #28635, #34191 ) ;
#33450 = LINE ( 'NONE', #11848, #1398 ) ;
#33451 = CARTESIAN_POINT ( 'NONE',  ( -28.92982233430281980, 0.000000000000000000, 7.919257187036034651 ) ) ;
#33452 = CARTESIAN_POINT ( 'NONE',  ( -18.86354292863559579, 0.000000000000000000, 14.21804678658176080 ) ) ;
#33453 = LINE ( 'NONE', #51343, #2160 ) ;
#33454 = DIRECTION ( 'NONE',  ( 0.007781995580012663651, 0.000000000000000000, -0.9999697198139515519 ) ) ;
#33455 = ORIENTED_EDGE ( 'NONE', *, *, #40578, .T. ) ;
#33456 = FACE_OUTER_BOUND ( 'NONE', #3043, .T. ) ;
#33457 = EDGE_LOOP ( 'NONE', ( #53294, #19933, #49132, #35007 ) ) ;
#33458 = ADVANCED_FACE ( 'NONE', ( #56054 ), #34455, .F. ) ;
#33459 = LINE ( 'NONE', #34313, #16574 ) ;
#33460 = DIRECTION ( 'NONE',  ( 0.005002170337468016433, -0.7660444431189770143, -0.6427681459581293666 ) ) ;
#33461 = DIRECTION ( 'NONE',  ( 0.6427681459581294776, -0.7660444431189769032, 0.005002170337467562802 ) ) ;
#33462 = EDGE_CURVE ( 'NONE', #52707, #46034, #67, .T. ) ;
#33463 = DIRECTION ( 'NONE',  ( -0.5364919789714478471, 0.6444004775717705469, -0.5449076811759709926 ) ) ;
#33464 = DIRECTION ( 'NONE',  ( -0.7660212471507179544, -0.6427876096865405842, -0.005961354470445141482 ) ) ;
#33465 = CARTESIAN_POINT ( 'NONE',  ( -30.79411802867772607, 0.000000000000000000, 8.643412946479525516 ) ) ;
#33466 =( NAMED_UNIT ( * ) SI_UNIT ( $, .STERADIAN. ) SOLID_ANGLE_UNIT ( ) );
#33467 = ORIENTED_EDGE ( 'NONE', *, *, #37593, .T. ) ;
#33468 = EDGE_CURVE ( 'NONE', #48904, #46790, #13166, .T. ) ;
#33469 = DIRECTION ( 'NONE',  ( -0.9999697198139514409, -0.000000000000000000, -0.007781995580013368816 ) ) ;
#33470 = DIRECTION ( 'NONE',  ( 0.007781995580012663651, 0.000000000000000000, -0.9999697198139515519 ) ) ;
#33471 = LINE ( 'NONE', #34038, #411 ) ;
#33472 = CARTESIAN_POINT ( 'NONE',  ( -22.40634380310664397, 0.000000000000000000, 5.584705972946605534 ) ) ;
#33473 = ADVANCED_FACE ( 'NONE', ( #1197 ), #44942, .F. ) ;
#33474 = ADVANCED_FACE ( 'NONE', ( #23370 ), #14836, .F. ) ;
#33475 = EDGE_CURVE ( 'NONE', #3340, #22086, #45472, .T. ) ;
#33476 = CARTESIAN_POINT ( 'NONE',  ( -21.93567689722629765, 19.99370688441071309, 4.657440554554202805 ) ) ;
#33477 = FACE_OUTER_BOUND ( 'NONE', #43471, .T. ) ;
#33478 = ADVANCED_FACE ( 'NONE', ( #36154 ), #40107, .F. ) ;
#33479 = CARTESIAN_POINT ( 'NONE',  ( -17.77802214183636664, -0.1191753592594185784, 6.998049893426011359 ) ) ;
#33480 = DIRECTION ( 'NONE',  ( 0.000000000000000000, -0.000000000000000000, -1.000000000000000000 ) ) ;
#33481 = ORIENTED_EDGE ( 'NONE', *, *, #16058, .T. ) ;
#33482 = CARTESIAN_POINT ( 'NONE',  ( -18.32463349006915010, 0.000000000000000000, 4.677800590572023687 ) ) ;
#33483 = DIRECTION ( 'NONE',  ( 0.7660212471507180654, -0.6427876096865404731, 0.005961354470445141482 ) ) ;
#33484 = ORIENTED_EDGE ( 'NONE', *, *, #18549, .T. ) ;
#33485 = EDGE_LOOP ( 'NONE', ( #16393, #12239, #26266, #44232 ) ) ;
#33486 = CARTESIAN_POINT ( 'NONE',  ( -17.06374735823969147, 1.257817950434005461, 5.573753622435739352 ) ) ;
#33487 = ORIENTED_EDGE ( 'NONE', *, *, #3788, .T. ) ;
#33488 = EDGE_CURVE ( 'NONE', #33893, #17923, #28160, .T. ) ;
#33489 = VERTEX_POINT ( 'NONE', #27621 ) ;
#33490 = CARTESIAN_POINT ( 'NONE',  ( -18.76354595665420177, -0.1191753592594177458, 14.21882498613976331 ) ) ;
#33491 = EDGE_CURVE ( 'NONE', #45690, #44220, #44372, .T. ) ;
#33492 = ORIENTED_EDGE ( 'NONE', *, *, #53911, .T. ) ;
#33493 = EDGE_LOOP ( 'NONE', ( #40994, #54354, #23732, #11357 ) ) ;
#33494 = ORIENTED_EDGE ( 'NONE', *, *, #53238, .T. ) ;
#33495 = EDGE_CURVE ( 'NONE', #41657, #18997, #32451, .T. ) ;
#33496 = CARTESIAN_POINT ( 'NONE',  ( -17.67880336941297870, 0.000000000000000000, 7.098825064965410547 ) ) ;
#33497 = CARTESIAN_POINT ( 'NONE',  ( -11.33496166291588558, 0.000000000000000000, 2.146871344287814232 ) ) ;
#33498 = FACE_OUTER_BOUND ( 'NONE', #15650, .T. ) ;
#33499 = ADVANCED_FACE ( 'NONE', ( #6583 ), #31611, .F. ) ;
#33500 = ORIENTED_EDGE ( 'NONE', *, *, #50933, .T. ) ;
#33501 = ORIENTED_EDGE ( 'NONE', *, *, #54985, .T. ) ;
#33502 = EDGE_CURVE ( 'NONE', #17567, #45180, #29123, .T. ) ;
#33503 = CARTESIAN_POINT ( 'NONE',  ( -11.83696125532564558, 0.000000000000000000, 6.944281574870742269 ) ) ;
#33504 = DIRECTION ( 'NONE',  ( 0.005961354470445682716, -0.6427876096865404731, -0.7660212471507180654 ) ) ;
#33505 = ORIENTED_EDGE ( 'NONE', *, *, #54229, .T. ) ;
#33506 = PLANE ( 'NONE',  #34588 ) ;
#33507 = ORIENTED_EDGE ( 'NONE', *, *, #21989, .T. ) ;
#33508 = CARTESIAN_POINT ( 'NONE',  ( -12.77226246836278989, 0.6102101463440035012, 1.623643323592976140 ) ) ;
#33509 = DIRECTION ( 'NONE',  ( 0.007781995580012663651, -3.146120232559066537E-19, -0.9999697198139514409 ) ) ;
#33510 = AXIS2_PLACEMENT_3D ( 'NONE', #45392, #1942, #19572 ) ;
#33511 = ORIENTED_EDGE ( 'NONE', *, *, #38026, .F. ) ;
#33512 = CARTESIAN_POINT ( 'NONE',  ( 5.282355347525632183, -1.069580340602398705, -2.393146392891059460 ) ) ;
#33513 = DIRECTION ( 'NONE',  ( 0.005961354470445682716, -0.6427876096865404731, -0.7660212471507180654 ) ) ;
#33514 = ORIENTED_EDGE ( 'NONE', *, *, #50480, .F. ) ;
#33515 = LINE ( 'NONE', #42589, #15865 ) ;
#33516 = DIRECTION ( 'NONE',  ( 0.007781995580012663651, 0.000000000000000000, -0.9999697198139515519 ) ) ;
#33517 = FACE_OUTER_BOUND ( 'NONE', #30016, .T. ) ;
#33518 = EDGE_LOOP ( 'NONE', ( #24408, #47539, #34963, #37713 ) ) ;
#33519 = DIRECTION ( 'NONE',  ( 0.000000000000000000, -1.000000000000000000, 0.000000000000000000 ) ) ;
#33520 = DIRECTION ( 'NONE',  ( 0.000000000000000000, -0.000000000000000000, -1.000000000000000000 ) ) ;
#33521 = DIRECTION ( 'NONE',  ( 0.9999697198139515519, 0.000000000000000000, 0.007781995580013368816 ) ) ;
#33522 = DIRECTION ( 'NONE',  ( 0.9999697198139515519, 0.000000000000000000, 0.007781995580013368816 ) ) ;
#33523 = DIRECTION ( 'NONE',  ( 0.005961354470445682716, -0.6427876096865404731, -0.7660212471507180654 ) ) ;
#33524 = CARTESIAN_POINT ( 'NONE',  ( -21.57722033895402092, 4.981562823951513508, 4.904318941198996029 ) ) ;
#33525 = CARTESIAN_POINT ( 'NONE',  ( -69.38651902536496152, -9.785563849073980691, -7.442420802397360369 ) ) ;
#33526 = EDGE_LOOP ( 'NONE', ( #51713, #19426, #40501, #3279 ) ) ;
#33527 = CARTESIAN_POINT ( 'NONE',  ( -16.72366309418326225, 0.000000000000000000, 3.782269559181549390 ) ) ;
#33528 = DIRECTION ( 'NONE',  ( 0.007781995580012662783, 0.000000000000000000, -0.9999697198139514409 ) ) ;
#33529 = DIRECTION ( 'NONE',  ( 0.5449076811759707706, 0.6444004775717708799, -0.5364919789714476250 ) ) ;
#33530 = ORIENTED_EDGE ( 'NONE', *, *, #208, .F. ) ;
#33531 = LINE ( 'NONE', #41505, #2982 ) ;
#33532 = DIRECTION ( 'NONE',  ( 0.5449076811759707706, 0.6444004775717708799, -0.5364919789714476250 ) ) ;
#33533 = EDGE_CURVE ( 'NONE', #14352, #21126, #6063, .T. ) ;
#33534 = EDGE_CURVE ( 'NONE', #12878, #23644, #19659, .T. ) ;
#33535 = CARTESIAN_POINT ( 'NONE',  ( -11.22056963685719211, 0.000000000000000000, 1.239771416285661010 ) ) ;
#33536 = EDGE_CURVE ( 'NONE', #40102, #44513, #27918, .T. ) ;
#33537 = LINE ( 'NONE', #2316, #54127 ) ;
#33538 = PLANE ( 'NONE',  #26574 ) ;
#33539 = EDGE_LOOP ( 'NONE', ( #19799, #1898, #47099, #44043, #34071 ) ) ;
#33540 = ORIENTED_EDGE ( 'NONE', *, *, #40906, .T. ) ;
#33541 = CARTESIAN_POINT ( 'NONE',  ( -25.84533253705052047, 17.69690203054840794, 4.605409525904272883 ) ) ;
#33542 = DIRECTION ( 'NONE',  ( 0.5364919789714477361, 0.6444004775717706579, 0.5449076811759711036 ) ) ;
#33543 = VERTEX_POINT ( 'NONE', #49757 ) ;
#33544 = FACE_OUTER_BOUND ( 'NONE', #8938, .T. ) ;
#33545 = ORIENTED_EDGE ( 'NONE', *, *, #34015, .T. ) ;
#33546 = LINE ( 'NONE', #34400, #24745 ) ;
#33547 = ORIENTED_EDGE ( 'NONE', *, *, #51788, .F. ) ;
#33548 = VERTEX_POINT ( 'NONE', #2324 ) ;
#33549 = ORIENTED_EDGE ( 'NONE', *, *, #10263, .F. ) ;
#33550 = PLANE ( 'NONE',  #43763 ) ;
#33551 = DIRECTION ( 'NONE',  ( 0.6427681459581294776, -0.7660444431189769032, 0.005002170337467562802 ) ) ;
#33552 = DIRECTION ( 'NONE',  ( 0.007781995580012663651, 0.000000000000000000, -0.9999697198139515519 ) ) ;
#33553 = DIRECTION ( 'NONE',  ( 0.7660212471507180654, -0.6427876096865404731, 0.005961354470445141482 ) ) ;
#33554 = ORIENTED_EDGE ( 'NONE', *, *, #21253, .T. ) ;
#33555 = ADVANCED_FACE ( 'NONE', ( #52888 ), #6320, .F. ) ;
#33556 = ORIENTED_EDGE ( 'NONE', *, *, #36953, .T. ) ;
#33557 = ORIENTED_EDGE ( 'NONE', *, *, #36547, .T. ) ;
#33558 = CARTESIAN_POINT ( 'NONE',  ( -10.77487009789602368, -0.6798977022406563764, 1.983085153357455166 ) ) ;
#33559 = EDGE_CURVE ( 'NONE', #40825, #28225, #35875, .T. ) ;
#33560 = CARTESIAN_POINT ( 'NONE',  ( -27.99767448711536133, 0.000000000000000000, 7.557179307314289218 ) ) ;
#33561 = ORIENTED_EDGE ( 'NONE', *, *, #6930, .F. ) ;
#33562 = CARTESIAN_POINT ( 'NONE',  ( -17.78951835585749919, -0.1191753592594190225, 8.475288706457071441 ) ) ;
#33563 = EDGE_CURVE ( 'NONE', #12727, #2320, #36405, .T. ) ;
#33564 = ORIENTED_EDGE ( 'NONE', *, *, #27342, .F. ) ;
#33565 = DIRECTION ( 'NONE',  ( -0.5364919789714478471, 0.6444004775717705469, -0.5449076811759709926 ) ) ;
#33566 = FACE_OUTER_BOUND ( 'NONE', #38027, .T. ) ;
#33567 = ORIENTED_EDGE ( 'NONE', *, *, #32701, .T. ) ;
#33568 = EDGE_CURVE ( 'NONE', #12564, #22624, #31323, .T. ) ;
#33569 = LINE ( 'NONE', #6915, #44951 ) ;
#33570 = ORIENTED_EDGE ( 'NONE', *, *, #9897, .T. ) ;
#33571 = AXIS2_PLACEMENT_3D ( 'NONE', #20079, #37408, #35976 ) ;
#33572 = LINE ( 'NONE', #7185, #154 ) ;
#33573 = CARTESIAN_POINT ( 'NONE',  ( -25.20200914511100265, -0.1191753592594197858, 6.570942640130446932 ) ) ;
#33574 = ORIENTED_EDGE ( 'NONE', *, *, #13911, .F. ) ;
#33575 = CARTESIAN_POINT ( 'NONE',  ( -18.97020357541589775, -4.889348428825664783, 4.093996603269308920 ) ) ;
#33576 = DIRECTION ( 'NONE',  ( -0.7660212471507179544, -0.6427876096865405842, -0.005961354470445141482 ) ) ;
#33577 = PLANE ( 'NONE',  #5120 ) ;
#33578 = FACE_OUTER_BOUND ( 'NONE', #38513, .T. ) ;
#33579 = ORIENTED_EDGE ( 'NONE', *, *, #41766, .T. ) ;
#33580 = VERTEX_POINT ( 'NONE', #22788 ) ;
#33581 = CARTESIAN_POINT ( 'NONE',  ( -16.99924723426068951, 0.000000000000000000, 13.49389102713827171 ) ) ;
#33582 = FACE_OUTER_BOUND ( 'NONE', #29533, .T. ) ;
#33583 = CARTESIAN_POINT ( 'NONE',  ( -69.79011221730237935, 0.1328921168376125672, 7.235198260161163297 ) ) ;
#33584 = CARTESIAN_POINT ( 'NONE',  ( -14.01623497886155256, -0.1191753592594197858, 2.226008083469502630 ) ) ;
#33585 = CARTESIAN_POINT ( 'NONE',  ( 2.072287782118878319, 0.000000000000000000, -2.950529333540147015 ) ) ;
#33586 = CARTESIAN_POINT ( 'NONE',  ( -25.20278734466900517, 0.000000000000000000, 6.670939612111840944 ) ) ;
#33587 = ORIENTED_EDGE ( 'NONE', *, *, #5350, .F. ) ;
#33588 = CARTESIAN_POINT ( 'NONE',  ( -12.64402384854216699, -0.1191753592594183703, 4.083347296812000593 ) ) ;
#33589 = CARTESIAN_POINT ( 'NONE',  ( -13.07066190154808361, 0.000000000000000000, 12.04713590736729678 ) ) ;
#33590 = ORIENTED_EDGE ( 'NONE', *, *, #23661, .T. ) ;
#33591 = CARTESIAN_POINT ( 'NONE',  ( -16.47470806322066039, 0.000000000000000000, 5.800193347417353706 ) ) ;
#33592 = VERTEX_POINT ( 'NONE', #29589 ) ;
#33593 = EDGE_CURVE ( 'NONE', #14093, #4092, #11412, .T. ) ;
#33594 = DIRECTION ( 'NONE',  ( 0.005961354470445682716, -0.6427876096865404731, -0.7660212471507180654 ) ) ;
#33595 = CARTESIAN_POINT ( 'NONE',  ( -15.46345981814678616, -0.1191753592594185784, 8.124058562039351727 ) ) ;
#33596 = CARTESIAN_POINT ( 'NONE',  ( -9.075990533167328067, 0.000000000000000000, 10.41622904950343909 ) ) ;
#33597 = EDGE_CURVE ( 'NONE', #48717, #460, #46902, .T. ) ;
#33598 = EDGE_CURVE ( 'NONE', #32693, #38304, #37236, .T. ) ;
#33599 = DIRECTION ( 'NONE',  ( -0.005002170337468016433, -0.7660444431189770143, 0.6427681459581293666 ) ) ;
#33600 = CARTESIAN_POINT ( 'NONE',  ( -69.14117849623558243, 2.000000000007579271, 6.564485215139889362 ) ) ;
#33601 = ORIENTED_EDGE ( 'NONE', *, *, #55448, .T. ) ;
#33602 = VERTEX_POINT ( 'NONE', #16492 ) ;
#33603 = CARTESIAN_POINT ( 'NONE',  ( -16.53317331066696383, 0.000000000000000000, 13.31285208727739899 ) ) ;
#33604 = FACE_OUTER_BOUND ( 'NONE', #51245, .T. ) ;
#33605 = DIRECTION ( 'NONE',  ( 0.9999697198139515519, 0.000000000000000000, 0.007781995580013368816 ) ) ;
#33606 = CARTESIAN_POINT ( 'NONE',  ( -61.74810725808001877, 6.470640170577545369, 2.999999999999993339 ) ) ;
#33607 = FACE_OUTER_BOUND ( 'NONE', #47906, .T. ) ;
#33608 = DIRECTION ( 'NONE',  ( 0.9999697198139515519, 0.000000000000000000, 0.007781995580013368816 ) ) ;
#33609 = ORIENTED_EDGE ( 'NONE', *, *, #51959, .T. ) ;
#33610 = PLANE ( 'NONE',  #7484 ) ;
#33611 = EDGE_CURVE ( 'NONE', #52077, #13086, #38081, .T. ) ;
#33612 = VECTOR ( 'NONE', #44087, 999.9999999999998863 ) ;
#33613 = LINE ( 'NONE', #12344, #24180 ) ;
#33614 = CARTESIAN_POINT ( 'NONE',  ( -13.73672976910459909, 0.000000000000000000, 12.22661844811216270 ) ) ;
#33615 = ORIENTED_EDGE ( 'NONE', *, *, #21775, .T. ) ;
#33616 = CARTESIAN_POINT ( 'NONE',  ( -68.85940620956198188, -10.75105392561086859, 7.491856536230701025 ) ) ;
#33617 = DIRECTION ( 'NONE',  ( -0.9999697198139514409, -0.000000000000000000, -0.007781995580013368816 ) ) ;
#33618 = LINE ( 'NONE', #25390, #2124 ) ;
#33619 = ORIENTED_EDGE ( 'NONE', *, *, #10794, .T. ) ;
#33620 = CARTESIAN_POINT ( 'NONE',  ( -20.54049170961573267, 0.000000000000000000, 4.660556269540326646 ) ) ;
#33621 = VERTEX_POINT ( 'NONE', #8004 ) ;
#33622 = ORIENTED_EDGE ( 'NONE', *, *, #54362, .T. ) ;
#33623 = ORIENTED_EDGE ( 'NONE', *, *, #46376, .F. ) ;
#33624 = EDGE_LOOP ( 'NONE', ( #3527, #44408, #7665, #15967 ) ) ;
#33625 = DIRECTION ( 'NONE',  ( -0.005002170337468016433, -0.7660444431189770143, 0.6427681459581293666 ) ) ;
#33626 = ORIENTED_EDGE ( 'NONE', *, *, #48172, .F. ) ;
#33627 = CARTESIAN_POINT ( 'NONE',  ( -14.73683979275883438, 2.391131607591508335, 2.329931154953872152 ) ) ;
#33628 = VECTOR ( 'NONE', #23760, 999.9999999999998863 ) ;
#33629 = VERTEX_POINT ( 'NONE', #50849 ) ;
#33630 = DIRECTION ( 'NONE',  ( 0.007781995580012663651, 0.000000000000000000, -0.9999697198139515519 ) ) ;
#33631 = EDGE_CURVE ( 'NONE', #55501, #2328, #51139, .T. ) ;
#33632 = ORIENTED_EDGE ( 'NONE', *, *, #17604, .F. ) ;
#33633 = ORIENTED_EDGE ( 'NONE', *, *, #24229, .T. ) ;
#33634 = LINE ( 'NONE', #20011, #1271 ) ;
#33635 = FACE_OUTER_BOUND ( 'NONE', #17407, .T. ) ;
#33636 = CARTESIAN_POINT ( 'NONE',  ( -12.09298204768809626, 0.000000000000000000, 5.834292952445442992 ) ) ;
#33637 = DIRECTION ( 'NONE',  ( 0.000000000000000000, -1.000000000000000000, 0.000000000000000000 ) ) ;
#33638 = FACE_OUTER_BOUND ( 'NONE', #51912, .T. ) ;
#33639 = ORIENTED_EDGE ( 'NONE', *, *, #28219, .T. ) ;
#33640 = EDGE_CURVE ( 'NONE', #15599, #25201, #20766, .T. ) ;
#33641 = ORIENTED_EDGE ( 'NONE', *, *, #29100, .F. ) ;
#33642 = VECTOR ( 'NONE', #38965, 1000.000000000000227 ) ;
#33643 = CARTESIAN_POINT ( 'NONE',  ( -14.38935462099992080, 0.000000000000000000, 2.370940423672420305 ) ) ;
#33644 = DIRECTION ( 'NONE',  ( 0.3313982828793700097, 0.4028455766673915694, 0.8531650599175529814 ) ) ;
#33645 = UNCERTAINTY_MEASURE_WITH_UNIT (LENGTH_MEASURE( 1.000000000000000082E-05 ), #27242, 'distance_accuracy_value', 'NONE');
#33646 = EDGE_CURVE ( 'NONE', #19155, #53854, #28740, .T. ) ;
#33647 = EDGE_CURVE ( 'NONE', #35388, #24636, #12250, .T. ) ;
#33648 = VECTOR ( 'NONE', #11870, 1000.000000000000227 ) ;
#33649 = CARTESIAN_POINT ( 'NONE',  ( -12.80458192191714595, 0.000000000000000000, 11.86454056839041726 ) ) ;
#33650 = PLANE ( 'NONE',  #43178 ) ;
#33651 = PLANE ( 'NONE',  #29475 ) ;
#33652 = DIRECTION ( 'NONE',  ( 0.5449076811759707706, 0.6444004775717708799, -0.5364919789714476250 ) ) ;
#33653 = ORIENTED_EDGE ( 'NONE', *, *, #51352, .F. ) ;
#33654 = DIRECTION ( 'NONE',  ( 0.005961354470445682716, -0.6427876096865404731, -0.7660212471507180654 ) ) ;
#33655 = EDGE_CURVE ( 'NONE', #15174, #22670, #16221, .T. ) ;
#33656 = CARTESIAN_POINT ( 'NONE',  ( -28.92982233430281980, 0.000000000000000000, 7.919257187036034651 ) ) ;
#33657 = EDGE_LOOP ( 'NONE', ( #26608, #52276, #13721 ) ) ;
#33658 = LINE ( 'NONE', #20320, #13466 ) ;
#33659 = DIRECTION ( 'NONE',  ( 0.007781995580012662783, 0.000000000000000000, -0.9999697198139514409 ) ) ;
#33660 = EDGE_CURVE ( 'NONE', #6407, #35835, #36988, .T. ) ;
#33661 = DIRECTION ( 'NONE',  ( -0.9999697198139514409, -0.000000000000000000, -0.007781995580013368816 ) ) ;
#33662 = DIRECTION ( 'NONE',  ( 0.9999697198139515519, 0.000000000000000000, 0.007781995580013368816 ) ) ;
#33663 = ADVANCED_FACE ( 'NONE', ( #29276 ), #11947, .F. ) ;
#33664 = LINE ( 'NONE', #42485, #25968 ) ;
#33665 = ORIENTED_EDGE ( 'NONE', *, *, #8488, .T. ) ;
#33666 =( BOUNDED_CURVE ( )  B_SPLINE_CURVE ( 3, ( #42336, #26136, #16203, #7684 ),
 .UNSPECIFIED., .F., .F. ) 
 B_SPLINE_CURVE_WITH_KNOTS ( ( 4, 4 ),
 ( 2.737789607505189515, 3.545395699674396717 ),
 .UNSPECIFIED. ) 
 CURVE ( )  GEOMETRIC_REPRESENTATION_ITEM ( )  RATIONAL_B_SPLINE_CURVE ( ( 1.000000000000000000, 0.9463822406352063732, 0.9463822406352063732, 1.000000000000000000 ) ) 
 REPRESENTATION_ITEM ( '' )  );
#33667 = ORIENTED_EDGE ( 'NONE', *, *, #44883, .T. ) ;
#33668 = CARTESIAN_POINT ( 'NONE',  ( -12.55995100094445505, -3.917936722690662954, 1.635029929575186891 ) ) ;
#33669 = CARTESIAN_POINT ( 'NONE',  ( -20.43612818448172419, 20.85947173737672955, 4.315991441970404630 ) ) ;
#33670 = DIRECTION ( 'NONE',  ( -0.9999697198139514409, -0.000000000000000000, -0.007781995580013368816 ) ) ;
#33671 = ADVANCED_FACE ( 'NONE', ( #54284 ), #46302, .F. ) ;
#33672 = VECTOR ( 'NONE', #22999, 1000.000000000000114 ) ;
#33673 = VECTOR ( 'NONE', #11008, 999.9999999999998863 ) ;
#33674 = LINE ( 'NONE', #11813, #34603 ) ;
#33675 = CARTESIAN_POINT ( 'NONE',  ( -14.00280974873554030, 0.000000000000000000, 12.40921378708904044 ) ) ;
#33676 = CARTESIAN_POINT ( 'NONE',  ( -23.33849165029409889, 0.000000000000000000, 5.946783852668351855 ) ) ;
#33677 = FACE_OUTER_BOUND ( 'NONE', #46849, .T. ) ;
#33678 = EDGE_CURVE ( 'NONE', #15181, #25884, #50005, .T. ) ;
#33679 = B_SPLINE_CURVE_WITH_KNOTS ( 'NONE', 3,
 ( #55315, #16410, #30051, #47085, #47356, #33734, #52195, #8466, #4496, #20949, #4233, #21803, #12161, #17003, #42550, #29496, #46816, #38862, #16707, #34037, #25795, #14428, #18961, #1634, #36278, #39421, #39710, #32007, #23227, #5604 ),
 .UNSPECIFIED., .F., .F.,
 ( 4, 1, 1, 1, 1, 1, 1, 1, 1, 1, 1, 2, 2, 1, 1, 1, 1, 1, 1, 1, 1, 2, 2, 4 ),
 ( 0.000000000000000000, 0.1249999999997620792, 0.1874999999996430633, 0.2187499999995836386, 0.2343749999995539124, 0.2421874999995391464, 0.2460937499995317357, 0.2480468749995280442, 0.2490234374995262401, 0.2495117187495253241, 0.2497558593745249633, 0.2498779296870247690, 0.2499999999995246025, 0.3749999999996284084, 0.4374999999996804223, 0.4687499999997064570, 0.4843749999997194466, 0.4921874999997258859, 0.4960937499997292166, 0.4980468749997308819, 0.4990234374997316591, 0.4995117187497319922, 0.4999999999997323252, 1.000000000000000000 ),
 .UNSPECIFIED. ) ;
#33680 = CARTESIAN_POINT ( 'NONE',  ( -9.030577898858158647, 0.000000000000000000, 4.580803066637238352 ) ) ;
#33681 = CARTESIAN_POINT ( 'NONE',  ( -67.96727558581105200, -9.488692052113647080, -7.038790429923468039 ) ) ;
#33682 = CARTESIAN_POINT ( 'NONE',  ( -17.00562625101985503, -3.108426967578162170, 3.387708771908411354 ) ) ;
#33683 = VERTEX_POINT ( 'NONE', #20183 ) ;
#33684 = CARTESIAN_POINT ( 'NONE',  ( -17.26532721389163072, 0.000000000000000000, 13.67648636611514590 ) ) ;
#33685 = VERTEX_POINT ( 'NONE', #2599 ) ;
#33686 = ORIENTED_EDGE ( 'NONE', *, *, #24192, .F. ) ;
#33687 = VECTOR ( 'NONE', #20729, 999.9999999999998863 ) ;
#33688 = VERTEX_POINT ( 'NONE', #11113 ) ;
#33689 = EDGE_LOOP ( 'NONE', ( #16979, #36502, #56032, #51906 ) ) ;
#33690 = ORIENTED_EDGE ( 'NONE', *, *, #4572, .T. ) ;
#33691 = EDGE_LOOP ( 'NONE', ( #8007, #16590, #52682, #32169 ) ) ;
#33692 = LINE ( 'NONE', #7892, #15139 ) ;
#33693 = DIRECTION ( 'NONE',  ( 0.7660212471507180654, -0.6427876096865404731, 0.005961354470445141482 ) ) ;
#33694 = LINE ( 'NONE', #24908, #47540 ) ;
#33695 = ORIENTED_EDGE ( 'NONE', *, *, #50821, .T. ) ;
#33696 = DIRECTION ( 'NONE',  ( -0.7660212471507179544, -0.6427876096865405842, -0.005961354470445141482 ) ) ;
#33697 = EDGE_CURVE ( 'NONE', #6551, #55548, #45756, .T. ) ;
#33698 = ORIENTED_EDGE ( 'NONE', *, *, #37443, .T. ) ;
#33699 = LINE ( 'NONE', #3880, #55809 ) ;
#33700 = ORIENTED_EDGE ( 'NONE', *, *, #37372, .T. ) ;
#33701 = CARTESIAN_POINT ( 'NONE',  ( -65.15079379074605015, -9.165714244539783451, 1.521991683921744887 ) ) ;
#33702 = CARTESIAN_POINT ( 'NONE',  ( -17.85999659322806821, 0.000000000000000000, 4.681416502340032260 ) ) ;
#33703 = CARTESIAN_POINT ( 'NONE',  ( -69.15027346225275551, -10.43622021222418716, -7.497281464624098390 ) ) ;
#33704 = EDGE_LOOP ( 'NONE', ( #53360, #39019, #3590, #35321 ) ) ;
#33705 = LINE ( 'NONE', #55569, #53669 ) ;
#33706 = VERTEX_POINT ( 'NONE', #19915 ) ;
#33707 = AXIS2_PLACEMENT_3D ( 'NONE', #18965, #10978, #28037 ) ;
#33708 = CIRCLE ( 'NONE', #23746, 2.000000000000002220 ) ;
#33709 = CARTESIAN_POINT ( 'NONE',  ( -15.96710241509184058, -0.1191753592594218814, 13.13259134697452879 ) ) ;
#33710 = CARTESIAN_POINT ( 'NONE',  ( -10.94028622754223967, 0.000000000000000000, 11.14038480894692995 ) ) ;
#33711 = ADVANCED_FACE ( 'NONE', ( #15644 ), #32986, .F. ) ;
#33712 = LINE ( 'NONE', #21221, #7921 ) ;
#33713 = VECTOR ( 'NONE', #8711, 1000.000000000000114 ) ;
#33714 = DIRECTION ( 'NONE',  ( 0.007781995580012662783, 0.000000000000000000, -0.9999697198139514409 ) ) ;
#33715 = PLANE ( 'NONE',  #23835 ) ;
#33716 = DIRECTION ( 'NONE',  ( 0.007781995580012662783, 0.000000000000000000, -0.9999697198139514409 ) ) ;
#33717 = DIRECTION ( 'NONE',  ( -0.5449076811759708816, 0.6444004775717707689, 0.5364919789714475140 ) ) ;
#33718 = CARTESIAN_POINT ( 'NONE',  ( -67.08386678843554307, -11.40049507478859603, -4.138470222184133185 ) ) ;
#33719 = ORIENTED_EDGE ( 'NONE', *, *, #29656, .F. ) ;
#33720 = FACE_OUTER_BOUND ( 'NONE', #20007, .T. ) ;
#33721 = ORIENTED_EDGE ( 'NONE', *, *, #32138, .T. ) ;
#33722 = CARTESIAN_POINT ( 'NONE',  ( -16.53317331066696383, 0.000000000000000000, 13.31285208727739899 ) ) ;
#33723 = LINE ( 'NONE', #37420, #24197 ) ;
#33724 = ADVANCED_FACE ( 'NONE', ( #41761 ), #15950, .F. ) ;
#33725 = PLANE ( 'NONE',  #13262 ) ;
#33726 = CIRCLE ( 'NONE', #6536, 2.749999999999998224 ) ;
#33727 = DIRECTION ( 'NONE',  ( 0.007781995580012663651, -3.146120232559066537E-19, -0.9999697198139514409 ) ) ;
#33728 = CARTESIAN_POINT ( 'NONE',  ( -16.56099755347650770, -4.241740624735664156, 3.178841246916717100 ) ) ;
#33729 = VECTOR ( 'NONE', #2496, 1000.000000000000114 ) ;
#33730 = EDGE_CURVE ( 'NONE', #4731, #98, #4846, .T. ) ;
#33731 = CARTESIAN_POINT ( 'NONE',  ( 0.000000000000000000, 2.000000000000000000, 0.000000000000000000 ) ) ;
#33732 = ORIENTED_EDGE ( 'NONE', *, *, #51269, .T. ) ;
#33733 = CARTESIAN_POINT ( 'NONE',  ( -18.61196750743211936, -0.03228989815065406305, 4.109811145338044369 ) ) ;
#33734 = CARTESIAN_POINT ( 'NONE',  ( -18.47181751008412220, 20.26151622644335148, 4.232279298899151776 ) ) ;
#33735 = LINE ( 'NONE', #47086, #16750 ) ;
#33736 = DIRECTION ( 'NONE',  ( -0.005961354470445682716, -0.6427876096865404731, 0.7660212471507180654 ) ) ;
#33737 = ADVANCED_FACE ( 'NONE', ( #13092 ), #43732, .F. ) ;
#33738 = DIRECTION ( 'NONE',  ( -0.5364919789714478471, 0.6444004775717705469, -0.5449076811759709926 ) ) ;
#33739 = LINE ( 'NONE', #3643, #51102 ) ;
#33740 = LINE ( 'NONE', #30642, #19582 ) ;
#33741 = DIRECTION ( 'NONE',  ( 0.000000000000000000, 0.000000000000000000, 1.000000000000000000 ) ) ;
#33742 = ORIENTED_EDGE ( 'NONE', *, *, #48440, .F. ) ;
#33743 = EDGE_CURVE ( 'NONE', #42918, #15204, #30424, .T. ) ;
#33744 = FACE_OUTER_BOUND ( 'NONE', #30871, .T. ) ;
#33745 = CARTESIAN_POINT ( 'NONE',  ( -24.26908309836554878, 0.000000000000000000, 6.108867788427308376 ) ) ;
#33746 = ORIENTED_EDGE ( 'NONE', *, *, #39119, .F. ) ;
#33747 = VECTOR ( 'NONE', #40019, 999.9999999999998863 ) ;
#33748 = ORIENTED_EDGE ( 'NONE', *, *, #21447, .F. ) ;
#33749 = PLANE ( 'NONE',  #10166 ) ;
#33750 = VECTOR ( 'NONE', #47817, 1000.000000000000227 ) ;
#33751 = VECTOR ( 'NONE', #3973, 1000.000000000000114 ) ;
#33752 = ORIENTED_EDGE ( 'NONE', *, *, #27440, .T. ) ;
#33753 = DIRECTION ( 'NONE',  ( -0.7660212471507179544, -0.6427876096865405842, -0.005961354470445141482 ) ) ;
#33754 = VECTOR ( 'NONE', #5615, 1000.000000000000114 ) ;
#33755 = VERTEX_POINT ( 'NONE', #26159 ) ;
#33756 = ORIENTED_EDGE ( 'NONE', *, *, #6022, .F. ) ;
#33757 = VECTOR ( 'NONE', #1733, 999.9999999999998863 ) ;
#33758 = ORIENTED_EDGE ( 'NONE', *, *, #41386, .T. ) ;
#33759 = DIRECTION ( 'NONE',  ( -0.9999697198139514409, -0.000000000000000000, -0.007781995580013368816 ) ) ;
#33760 = CARTESIAN_POINT ( 'NONE',  ( -65.16688019966139223, -9.167558940675322177, 1.648866456817433823 ) ) ;
#33761 = DIRECTION ( 'NONE',  ( 0.007781995580012663651, -3.146120232559066537E-19, -0.9999697198139514409 ) ) ;
#33762 = EDGE_CURVE ( 'NONE', #54772, #48743, #34967, .T. ) ;
#33763 = ORIENTED_EDGE ( 'NONE', *, *, #18990, .F. ) ;
#33764 = VECTOR ( 'NONE', #104, 999.9999999999998863 ) ;
#33766 = ORIENTED_EDGE ( 'NONE', *, *, #8320, .F. ) ;
#33765 = ADVANCED_FACE ( 'NONE', ( #286 ), #22169, .F. ) ;
#33767 = ADVANCED_FACE ( 'NONE', ( #21031 ), #51698, .F. ) ;
#33768 = FACE_OUTER_BOUND ( 'NONE', #13360, .T. ) ;
#33769 = LINE ( 'NONE', #3954, #40893 ) ;
#33771 = ADVANCED_FACE ( 'NONE', ( #4009 ), #4311, .F. ) ;
#33770 = ORIENTED_EDGE ( 'NONE', *, *, #40358, .F. ) ;
#33772 = FACE_OUTER_BOUND ( 'NONE', #6547, .T. ) ;
#33773 = CARTESIAN_POINT ( 'NONE',  ( -28.93060053386082231, -0.1191753592594197858, 8.019254159017428663 ) ) ;
#33774 = ORIENTED_EDGE ( 'NONE', *, *, #20069, .F. ) ;
#33775 = LINE ( 'NONE', #33508, #55701 ) ;
#33776 = DIRECTION ( 'NONE',  ( 0.5364919789714477361, 0.6444004775717706579, 0.5449076811759711036 ) ) ;
#33777 = ADVANCED_FACE ( 'NONE', ( #13392 ), #34656, .F. ) ;
#33778 = ADVANCED_FACE ( 'NONE', ( #51977 ), #12803, .F. ) ;
#33779 = EDGE_CURVE ( 'NONE', #45468, #19093, #26413, .T. ) ;
#33780 = ORIENTED_EDGE ( 'NONE', *, *, #9277, .F. ) ;
#33781 = LINE ( 'NONE', #32946, #33150 ) ;
#33782 = VECTOR ( 'NONE', #24647, 1000.000000000000227 ) ;
#33783 = CARTESIAN_POINT ( 'NONE',  ( -20.65957321758616416, 2.229229656569007734, 4.635687473917941226 ) ) ;
#33784 = ORIENTED_EDGE ( 'NONE', *, *, #20249, .F. ) ;
#33785 = DIRECTION ( 'NONE',  ( -0.6427681459581293666, -0.7660444431189770143, -0.005002170337467561935 ) ) ;
#33786 = PLANE ( 'NONE',  #7505 ) ;
#33787 = LINE ( 'NONE', #51414, #20293 ) ;
#33788 = VECTOR ( 'NONE', #41522, 1000.000000000000227 ) ;
#33789 = CARTESIAN_POINT ( 'NONE',  ( -15.47117689834755261, -2.946525016555661125, 2.796842053098518743 ) ) ;
#33790 = EDGE_LOOP ( 'NONE', ( #3537, #20549, #341, #9578 ) ) ;
#33791 = AXIS2_PLACEMENT_3D ( 'NONE', #45097, #5611, #6201 ) ;
#33792 = VECTOR ( 'NONE', #26016, 1000.000000000000227 ) ;
#33793 = LINE ( 'NONE', #12219, #18317 ) ;
#33794 = CARTESIAN_POINT ( 'NONE',  ( -46.52156441860571334, 5.799038105676371124, -5.000000000000000000 ) ) ;
#33795 = DIRECTION ( 'NONE',  ( -0.005961354470445682716, -0.6427876096865404731, 0.7660212471507180654 ) ) ;
#33796 = EDGE_CURVE ( 'NONE', #36235, #18922, #12543, .T. ) ;
#33797 = CARTESIAN_POINT ( 'NONE',  ( -16.06709938707323460, 0.000000000000000000, 13.13181314741652628 ) ) ;
#33798 = DIRECTION ( 'NONE',  ( -0.005002170337468016433, -0.7660444431189770143, 0.6427681459581293666 ) ) ;
#33799 = CARTESIAN_POINT ( 'NONE',  ( -15.60102546347950536, 0.000000000000000000, 12.95077420755565356 ) ) ;
#33800 = EDGE_CURVE ( 'NONE', #32412, #47173, #51443, .T. ) ;
#33801 = VECTOR ( 'NONE', #27333, 999.9999999999998863 ) ;
#33802 = LINE ( 'NONE', #42601, #51226 ) ;
#33803 = AXIS2_PLACEMENT_3D ( 'NONE', #46215, #15555, #33193 ) ;
#33804 = ORIENTED_EDGE ( 'NONE', *, *, #54330, .T. ) ;
#33805 =( NAMED_UNIT ( * ) PLANE_ANGLE_UNIT ( ) SI_UNIT ( $, .RADIAN. ) );
#33806 = ADVANCED_FACE ( 'NONE', ( #8259 ), #21334, .F. ) ;
#33807 = CARTESIAN_POINT ( 'NONE',  ( -68.69950585158439083, -0.6013238516280168255, 6.175865180864700044 ) ) ;
#33808 = ORIENTED_EDGE ( 'NONE', *, *, #4520, .F. ) ;
#33809 = CARTESIAN_POINT ( 'NONE',  ( -21.84967550273626102, 5.305366725996514710, 4.999818739653546729 ) ) ;
#33810 = FACE_OUTER_BOUND ( 'NONE', #21883, .T. ) ;
#33811 = EDGE_CURVE ( 'NONE', #48202, #16580, #7915, .T. ) ;
#33812 = FACE_OUTER_BOUND ( 'NONE', #41566, .T. ) ;
#33813 = VECTOR ( 'NONE', #40297, 999.9999999999998863 ) ;
#33814 = VECTOR ( 'NONE', #36500, 999.9999999999998863 ) ;
#33815 = CARTESIAN_POINT ( 'NONE',  ( -15.88130887279446490, 0.000000000000000000, 3.050160814894388839 ) ) ;
#33816 = DIRECTION ( 'NONE',  ( -0.000000000000000000, -0.000000000000000000, -1.000000000000000000 ) ) ;
#33817 = VERTEX_POINT ( 'NONE', #15550 ) ;
#33818 = EDGE_LOOP ( 'NONE', ( #2836, #26416, #40224, #30224 ) ) ;
#33819 = CARTESIAN_POINT ( 'NONE',  ( -25.20123094555300369, 0.000000000000000000, 6.470945668149052032 ) ) ;
#33820 = FACE_OUTER_BOUND ( 'NONE', #737, .T. ) ;
#33821 = ORIENTED_EDGE ( 'NONE', *, *, #11219, .F. ) ;
#33822 = AXIS2_PLACEMENT_3D ( 'NONE', #52771, #46633, #22435 ) ;
#33823 = DIRECTION ( 'NONE',  ( 0.2113248654051873565, 0.7886751345948121994, -0.5773502691896263972 ) ) ;
#33824 = ORIENTED_EDGE ( 'NONE', *, *, #22370, .T. ) ;
#33825 = DIRECTION ( 'NONE',  ( 0.007781995580012663651, -3.146120232559066537E-19, -0.9999697198139514409 ) ) ;
#33826 = AXIS2_PLACEMENT_3D ( 'NONE', #9446, #14547, #35866 ) ;
#33827 = ORIENTED_EDGE ( 'NONE', *, *, #33598, .F. ) ;
#33828 = LINE ( 'NONE', #16498, #51940 ) ;
#33829 = ORIENTED_EDGE ( 'NONE', *, *, #46405, .T. ) ;
#33830 = ORIENTED_EDGE ( 'NONE', *, *, #14377, .T. ) ;
#33831 = ORIENTED_EDGE ( 'NONE', *, *, #37169, .F. ) ;
#33832 = CARTESIAN_POINT ( 'NONE',  ( -11.87243407472968926, 0.000000000000000000, 11.50246268866867361 ) ) ;
#33833 = VECTOR ( 'NONE', #38942, 999.9999999999998863 ) ;
#33834 = LINE ( 'NONE', #51152, #24130 ) ;
#33835 = CARTESIAN_POINT ( 'NONE',  ( -19.05259568539925752, 0.000000000000000000, 4.502809406857032570 ) ) ;
#33836 = VECTOR ( 'NONE', #15298, 1000.000000000000227 ) ;
#33837 = VECTOR ( 'NONE', #28213, 1000.000000000000227 ) ;
#33838 = CARTESIAN_POINT ( 'NONE',  ( -21.47263955680318404, 0.000000000000000000, 5.022634149262071190 ) ) ;
#33839 = ORIENTED_EDGE ( 'NONE', *, *, #46279, .F. ) ;
#33840 = ORIENTED_EDGE ( 'NONE', *, *, #14552, .F. ) ;
#33841 = VECTOR ( 'NONE', #23912, 1000.000000000000227 ) ;
#33842 = ORIENTED_EDGE ( 'NONE', *, *, #53130, .T. ) ;
#33843 = FACE_OUTER_BOUND ( 'NONE', #37069, .T. ) ;
#33844 = AXIS2_PLACEMENT_3D ( 'NONE', #26211, #347, #9152 ) ;
#33845 = DIRECTION ( 'NONE',  ( -0.9999697198139514409, -0.000000000000000000, -0.007781995580013368816 ) ) ;
#33846 = ORIENTED_EDGE ( 'NONE', *, *, #29779, .F. ) ;
#33847 = DIRECTION ( 'NONE',  ( 0.3583679495452925523, 0.9335804264972047406, 0.000000000000000000 ) ) ;
#33848 = ORIENTED_EDGE ( 'NONE', *, *, #55848, .T. ) ;
#33849 = DIRECTION ( 'NONE',  ( -0.2588190451025176864, -0.9659258262890692004, 0.000000000000000000 ) ) ;
#33850 = FACE_OUTER_BOUND ( 'NONE', #37765, .T. ) ;
#33851 = EDGE_CURVE ( 'NONE', #42922, #45468, #41947, .T. ) ;
#33852 = EDGE_CURVE ( 'NONE', #12574, #30915, #29479, .T. ) ;
#33853 = ORIENTED_EDGE ( 'NONE', *, *, #41459, .T. ) ;
#33854 = LINE ( 'NONE', #24230, #17756 ) ;
#33855 = EDGE_LOOP ( 'NONE', ( #42561, #45993, #41563, #6003 ) ) ;
#33856 = ADVANCED_FACE ( 'NONE', ( #3626 ), #20931, .F. ) ;
#33857 = VECTOR ( 'NONE', #25141, 999.9999999999998863 ) ;
#33858 = DIRECTION ( 'NONE',  ( 0.000000000000000000, -0.000000000000000000, -1.000000000000000000 ) ) ;
#33859 = DIRECTION ( 'NONE',  ( -0.9999697198139514409, -0.000000000000000000, -0.007781995580013368816 ) ) ;
#33860 = ORIENTED_EDGE ( 'NONE', *, *, #26125, .T. ) ;
#33861 = LINE ( 'NONE', #33575, #49535 ) ;
#33862 = DIRECTION ( 'NONE',  ( -0.5449076811759708816, 0.6444004775717707689, 0.5364919789714475140 ) ) ;
#33863 = CARTESIAN_POINT ( 'NONE',  ( -27.99767448711536133, 0.000000000000000000, 7.557179307314289218 ) ) ;
#33864 = DIRECTION ( 'NONE',  ( 0.007781995580012662783, 0.000000000000000000, -0.9999697198139514409 ) ) ;
#33865 = VERTEX_POINT ( 'NONE', #54734 ) ;
#33866 = VECTOR ( 'NONE', #24486, 1000.000000000000227 ) ;
#33867 = ORIENTED_EDGE ( 'NONE', *, *, #38870, .F. ) ;
#33868 = DIRECTION ( 'NONE',  ( 0.007781995580012662783, 0.000000000000000000, -0.9999697198139514409 ) ) ;
#33869 = CARTESIAN_POINT ( 'NONE',  ( -19.59569683186026268, 0.000000000000000000, 14.58168106541950948 ) ) ;
#33870 = VECTOR ( 'NONE', #26484, 1000.000000000000114 ) ;
#33871 = DIRECTION ( 'NONE',  ( -0.5449076811759708816, 0.6444004775717707689, 0.5364919789714475140 ) ) ;
#33872 = CARTESIAN_POINT ( 'NONE',  ( -11.30636317915456779, -0.1191753592594197858, 11.32220194836580340 ) ) ;
#33874 = EDGE_CURVE ( 'NONE', #13391, #40480, #12456, .T. ) ;
#33873 = FACE_OUTER_BOUND ( 'NONE', #44944, .T. ) ;
#33875 = PLANE ( 'NONE',  #33114 ) ;
#33876 = VERTEX_POINT ( 'NONE', #38256 ) ;
#33877 = LINE ( 'NONE', #29649, #14128 ) ;
#33878 = EDGE_CURVE ( 'NONE', #14582, #2799, #33453, .T. ) ;
#33879 = DIRECTION ( 'NONE',  ( 0.7660212471507180654, -0.6427876096865404731, 0.005961354470445141482 ) ) ;
#33880 = ORIENTED_EDGE ( 'NONE', *, *, #37258, .F. ) ;
#33881 = VECTOR ( 'NONE', #8342, 1000.000000000000227 ) ;
#33882 = LINE ( 'NONE', #51202, #23186 ) ;
#33883 = ORIENTED_EDGE ( 'NONE', *, *, #24107, .T. ) ;
#33884 = MECHANICAL_DESIGN_GEOMETRIC_PRESENTATION_REPRESENTATION (  '', ( #19357 ), #39317 ) ;
#33885 = AXIS2_PLACEMENT_3D ( 'NONE', #4664, #43833, #47843 ) ;
#33886 = DIRECTION ( 'NONE',  ( -0.005961354470445682716, -0.6427876096865404731, 0.7660212471507180654 ) ) ;
#33887 = CARTESIAN_POINT ( 'NONE',  ( -9.342070512798265725, 0.000000000000000000, 10.59882438848031505 ) ) ;
#33888 = EDGE_CURVE ( 'NONE', #50295, #30246, #3899, .T. ) ;
#33889 = DIRECTION ( 'NONE',  ( 0.9999697198139515519, 0.000000000000000000, 0.007781995580013368816 ) ) ;
#33890 = CARTESIAN_POINT ( 'NONE',  ( -23.33849165029409889, 0.000000000000000000, 5.946783852668351855 ) ) ;
#33891 = EDGE_CURVE ( 'NONE', #43988, #43441, #24936, .T. ) ;
#33892 = CARTESIAN_POINT ( 'NONE',  ( -69.85628739008400601, 2.000000000006432632, -7.520604412859268173 ) ) ;
#33893 = VERTEX_POINT ( 'NONE', #16391 ) ;
#33894 = AXIS2_PLACEMENT_3D ( 'NONE', #32085, #24387, #2782 ) ;
#33895 = VECTOR ( 'NONE', #29194, 999.9999999999998863 ) ;
#33896 = VERTEX_POINT ( 'NONE', #47072 ) ;
#33897 = CARTESIAN_POINT ( 'NONE',  ( -22.40478740399063895, 0.000000000000000000, 5.384712028983816623 ) ) ;
#33898 = FACE_OUTER_BOUND ( 'NONE', #7719, .T. ) ;
#33899 = DIRECTION ( 'NONE',  ( 0.007781995580012663651, -3.146120232559066537E-19, -0.9999697198139514409 ) ) ;
#33900 = CARTESIAN_POINT ( 'NONE',  ( -20.00186950356889426, -0.008498251296377924008, 6.149207326778157956 ) ) ;
#33901 = DIRECTION ( 'NONE',  ( 0.5449076811759707706, 0.6444004775717708799, -0.5364919789714476250 ) ) ;
#33902 = DIRECTION ( 'NONE',  ( 0.007781995580012663651, 0.000000000000000000, -0.9999697198139515519 ) ) ;
#33903 = ORIENTED_EDGE ( 'NONE', *, *, #51997, .T. ) ;
#33904 = CARTESIAN_POINT ( 'NONE',  ( -10.94028622754223967, 0.000000000000000000, 11.14038480894692995 ) ) ;
#33905 = DIRECTION ( 'NONE',  ( 0.000000000000000000, -0.000000000000000000, -1.000000000000000000 ) ) ;
#33906 = DIRECTION ( 'NONE',  ( 0.6427681459581294776, -0.7660444431189769032, 0.005002170337467562802 ) ) ;
#33907 = ORIENTED_EDGE ( 'NONE', *, *, #17717, .F. ) ;
#33908 = VECTOR ( 'NONE', #15154, 1000.000000000000227 ) ;
#33909 = LINE ( 'NONE', #7229, #41060 ) ;
#33910 = DIRECTION ( 'NONE',  ( 0.000000000000000000, -0.000000000000000000, -1.000000000000000000 ) ) ;
#33911 = VECTOR ( 'NONE', #28631, 999.9999999999998863 ) ;
#33912 = LINE ( 'NONE', #29684, #19356 ) ;
#33913 = VERTEX_POINT ( 'NONE', #50198 ) ;
#33914 = DIRECTION ( 'NONE',  ( 0.5449076811759707706, 0.6444004775717708799, -0.5364919789714476250 ) ) ;
#33915 = AXIS2_PLACEMENT_3D ( 'NONE', #2760, #20085, #11598 ) ;
#33916 = VERTEX_POINT ( 'NONE', #3052 ) ;
#33917 = ORIENTED_EDGE ( 'NONE', *, *, #14467, .F. ) ;
#33918 = ORIENTED_EDGE ( 'NONE', *, *, #9104, .F. ) ;
#33919 = EDGE_LOOP ( 'NONE', ( #26248, #14465, #27338, #47251 ) ) ;
#33920 = VECTOR ( 'NONE', #46915, 1000.000000000000227 ) ;
#33921 = PLANE ( 'NONE',  #37500 ) ;
#33922 = ORIENTED_EDGE ( 'NONE', *, *, #13363, .T. ) ;
#33923 = FACE_OUTER_BOUND ( 'NONE', #43360, .T. ) ;
#33924 = PRESENTATION_LAYER_ASSIGNMENT (  '', '', ( #43002 ) ) ;
#33925 = ADVANCED_FACE ( 'NONE', ( #33186 ), #25485, .F. ) ;
#33926 = VERTEX_POINT ( 'NONE', #29774 ) ;
#33927 = CARTESIAN_POINT ( 'NONE',  ( -12.15929124516513227, -0.1191753592594198830, 1.504708075227162656 ) ) ;
#33928 = ORIENTED_EDGE ( 'NONE', *, *, #54801, .F. ) ;
#33929 = ORIENTED_EDGE ( 'NONE', *, *, #10071, .T. ) ;
#33930 = EDGE_CURVE ( 'NONE', #19674, #34361, #8177, .T. ) ;
#33931 = EDGE_CURVE ( 'NONE', #42035, #3660, #20682, .T. ) ;
#33932 = AXIS2_PLACEMENT_3D ( 'NONE', #37951, #25439, #21178 ) ;
#33933 = VECTOR ( 'NONE', #20040, 1000.000000000000000 ) ;
#33934 = CARTESIAN_POINT ( 'NONE',  ( -19.25577499705407902, 1.095915999411505082, 6.159502914972740939 ) ) ;
#33935 = LINE ( 'NONE', #4667, #3272 ) ;
#33936 = FACE_OUTER_BOUND ( 'NONE', #10937, .T. ) ;
#33937 = CARTESIAN_POINT ( 'NONE',  ( -14.39760455647254744, 0.000000000000000000, 3.431039414763832340 ) ) ;
#33938 = DIRECTION ( 'NONE',  ( -0.7660212471507179544, -0.6427876096865405842, -0.005961354470445141482 ) ) ;
#33939 = ORIENTED_EDGE ( 'NONE', *, *, #20276, .T. ) ;
#33940 = EDGE_LOOP ( 'NONE', ( #2643, #32871, #50097, #22041 ) ) ;
#33941 = PLANE ( 'NONE',  #47551 ) ;
#33942 = LINE ( 'NONE', #43324, #47529 ) ;
#33943 = FACE_OUTER_BOUND ( 'NONE', #42155, .T. ) ;
#33944 = VECTOR ( 'NONE', #28395, 1000.000000000000114 ) ;
#33945 = LINE ( 'NONE', #51268, #53013 ) ;
#33946 = LINE ( 'NONE', #24030, #50340 ) ;
#33947 = CARTESIAN_POINT ( 'NONE',  ( -15.09384998583453097, 0.000000000000000000, 7.488273839715230196 ) ) ;
#33948 = VERTEX_POINT ( 'NONE', #16689 ) ;
#33949 = CARTESIAN_POINT ( 'NONE',  ( -12.78951571262592068, -1.975113310420658852, 1.786186898291378000 ) ) ;
#33950 = DIRECTION ( 'NONE',  ( -0.7660212471507179544, -0.6427876096865405842, -0.005961354470445141482 ) ) ;
#33951 = AXIS2_PLACEMENT_3D ( 'NONE', #54328, #15421, #29044 ) ;
#33952 = ORIENTED_EDGE ( 'NONE', *, *, #10080, .T. ) ;
#33953 = CARTESIAN_POINT ( 'NONE',  ( -28.92982233430281980, 0.000000000000000000, 7.919257187036034651 ) ) ;
#33954 = CARTESIAN_POINT ( 'NONE',  ( -18.19747506107908563, 0.000000000000000000, 14.03856424583689311 ) ) ;
#33955 = DIRECTION ( 'NONE',  ( -0.7660212471507179544, -0.6427876096865405842, -0.005961354470445141482 ) ) ;
#33956 = LINE ( 'NONE', #56107, #44958 ) ;
#33957 = EDGE_CURVE ( 'NONE', #46531, #21352, #50503, .T. ) ;
#33958 = DIRECTION ( 'NONE',  ( 0.007781995580012663651, -3.146120232559066537E-19, -0.9999697198139514409 ) ) ;
#33959 = VERTEX_POINT ( 'NONE', #42793 ) ;
#33960 = VECTOR ( 'NONE', #5327, 1000.000000000000227 ) ;
#33961 = EDGE_CURVE ( 'NONE', #48671, #31756, #37997, .T. ) ;
#33962 = ORIENTED_EDGE ( 'NONE', *, *, #5655, .T. ) ;
#33963 = VECTOR ( 'NONE', #19528, 999.9999999999998863 ) ;
#33964 = CARTESIAN_POINT ( 'NONE',  ( -17.43427879107165879, 0.000000000000000000, 9.686052500421766354 ) ) ;
#33965 = CARTESIAN_POINT ( 'NONE',  ( -19.77061338776520216, 21.24370688441071664, 4.270755533188014930 ) ) ;
#33966 = DIRECTION ( 'NONE',  ( 0.6427681459581294776, -0.7660444431189769032, 0.005002170337467562802 ) ) ;
#33967 = EDGE_CURVE ( 'NONE', #41210, #51656, #28640, .T. ) ;
#33968 = VECTOR ( 'NONE', #5048, 999.9999999999998863 ) ;
#33969 = DIRECTION ( 'NONE',  ( -0.9999697198139514409, -0.000000000000000000, -0.007781995580013368816 ) ) ;
#33970 = ADVANCED_FACE ( 'NONE', ( #24365 ), #41675, .F. ) ;
#33971 = CARTESIAN_POINT ( 'NONE',  ( -2.881839257824877265, -5.376589517215482950, -2.098969340251471305 ) ) ;
#33972 = LINE ( 'NONE', #3583, #13780 ) ;
#33973 = DIRECTION ( 'NONE',  ( -0.5449076811759708816, 0.6444004775717707689, 0.5364919789714475140 ) ) ;
#33974 = VECTOR ( 'NONE', #19727, 1000.000000000000000 ) ;
#33975 = PLANE ( 'NONE',  #11450 ) ;
#33976 = VECTOR ( 'NONE', #46516, 1000.000000000000227 ) ;
#33977 = CARTESIAN_POINT ( 'NONE',  ( -15.88130887279446490, 0.000000000000000000, 3.050160814894388839 ) ) ;
#33978 = DIRECTION ( 'NONE',  ( -0.3313982828793700097, 0.4028455766673915694, -0.8531650599175529814 ) ) ;
#33979 = ORIENTED_EDGE ( 'NONE', *, *, #45565, .T. ) ;
#33980 = DIRECTION ( 'NONE',  ( 0.000000000000000000, -5.782411586589354681E-16, 1.000000000000000000 ) ) ;
#33981 = EDGE_LOOP ( 'NONE', ( #22237, #46170, #3338, #14962 ) ) ;
#33982 = ORIENTED_EDGE ( 'NONE', *, *, #38926, .F. ) ;
#33983 = ADVANCED_FACE ( 'NONE', ( #37413 ), #28917, .F. ) ;
#33984 = VECTOR ( 'NONE', #28034, 1000.000000000000227 ) ;
#33985 = ORIENTED_EDGE ( 'NONE', *, *, #51672, .T. ) ;
#33986 = ORIENTED_EDGE ( 'NONE', *, *, #3264, .T. ) ;
#33987 = ORIENTED_EDGE ( 'NONE', *, *, #54952, .T. ) ;
#33988 = AXIS2_PLACEMENT_3D ( 'NONE', #43756, #40062, #4872 ) ;
#33989 = ORIENTED_EDGE ( 'NONE', *, *, #37366, .F. ) ;
#33990 = LINE ( 'NONE', #20061, #40522 ) ;
#33991 = DIRECTION ( 'NONE',  ( -0.9999697198139514409, -0.000000000000000000, -0.007781995580013368816 ) ) ;
#33992 = EDGE_CURVE ( 'NONE', #35868, #26894, #30319, .T. ) ;
#33993 = LINE ( 'NONE', #12431, #4940 ) ;
#33994 = AXIS2_PLACEMENT_3D ( 'NONE', #40079, #49156, #44074 ) ;
#33996 = EDGE_CURVE ( 'NONE', #45628, #5924, #34308, .T. ) ;
#33995 = VERTEX_POINT ( 'NONE', #13557 ) ;
#33997 = FACE_OUTER_BOUND ( 'NONE', #54398, .T. ) ;
#33998 = ORIENTED_EDGE ( 'NONE', *, *, #10902, .F. ) ;
#33999 = VECTOR ( 'NONE', #48826, 999.9999999999998863 ) ;
#34000 = DIRECTION ( 'NONE',  ( -0.5449076811759708816, 0.6444004775717707689, 0.5364919789714475140 ) ) ;
#34001 = EDGE_LOOP ( 'NONE', ( #3176, #44598, #37624, #33228 ) ) ;
#34002 = EDGE_CURVE ( 'NONE', #8988, #26117, #26914, .T. ) ;
#34003 = AXIS2_PLACEMENT_3D ( 'NONE', #16592, #16310, #51536 ) ;
#34004 = AXIS2_PLACEMENT_3D ( 'NONE', #38340, #32966, #16769 ) ;
#34005 = CARTESIAN_POINT ( 'NONE',  ( -21.47341775636118655, -0.1191753592594197858, 5.122631121243466090 ) ) ;
#34006 = VECTOR ( 'NONE', #25461, 1000.000000000000227 ) ;
#34007 = CARTESIAN_POINT ( 'NONE',  ( -13.06197087640816434, -2.298917212465660054, 1.881686696745927589 ) ) ;
#34008 = CARTESIAN_POINT ( 'NONE',  ( -9.607175450607181588, -0.1191753592594187727, 2.260320404213849610 ) ) ;
#34009 = ORIENTED_EDGE ( 'NONE', *, *, #22885, .T. ) ;
#34010 = FACE_OUTER_BOUND ( 'NONE', #16429, .T. ) ;
#34011 = ORIENTED_EDGE ( 'NONE', *, *, #31203, .T. ) ;
#34012 = AXIS2_PLACEMENT_3D ( 'NONE', #34707, #26203, #43506 ) ;
#34013 = FACE_OUTER_BOUND ( 'NONE', #48454, .T. ) ;
#34014 = CARTESIAN_POINT ( 'NONE',  ( -14.46888367232926420, 0.000000000000000000, 12.59025272694991315 ) ) ;
#34015 = EDGE_CURVE ( 'NONE', #51439, #21119, #31149, .T. ) ;
#34016 = VECTOR ( 'NONE', #53398, 1000.000000000000114 ) ;
#34017 = LINE ( 'NONE', #38552, #39664 ) ;
#34018 = VECTOR ( 'NONE', #23135, 1000.000000000000227 ) ;
#34019 = CARTESIAN_POINT ( 'NONE',  ( -14.01545677930355183, 0.000000000000000000, 2.126011111488108174 ) ) ;
#34020 = CARTESIAN_POINT ( 'NONE',  ( 2.072287782118878319, 0.000000000000000000, -2.950529333540147015 ) ) ;
#34021 = CARTESIAN_POINT ( 'NONE',  ( -22.40556560354864146, -0.1191753592594197858, 5.484709000965211523 ) ) ;
#34022 = CARTESIAN_POINT ( 'NONE',  ( -24.26986129792355129, -0.1191753592594197858, 6.208864760408702388 ) ) ;
#34023 = CARTESIAN_POINT ( 'NONE',  ( -14.88235982785061218, 0.000000000000000000, 6.012591425800175138 ) ) ;
#34024 = ORIENTED_EDGE ( 'NONE', *, *, #40287, .T. ) ;
#34025 = CARTESIAN_POINT ( 'NONE',  ( 2.072287782118878319, 0.000000000000000000, -2.950529333540147015 ) ) ;
#34026 = ORIENTED_EDGE ( 'NONE', *, *, #18702, .F. ) ;
#34027 = DIRECTION ( 'NONE',  ( 0.9999697198139515519, 0.000000000000000000, 0.007781995580013368816 ) ) ;
#34028 = DIRECTION ( 'NONE',  ( -0.5364919789714478471, 0.6444004775717705469, -0.5449076811759709926 ) ) ;
#34029 = CARTESIAN_POINT ( 'NONE',  ( -27.06630483948590893, -0.1191753592594197858, 7.295098399573937797 ) ) ;
#34030 = DIRECTION ( 'NONE',  ( 0.005961354470445682716, -0.6427876096865404731, -0.7660212471507180654 ) ) ;
#34031 = CARTESIAN_POINT ( 'NONE',  ( -15.56555264407546346, 0.000000000000000000, 8.392593093757724887 ) ) ;
#34032 = VECTOR ( 'NONE', #53270, 1000.000000000000227 ) ;
#34033 = CARTESIAN_POINT ( 'NONE',  ( -16.89925026227929195, -0.1191753592594197858, 13.49466922669627422 ) ) ;
#34034 = ITEM_DEFINED_TRANSFORMATION ( 'NONE', 'NONE', #9037,  #2610 ) ;
#34035 = VECTOR ( 'NONE', #55025, 1000.000000000000227 ) ;
#34036 = VERTEX_POINT ( 'NONE', #56158 ) ;
#34037 = CARTESIAN_POINT ( 'NONE',  ( -27.65699453300243249, 14.95845179970709182, 4.704869143278580523 ) ) ;
#34038 = CARTESIAN_POINT ( 'NONE',  ( -13.40764798327444574, 3.524445264749008988, 7.873522038848314253 ) ) ;
#34039 = LINE ( 'NONE', #7625, #10987 ) ;
#34040 = AXIS2_PLACEMENT_3D ( 'NONE', #8965, #13220, #22305 ) ;
#34041 = LINE ( 'NONE', #54759, #23702 ) ;
#34042 = ADVANCED_FACE ( 'NONE', ( #30621 ), #52460, .F. ) ;
#34043 = AXIS2_PLACEMENT_3D ( 'NONE', #42531, #42253, #16388 ) ;
#34044 = PLANE ( 'NONE',  #22099 ) ;
#34045 = PLANE ( 'NONE',  #5082 ) ;
#34046 = LINE ( 'NONE', #51371, #218 ) ;
#34047 = ORIENTED_EDGE ( 'NONE', *, *, #40064, .F. ) ;
#34048 = PLANE ( 'NONE',  #35809 ) ;
#34049 = VECTOR ( 'NONE', #32121, 999.9999999999998863 ) ;
#34050 = CARTESIAN_POINT ( 'NONE',  ( 2.072287782118878319, 0.000000000000000000, -2.950529333540147015 ) ) ;
#34051 = VECTOR ( 'NONE', #19996, 1000.000000000000227 ) ;
#34052 = VERTEX_POINT ( 'NONE', #4215 ) ;
#34053 = EDGE_LOOP ( 'NONE', ( #40674, #6645, #4364, #45497 ) ) ;
#34054 = DIRECTION ( 'NONE',  ( 0.000000000000000000, 0.000000000000000000, 1.000000000000000000 ) ) ;
#34055 = VECTOR ( 'NONE', #19203, 1000.000000000000227 ) ;
#34056 = EDGE_CURVE ( 'NONE', #28808, #42382, #39107, .T. ) ;
#34057 = ORIENTED_EDGE ( 'NONE', *, *, #42752, .T. ) ;
#34058 = VECTOR ( 'NONE', #26119, 1000.000000000000227 ) ;
#34059 = EDGE_CURVE ( 'NONE', #14066, #34341, #26077, .T. ) ;
#34060 = ADVANCED_FACE ( 'NONE', ( #34863 ), #48174, .F. ) ;
#34061 = AXIS2_PLACEMENT_3D ( 'NONE', #29140, #42218, #37961 ) ;
#34062 = ORIENTED_EDGE ( 'NONE', *, *, #21050, .F. ) ;
#34063 = VECTOR ( 'NONE', #41561, 1000.000000000000227 ) ;
#34064 = ORIENTED_EDGE ( 'NONE', *, *, #3977, .T. ) ;
#34065 = ORIENTED_EDGE ( 'NONE', *, *, #29963, .T. ) ;
#34066 = CARTESIAN_POINT ( 'NONE',  ( -23.32622135384906770, 18.90220053346460105, 4.407440554554201917 ) ) ;
#34067 = CARTESIAN_POINT ( 'NONE',  ( -66.04860918961693983, -9.268670510630919068, -5.126440291711352515 ) ) ;
#34068 = EDGE_CURVE ( 'NONE', #56109, #8019, #16989, .T. ) ;
#34069 = DIRECTION ( 'NONE',  ( 0.007781995580012662783, 0.000000000000000000, -0.9999697198139514409 ) ) ;
#34070 = EDGE_CURVE ( 'NONE', #40934, #55582, #12714, .T. ) ;
#34071 = ORIENTED_EDGE ( 'NONE', *, *, #26061, .T. ) ;
#34072 = ORIENTED_EDGE ( 'NONE', *, *, #23256, .F. ) ;
#34073 = EDGE_CURVE ( 'NONE', #33398, #20973, #26606, .T. ) ;
#34074 = VECTOR ( 'NONE', #10010, 1000.000000000000000 ) ;
#34075 = PLANE ( 'NONE',  #5791 ) ;
#34076 = PLANE ( 'NONE',  #49048 ) ;
#34077 = VECTOR ( 'NONE', #42455, 1000.000000000000000 ) ;
#34078 = ORIENTED_EDGE ( 'NONE', *, *, #42450, .F. ) ;
#34079 = LINE ( 'NONE', #51657, #43662 ) ;
#34080 = CARTESIAN_POINT ( 'NONE',  ( -25.20200914511100265, -0.1191753592594197858, 6.570942640130446932 ) ) ;
#34081 = EDGE_LOOP ( 'NONE', ( #38664, #39500, #19474, #36256 ) ) ;
#34082 = AXIS2_PLACEMENT_3D ( 'NONE', #4366, #25367, #16549 ) ;
#34083 = CARTESIAN_POINT ( 'NONE',  ( -10.66326506071217040, 0.000000000000000000, 1.244108489361323677 ) ) ;
#34084 = ADVANCED_FACE ( 'NONE', ( #25774 ), #39403, .F. ) ;
#34085 = ORIENTED_EDGE ( 'NONE', *, *, #2822, .T. ) ;
#34086 = CARTESIAN_POINT ( 'NONE',  ( -18.66354898467281132, 0.000000000000000000, 14.21960318569776582 ) ) ;
#34087 = AXIS2_PLACEMENT_3D ( 'NONE', #6859, #41494, #40917 ) ;
#34088 = EDGE_CURVE ( 'NONE', #10254, #55582, #17531, .T. ) ;
#34089 = LINE ( 'NONE', #26376, #51767 ) ;
#34090 = VECTOR ( 'NONE', #47782, 1000.000000000000227 ) ;
#34091 = VERTEX_POINT ( 'NONE', #47641 ) ;
#34092 = CARTESIAN_POINT ( 'NONE',  ( -11.20636620717317378, 0.000000000000000000, 11.32298014792380414 ) ) ;
#34093 = DIRECTION ( 'NONE',  ( 0.007781995580012663651, 0.000000000000000000, -0.9999697198139515519 ) ) ;
#34094 = DIRECTION ( 'NONE',  ( -0.8531650599175529814, -0.4028455766673920135, 0.3313982828793697877 ) ) ;
#34095 = DIRECTION ( 'NONE',  ( 0.7660212471507180654, -0.6427876096865404731, 0.005961354470445141482 ) ) ;
#34096 = EDGE_LOOP ( 'NONE', ( #25374, #10002, #9834, #46466 ) ) ;
#34097 = AXIS2_PLACEMENT_3D ( 'NONE', #52112, #48121, #22312 ) ;
#34098 = VECTOR ( 'NONE', #49657, 1000.000000000000000 ) ;
#34099 = PLANE ( 'NONE',  #42789 ) ;
#34100 = PLANE ( 'NONE',  #52316 ) ;
#34101 = LINE ( 'NONE', #43185, #4035 ) ;
#34102 = FACE_OUTER_BOUND ( 'NONE', #35574, .T. ) ;
#34103 = CARTESIAN_POINT ( 'NONE',  ( -16.99924723426068951, 0.000000000000000000, 13.49389102713827171 ) ) ;
#34104 = FACE_OUTER_BOUND ( 'NONE', #52402, .T. ) ;
#34105 = VECTOR ( 'NONE', #19304, 999.9999999999998863 ) ;
#34106 = AXIS2_PLACEMENT_3D ( 'NONE', #29977, #39055, #52660 ) ;
#34107 = CARTESIAN_POINT ( 'NONE',  ( -66.80765385348918528, -11.36882057637399512, -7.559434449094163178 ) ) ;
#34108 = ORIENTED_EDGE ( 'NONE', *, *, #53683, .F. ) ;
#34109 = CARTESIAN_POINT ( 'NONE',  ( -68.08080254705713230, -5.290906601729261638E-14, 7.854170068342909872 ) ) ;
#34110 = ORIENTED_EDGE ( 'NONE', *, *, #10719, .F. ) ;
#34111 = LINE ( 'NONE', #21320, #20260 ) ;
#34112 = CARTESIAN_POINT ( 'NONE',  ( -19.26121178987789051, 0.000000000000000000, 5.609182117514321497 ) ) ;
#34113 = EDGE_CURVE ( 'NONE', #21256, #42731, #497, .T. ) ;
#34114 = DIRECTION ( 'NONE',  ( -0.005002170337468016433, -0.7660444431189770143, 0.6427681459581293666 ) ) ;
#34115 = EDGE_CURVE ( 'NONE', #37525, #9203, #51879, .T. ) ;
#34116 = LINE ( 'NONE', #3997, #36032 ) ;
#34117 = LINE ( 'NONE', #4303, #39264 ) ;
#34118 = VECTOR ( 'NONE', #49114, 1000.000000000000227 ) ;
#34119 = ORIENTED_EDGE ( 'NONE', *, *, #32173, .T. ) ;
#34120 = ORIENTED_EDGE ( 'NONE', *, *, #53262, .T. ) ;
#34121 = CARTESIAN_POINT ( 'NONE',  ( -17.46532115785441519, 0.000000000000000000, 13.67492996699914265 ) ) ;
#34122 = DIRECTION ( 'NONE',  ( -0.8531650599175529814, -0.4028455766673920135, 0.3313982828793697877 ) ) ;
#34123 = EDGE_LOOP ( 'NONE', ( #16432, #21873, #28467, #7238 ) ) ;
#34124 = AXIS2_PLACEMENT_3D ( 'NONE', #6640, #49539, #32746 ) ;
#34125 = ADVANCED_FACE ( 'NONE', ( #43386 ), #13292, .F. ) ;
#34126 = ADVANCED_FACE ( 'NONE', ( #17832 ), #35163, .F. ) ;
#34127 = EDGE_CURVE ( 'NONE', #3505, #3254, #32294, .T. ) ;
#34128 = DIRECTION ( 'NONE',  ( -0.3620778797217457656, 0.000000000000000000, -0.9321478471874539151 ) ) ;
#34129 = ORIENTED_EDGE ( 'NONE', *, *, #20665, .T. ) ;
#34130 = LINE ( 'NONE', #46906, #15005 ) ;
#34131 = AXIS2_PLACEMENT_3D ( 'NONE', #47985, #48837, #9084 ) ;
#34132 = ORIENTED_EDGE ( 'NONE', *, *, #21933, .T. ) ;
#34133 = DIRECTION ( 'NONE',  ( 0.007781995580012663651, -3.146120232559066537E-19, -0.9999697198139514409 ) ) ;
#34134 = ADVANCED_FACE ( 'NONE', ( #41063 ), #6179, .F. ) ;
#34135 = AXIS2_PLACEMENT_3D ( 'NONE', #43446, #17055, #261 ) ;
#34136 = ORIENTED_EDGE ( 'NONE', *, *, #18421, .T. ) ;
#34137 = ORIENTED_EDGE ( 'NONE', *, *, #25740, .F. ) ;
#34138 = VERTEX_POINT ( 'NONE', #1618 ) ;
#34139 = CARTESIAN_POINT ( 'NONE',  ( -12.31313304499984440, 4.495856970884013037, 1.321329386160589703 ) ) ;
#34140 = DIRECTION ( 'NONE',  ( 0.007781995580012663651, 0.000000000000000000, -0.9999697198139515519 ) ) ;
#34141 = FACE_OUTER_BOUND ( 'NONE', #22223, .T. ) ;
#34142 = VECTOR ( 'NONE', #21139, 999.9999999999998863 ) ;
#34143 = VECTOR ( 'NONE', #38117, 1000.000000000000227 ) ;
#34144 = CARTESIAN_POINT ( 'NONE',  ( -20.54204810873173415, 0.000000000000000000, 4.860550213503115558 ) ) ;
#34145 = EDGE_CURVE ( 'NONE', #17633, #36664, #28022, .T. ) ;
#34146 = ORIENTED_EDGE ( 'NONE', *, *, #53096, .T. ) ;
#34147 = EDGE_LOOP ( 'NONE', ( #52360, #49431, #13978, #24324 ) ) ;
#34148 = VECTOR ( 'NONE', #45356, 1000.000000000000227 ) ;
#34149 = EDGE_CURVE ( 'NONE', #608, #50606, #27173, .T. ) ;
#34150 = EDGE_LOOP ( 'NONE', ( #35194, #49762, #33507, #1214 ) ) ;
#34151 = PLANE ( 'NONE',  #26794 ) ;
#34152 = DIRECTION ( 'NONE',  ( 0.9999697198139515519, 0.000000000000000000, 0.007781995580013368816 ) ) ;
#34153 = EDGE_CURVE ( 'NONE', #11770, #52378, #53564, .T. ) ;
#34154 = ORIENTED_EDGE ( 'NONE', *, *, #49899, .F. ) ;
#34155 = CARTESIAN_POINT ( 'NONE',  ( -19.32961685222932147, 0.000000000000000000, 14.39908572644263351 ) ) ;
#34156 = ORIENTED_EDGE ( 'NONE', *, *, #36885, .F. ) ;
#34157 = CARTESIAN_POINT ( 'NONE',  ( -19.60990026154428278, 0.000000000000000000, 4.498472333781370125 ) ) ;
#34158 = CARTESIAN_POINT ( 'NONE',  ( -13.67982092077429890, 0.000000000000000000, 4.913953652214907208 ) ) ;
#34159 = EDGE_CURVE ( 'NONE', #51983, #43785, #36526, .T. ) ;
#34160 = ORIENTED_EDGE ( 'NONE', *, *, #30344, .T. ) ;
#34161 = CARTESIAN_POINT ( 'NONE',  ( -12.18226100520636379, -0.1191753592594183703, 4.456272911837774409 ) ) ;
#34162 = ORIENTED_EDGE ( 'NONE', *, *, #14291, .F. ) ;
#34163 = AXIS2_PLACEMENT_3D ( 'NONE', #37604, #16571, #33361 ) ;
#34164 = CARTESIAN_POINT ( 'NONE',  ( -19.70588832770281584, 2.167151335408493029, 6.911193162818738855 ) ) ;
#34165 = DIRECTION ( 'NONE',  ( 0.000000000000000000, 1.000000000000000000, 0.000000000000000000 ) ) ;
#34166 = VERTEX_POINT ( 'NONE', #14414 ) ;
#34167 = FACE_OUTER_BOUND ( 'NONE', #40276, .T. ) ;
#34168 = CARTESIAN_POINT ( 'NONE',  ( -13.37456397384763740, 0.7721120973665037690, 1.852432162681123984 ) ) ;
#34169 = LINE ( 'NONE', #24777, #22354 ) ;
#34170 = CARTESIAN_POINT ( 'NONE',  ( -19.32961685222932147, 0.000000000000000000, 14.39908572644263351 ) ) ;
#34171 = AXIS2_PLACEMENT_3D ( 'NONE', #25026, #7990, #4829 ) ;
#34172 = ORIENTED_EDGE ( 'NONE', *, *, #52054, .F. ) ;
#34173 = DIRECTION ( 'NONE',  ( 0.005961354470445682716, -0.6427876096865404731, -0.7660212471507180654 ) ) ;
#34174 = VECTOR ( 'NONE', #4166, 999.9999999999998863 ) ;
#34175 = DIRECTION ( 'NONE',  ( 0.005002170337468016433, -0.7660444431189770143, -0.6427681459581293666 ) ) ;
#34176 = CARTESIAN_POINT ( 'NONE',  ( -20.54204810873173415, 0.000000000000000000, 4.860550213503115558 ) ) ;
#34177 = FACE_OUTER_BOUND ( 'NONE', #29883, .T. ) ;
#34178 = CARTESIAN_POINT ( 'NONE',  ( -11.69750573382829550, -0.1191753592594198274, 1.874720900801436940 ) ) ;
#34179 = VECTOR ( 'NONE', #38004, 1000.000000000000000 ) ;
#34180 = DIRECTION ( 'NONE',  ( 0.6427681459581294776, -0.7660444431189769032, 0.005002170337467562802 ) ) ;
#34181 = ORIENTED_EDGE ( 'NONE', *, *, #31356, .F. ) ;
#34182 = PLANE ( 'NONE',  #798 ) ;
#34183 = DIRECTION ( 'NONE',  ( 0.000000000000000000, -1.000000000000000000, 0.000000000000000000 ) ) ;
#34184 = CARTESIAN_POINT ( 'NONE',  ( -13.97961799777601932, -5.051250379848164940, 2.150318164026983947 ) ) ;
#34185 = ORIENTED_EDGE ( 'NONE', *, *, #49364, .F. ) ;
#34186 = DIRECTION ( 'NONE',  ( 0.007781995580012663651, -3.146120232559066537E-19, -0.9999697198139514409 ) ) ;
#34187 = ORIENTED_EDGE ( 'NONE', *, *, #21624, .F. ) ;
#34188 = EDGE_CURVE ( 'NONE', #24292, #171, #2150, .T. ) ;
#34189 = DIRECTION ( 'NONE',  ( 0.6427681459581294776, -0.7660444431189769032, 0.005002170337467562802 ) ) ;
#34190 = DIRECTION ( 'NONE',  ( 0.007781995580012663651, 0.000000000000000000, -0.9999697198139515519 ) ) ;
#34191 = VECTOR ( 'NONE', #32604, 999.9999999999998863 ) ;
#34192 = EDGE_CURVE ( 'NONE', #19170, #3617, #36832, .T. ) ;
#34193 = CARTESIAN_POINT ( 'NONE',  ( -15.79858100839565083, 0.000000000000000000, 4.328126845270309886 ) ) ;
#34194 = AXIS2_PLACEMENT_3D ( 'NONE', #49890, #53059, #44515 ) ;
#34195 = CARTESIAN_POINT ( 'NONE',  ( -68.73712005124077962, 0.1329671457173686178, 5.608481661908657934 ) ) ;
#34196 = ORIENTED_EDGE ( 'NONE', *, *, #34373, .F. ) ;
#34197 = AXIS2_PLACEMENT_3D ( 'NONE', #22462, #52803, #11039 ) ;
#34198 = ORIENTED_EDGE ( 'NONE', *, *, #47024, .F. ) ;
#34199 = CARTESIAN_POINT ( 'NONE',  ( -67.09057908004916726, -0.6008667158328537816, -1.335442097082733870 ) ) ;
#34200 = LINE ( 'NONE', #30769, #55837 ) ;
#34201 = PLANE ( 'NONE',  #37775 ) ;
#34202 = EDGE_CURVE ( 'NONE', #5703, #37228, #49610, .T. ) ;
#34203 = EDGE_CURVE ( 'NONE', #53459, #19068, #1321, .T. ) ;
#34204 = EDGE_CURVE ( 'NONE', #44736, #47582, #18363, .T. ) ;
#34205 = FACE_OUTER_BOUND ( 'NONE', #4181, .T. ) ;
#34206 = FACE_OUTER_BOUND ( 'NONE', #47176, .T. ) ;
#34207 = DIRECTION ( 'NONE',  ( 0.007781995580012662783, 0.000000000000000000, -0.9999697198139514409 ) ) ;
#34209 = EDGE_CURVE ( 'NONE', #36112, #39217, #49311, .T. ) ;
#34208 = ORIENTED_EDGE ( 'NONE', *, *, #22722, .T. ) ;
#34210 = CARTESIAN_POINT ( 'NONE',  ( -70.00259797851279586, 0.1329035588801656675, 7.501778215771297553 ) ) ;
#34211 = AXIS2_PLACEMENT_3D ( 'NONE', #879, #26728, #44054 ) ;
#34212 = CARTESIAN_POINT ( 'NONE',  ( -50.02554558092695913, 3.776013638374817294, 5.000000000000000000 ) ) ;
#34213 = ORIENTED_EDGE ( 'NONE', *, *, #12249, .F. ) ;
#34214 = DIRECTION ( 'NONE',  ( -0.9999697198139514409, -0.000000000000000000, -0.007781995580013368816 ) ) ;
#34215 = FACE_OUTER_BOUND ( 'NONE', #37553, .T. ) ;
#34216 = LINE ( 'NONE', #44384, #40204 ) ;
#34217 = ORIENTED_EDGE ( 'NONE', *, *, #55930, .T. ) ;
#34218 = CARTESIAN_POINT ( 'NONE',  ( -16.64444113932924196, -1.003701604285656579, 4.794443245222647754 ) ) ;
#34219 = VECTOR ( 'NONE', #34740, 1000.000000000000000 ) ;
#34220 = EDGE_LOOP ( 'NONE', ( #6382, #29680, #35859, #14722 ) ) ;
#34221 = EDGE_CURVE ( 'NONE', #32474, #47218, #10127, .T. ) ;
#34223 = ORIENTED_EDGE ( 'NONE', *, *, #13867, .F. ) ;
#34222 = ADVANCED_FACE ( 'NONE', ( #27754 ), #45074, .F. ) ;
#34224 = VECTOR ( 'NONE', #37038, 1000.000000000000227 ) ;
#34225 = EDGE_LOOP ( 'NONE', ( #3244, #29398, #9635, #43680 ) ) ;
#34226 = EDGE_CURVE ( 'NONE', #27231, #27480, #35701, .T. ) ;
#34227 = VERTEX_POINT ( 'NONE', #54144 ) ;
#34228 = LINE ( 'NONE', #43304, #22108 ) ;
#34229 = EDGE_LOOP ( 'NONE', ( #19302, #46140, #55787, #20654, #19753 ) ) ;
#34230 = PLANE ( 'NONE',  #4090 ) ;
#34231 = EDGE_CURVE ( 'NONE', #23596, #44456, #1871, .T. ) ;
#34232 = AXIS2_PLACEMENT_3D ( 'NONE', #18087, #5325, #9279 ) ;
#34233 = VERTEX_POINT ( 'NONE', #10959 ) ;
#34234 = LINE ( 'NONE', #29093, #55840 ) ;
#34235 = EDGE_LOOP ( 'NONE', ( #5278, #37297, #35472, #51093 ) ) ;
#34236 = VERTEX_POINT ( 'NONE', #53017 ) ;
#34237 = EDGE_CURVE ( 'NONE', #947, #45223, #28278, .T. ) ;
#34238 = FACE_OUTER_BOUND ( 'NONE', #5764, .T. ) ;
#34239 = FACE_OUTER_BOUND ( 'NONE', #6285, .T. ) ;
#34240 = PLANE ( 'NONE',  #35838 ) ;
#34241 = DIRECTION ( 'NONE',  ( -0.5364919789714478471, 0.6444004775717705469, -0.5449076811759709926 ) ) ;
#34242 = DIRECTION ( 'NONE',  ( -0.005961354470445682716, -0.6427876096865404731, 0.7660212471507180654 ) ) ;
#34243 = VERTEX_POINT ( 'NONE', #36009 ) ;
#34244 = EDGE_LOOP ( 'NONE', ( #30651, #30680, #10470, #2019 ) ) ;
#34245 = DIRECTION ( 'NONE',  ( -0.3313982828793700652, 0.4028455766673916250, -0.8531650599175529814 ) ) ;
#34246 = DIRECTION ( 'NONE',  ( 0.5364919789714477361, 0.6444004775717706579, 0.5449076811759711036 ) ) ;
#34247 = DIRECTION ( 'NONE',  ( 0.6246952433987893460, 0.7422098413412802076, -0.2426528472758539279 ) ) ;
#34248 = CARTESIAN_POINT ( 'NONE',  ( -20.54049170961573267, 0.000000000000000000, 4.660556269540326646 ) ) ;
#34249 = CARTESIAN_POINT ( 'NONE',  ( -14.66887761629205222, 0.000000000000000000, 12.58869632783390990 ) ) ;
#34250 = DIRECTION ( 'NONE',  ( 0.000000000000000000, -0.000000000000000000, -1.000000000000000000 ) ) ;
#34251 = ORIENTED_EDGE ( 'NONE', *, *, #54124, .F. ) ;
#34252 = FACE_OUTER_BOUND ( 'NONE', #54703, .T. ) ;
#34253 = PLANE ( 'NONE',  #31322 ) ;
#34254 = ORIENTED_EDGE ( 'NONE', *, *, #17615, .F. ) ;
#34255 = CARTESIAN_POINT ( 'NONE',  ( -9.342070512798265725, 0.000000000000000000, 10.59882438848031505 ) ) ;
#34256 = DIRECTION ( 'NONE',  ( 0.5364919789714477361, 0.6444004775717706579, 0.5449076811759711036 ) ) ;
#34257 = DIRECTION ( 'NONE',  ( 0.7660212471507180654, -0.6427876096865404731, 0.005961354470445141482 ) ) ;
#34258 = DIRECTION ( 'NONE',  ( 1.000000000000000000, 0.000000000000000000, 0.000000000000000000 ) ) ;
#34259 = VECTOR ( 'NONE', #23688, 999.9999999999998863 ) ;
#34260 = VERTEX_POINT ( 'NONE', #33503 ) ;
#34261 = ORIENTED_EDGE ( 'NONE', *, *, #37837, .F. ) ;
#34262 = DIRECTION ( 'NONE',  ( 0.5449076811759707706, 0.6444004775717708799, -0.5364919789714476250 ) ) ;
#34263 = LINE ( 'NONE', #21173, #28591 ) ;
#34264 = DIRECTION ( 'NONE',  ( -0.9999697198139514409, -0.000000000000000000, -0.007781995580013368816 ) ) ;
#34265 = ADVANCED_FACE ( 'NONE', ( #33242 ), #29537, .F. ) ;
#34266 = VECTOR ( 'NONE', #16767, 1000.000000000000227 ) ;
#34267 = CARTESIAN_POINT ( 'NONE',  ( -10.27421835998572064, 0.000000000000000000, 10.96090226820206048 ) ) ;
#34268 = DIRECTION ( 'NONE',  ( -0.7886751345948130876, 0.2113248654051844977, -0.5773502691896263972 ) ) ;
#34269 = EDGE_CURVE ( 'NONE', #22414, #13266, #46852, .T. ) ;
#34270 = CARTESIAN_POINT ( 'NONE',  ( -19.28774072249866478, -2.460819163488157546, 8.212568725711509643 ) ) ;
#34271 = EDGE_CURVE ( 'NONE', #21088, #8091, #54498, .T. ) ;
#34272 = FACE_OUTER_BOUND ( 'NONE', #10307, .T. ) ;
#34273 = DIRECTION ( 'NONE',  ( 0.9999697198139515519, 0.000000000000000000, 0.007781995580013368816 ) ) ;
#34274 = LINE ( 'NONE', #51579, #14238 ) ;
#34275 = CARTESIAN_POINT ( 'NONE',  ( 2.072287782118878319, 0.000000000000000000, -2.950529333540147015 ) ) ;
#34276 = ORIENTED_EDGE ( 'NONE', *, *, #2385, .T. ) ;
#34277 = PLANE ( 'NONE',  #11390 ) ;
#34278 = ORIENTED_EDGE ( 'NONE', *, *, #24515, .T. ) ;
#34279 = ORIENTED_EDGE ( 'NONE', *, *, #40264, .T. ) ;
#34280 = ORIENTED_EDGE ( 'NONE', *, *, #48695, .F. ) ;
#34281 = EDGE_LOOP ( 'NONE', ( #32257, #6746, #31491, #37537 ) ) ;
#34282 = VERTEX_POINT ( 'NONE', #24684 ) ;
#34283 = ORIENTED_EDGE ( 'NONE', *, *, #35323, .F. ) ;
#34284 = CARTESIAN_POINT ( 'NONE',  ( -17.83139810946674686, -0.1191753592594197858, 13.85674710641801788 ) ) ;
#34285 = CARTESIAN_POINT ( 'NONE',  ( -16.81793962562570144, -0.1166911823299060097, 3.314285314562989360 ) ) ;
#34286 = DIRECTION ( 'NONE',  ( 0.000000000000000000, -0.000000000000000000, -1.000000000000000000 ) ) ;
#34287 = ORIENTED_EDGE ( 'NONE', *, *, #16453, .T. ) ;
#34288 = CARTESIAN_POINT ( 'NONE',  ( -26.13337879274045505, 0.000000000000000000, 6.833023547870798353 ) ) ;
#34289 = ORIENTED_EDGE ( 'NONE', *, *, #31592, .F. ) ;
#34290 = LINE ( 'NONE', #51598, #28606 ) ;
#34291 = ORIENTED_EDGE ( 'NONE', *, *, #45294, .T. ) ;
#34292 = EDGE_CURVE ( 'NONE', #4182, #35810, #28963, .T. ) ;
#34293 = DIRECTION ( 'NONE',  ( -0.5449076811759708816, 0.6444004775717707689, 0.5364919789714475140 ) ) ;
#34294 = ADVANCED_FACE ( 'NONE', ( #7663 ), #37779, .F. ) ;
#34295 = CARTESIAN_POINT ( 'NONE',  ( -25.20123094555300369, 0.000000000000000000, 6.470945668149052032 ) ) ;
#34296 = FACE_OUTER_BOUND ( 'NONE', #28239, .T. ) ;
#34297 = EDGE_LOOP ( 'NONE', ( #45866, #8792, #48825, #39764 ) ) ;
#34298 = DIRECTION ( 'NONE',  ( 0.6427681459581294776, -0.7660444431189769032, 0.005002170337467562802 ) ) ;
#34299 = ORIENTED_EDGE ( 'NONE', *, *, #54193, .T. ) ;
#34300 = AXIS2_PLACEMENT_3D ( 'NONE', #44701, #48118, #43864 ) ;
#34301 = PLANE ( 'NONE',  #11896 ) ;
#34302 = EDGE_CURVE ( 'NONE', #6152, #26523, #50250, .T. ) ;
#34303 = PLANE ( 'NONE',  #24827 ) ;
#34304 = CARTESIAN_POINT ( 'NONE',  ( -9.542064456761055524, 0.000000000000000000, 10.59726798936431180 ) ) ;
#34305 = PLANE ( 'NONE',  #26782 ) ;
#34306 = CARTESIAN_POINT ( 'NONE',  ( -13.86944162542047287, -3.756034771668159689, 8.233586821798175137 ) ) ;
#34307 = CARTESIAN_POINT ( 'NONE',  ( -12.96168924638702968, -0.5179957512181557755, 1.899554624828523108 ) ) ;
#34308 = LINE ( 'NONE', #55886, #27548 ) ;
#34309 = FACE_OUTER_BOUND ( 'NONE', #29958, .T. ) ;
#34310 = ORIENTED_EDGE ( 'NONE', *, *, #29645, .T. ) ;
#34311 = DIRECTION ( 'NONE',  ( 0.9999697198139515519, 0.000000000000000000, 0.007781995580013368816 ) ) ;
#34312 = EDGE_LOOP ( 'NONE', ( #5811, #29449, #50236, #42367 ) ) ;
#34313 = CARTESIAN_POINT ( 'NONE',  ( -17.93139508144814442, 0.000000000000000000, 13.85596890686001537 ) ) ;
#34314 = DIRECTION ( 'NONE',  ( 0.007781995580012663651, -3.146120232559066537E-19, -0.9999697198139514409 ) ) ;
#34315 = DIRECTION ( 'NONE',  ( 0.9999697198139515519, 0.000000000000000000, 0.007781995580013368816 ) ) ;
#34316 = PLANE ( 'NONE',  #39481 ) ;
#34317 = DIRECTION ( 'NONE',  ( 0.5449076811759707706, 0.6444004775717708799, -0.5364919789714476250 ) ) ;
#34318 = DIRECTION ( 'NONE',  ( -0.6427681459581293666, -0.7660444431189770143, -0.005002170337467561935 ) ) ;
#34319 = PRODUCT_CONTEXT ( 'NONE', #13390, 'mechanical' ) ;
#34320 = ORIENTED_EDGE ( 'NONE', *, *, #34558, .F. ) ;
#34321 = CARTESIAN_POINT ( 'NONE',  ( -14.01623497886155256, -0.1191753592594197858, 2.226008083469502630 ) ) ;
#34322 = CARTESIAN_POINT ( 'NONE',  ( -25.20200914511100265, -0.1191753592594197858, 6.570942640130446932 ) ) ;
#34323 = ADVANCED_FACE ( 'NONE', ( #3667 ), #42312, .F. ) ;
#34324 = DIRECTION ( 'NONE',  ( -0.005002170337468016433, -0.7660444431189770143, 0.6427681459581293666 ) ) ;
#34325 = EDGE_CURVE ( 'NONE', #28099, #1224, #3107, .T. ) ;
#34326 = LINE ( 'NONE', #17261, #39112 ) ;
#34327 = CARTESIAN_POINT ( 'NONE',  ( -58.00000000000000711, 3.800000000000002931, 7.102951435054649637E-15 ) ) ;
#34328 = LINE ( 'NONE', #38280, #5978 ) ;
#34329 = ADVANCED_FACE ( 'NONE', ( #51087 ), #11063, .F. ) ;
#34330 = EDGE_CURVE ( 'NONE', #41524, #7759, #28388, .T. ) ;
#34331 = DIRECTION ( 'NONE',  ( 0.005002170337468016433, -0.7660444431189770143, -0.6427681459581293666 ) ) ;
#34332 = EDGE_LOOP ( 'NONE', ( #14713, #8202, #53343, #8585 ) ) ;
#34333 = PLANE ( 'NONE',  #19458 ) ;
#34334 = LINE ( 'NONE', #54766, #18725 ) ;
#34335 = EDGE_LOOP ( 'NONE', ( #28843, #9957, #30264, #27010 ) ) ;
#34336 = ORIENTED_EDGE ( 'NONE', *, *, #24515, .F. ) ;
#34337 = LINE ( 'NONE', #33486, #29208 ) ;
#34338 = AXIS2_PLACEMENT_3D ( 'NONE', #32506, #20252, #19418 ) ;
#34339 = ORIENTED_EDGE ( 'NONE', *, *, #55601, .T. ) ;
#34340 = EDGE_CURVE ( 'NONE', #47897, #3535, #15739, .T. ) ;
#34341 = VERTEX_POINT ( 'NONE', #25270 ) ;
#34342 = EDGE_LOOP ( 'NONE', ( #41700, #14327, #41747, #10950 ) ) ;
#34343 = ORIENTED_EDGE ( 'NONE', *, *, #41815, .T. ) ;
#34344 = DIRECTION ( 'NONE',  ( -0.5364919789714478471, 0.6444004775717705469, -0.5449076811759709926 ) ) ;
#34345 = ORIENTED_EDGE ( 'NONE', *, *, #42339, .F. ) ;
#34346 = PLANE ( 'NONE',  #11482 ) ;
#34347 = LINE ( 'NONE', #55344, #6761 ) ;
#34348 = ORIENTED_EDGE ( 'NONE', *, *, #8100, .F. ) ;
#34349 = VERTEX_POINT ( 'NONE', #11361 ) ;
#34350 = CARTESIAN_POINT ( 'NONE',  ( -17.77227403482580570, -0.1191753592594188005, 6.259430486910483538 ) ) ;
#34351 = DIRECTION ( 'NONE',  ( 0.6427681459581294776, -0.7660444431189769032, 0.005002170337467562802 ) ) ;
#34352 = ORIENTED_EDGE ( 'NONE', *, *, #16630, .T. ) ;
#34353 = LINE ( 'NONE', #55635, #5571 ) ;
#34354 = CARTESIAN_POINT ( 'NONE',  ( -9.280420900666706885, 0.000000000000000000, 3.101530451399800103 ) ) ;
#34355 = ORIENTED_EDGE ( 'NONE', *, *, #44255, .F. ) ;
#34356 = LINE ( 'NONE', #51660, #11275 ) ;
#34357 = ORIENTED_EDGE ( 'NONE', *, *, #2622, .F. ) ;
#34358 = FACE_OUTER_BOUND ( 'NONE', #39383, .T. ) ;
#34359 = ADVANCED_FACE ( 'NONE', ( #33768 ), #15597, .F. ) ;
#34360 = LINE ( 'NONE', #29550, #30893 ) ;
#34361 = VERTEX_POINT ( 'NONE', #29228 ) ;
#34362 = FACE_OUTER_BOUND ( 'NONE', #42904, .T. ) ;
#34363 = CARTESIAN_POINT ( 'NONE',  ( -8.938424887834608867, -0.1191753592594185784, 5.589513403987136364 ) ) ;
#34364 = LINE ( 'NONE', #12214, #37520 ) ;
#34365 = DIRECTION ( 'NONE',  ( 0.9999697198139515519, 0.000000000000000000, 0.007781995580013368816 ) ) ;
#34366 = ORIENTED_EDGE ( 'NONE', *, *, #29944, .T. ) ;
#34367 = ADVANCED_FACE ( 'NONE', ( #15897 ), #34075, .F. ) ;
#34368 = DIRECTION ( 'NONE',  ( 0.7660212471507180654, -0.6427876096865404731, 0.005961354470445141482 ) ) ;
#34369 = LINE ( 'NONE', #25853, #12399 ) ;
#34370 = LINE ( 'NONE', #25553, #28512 ) ;
#34371 = LINE ( 'NONE', #51676, #4178 ) ;
#34372 = CARTESIAN_POINT ( 'NONE',  ( -27.99767448711536133, 0.000000000000000000, 7.557179307314289218 ) ) ;
#34373 = EDGE_CURVE ( 'NONE', #7084, #25458, #3353, .T. ) ;
#34374 = PLANE ( 'NONE',  #54829 ) ;
#34376 = EDGE_CURVE ( 'NONE', #50478, #55289, #12757, .T. ) ;
#34375 = CARTESIAN_POINT ( 'NONE',  ( -10.22563470401762764, 0.01196729935014182421, 0.6681340434156105568 ) ) ;
#34377 = DIRECTION ( 'NONE',  ( -0.5364919789714478471, 0.6444004775717705469, -0.5449076811759709926 ) ) ;
#34378 = LINE ( 'NONE', #38645, #37692 ) ;
#34379 = ORIENTED_EDGE ( 'NONE', *, *, #49247, .T. ) ;
#34380 = CARTESIAN_POINT ( 'NONE',  ( -69.19586433673185866, 2.103352214621878602E-14, 7.932749270814285047 ) ) ;
#34381 = VERTEX_POINT ( 'NONE', #21278 ) ;
#34382 = CARTESIAN_POINT ( 'NONE',  ( -14.00280974873554030, 0.000000000000000000, 12.40921378708904044 ) ) ;
#34383 = ADVANCED_FACE ( 'NONE', ( #39451 ), #43156, .F. ) ;
#34384 = PLANE ( 'NONE',  #43584 ) ;
#34385 = ADVANCED_FACE ( 'NONE', ( #38607 ), #47114, .F. ) ;
#34386 = CARTESIAN_POINT ( 'NONE',  ( -9.591484076946107606, 1.593386918697492494, 2.300716907277841727 ) ) ;
#34387 = CARTESIAN_POINT ( 'NONE',  ( -16.73935101609895426, 0.000000000000000000, 5.798133834765347494 ) ) ;
#34388 = EDGE_CURVE ( 'NONE', #1645, #31141, #51655, .T. ) ;
#34389 = CARTESIAN_POINT ( 'NONE',  ( -26.13493519185646008, 0.000000000000000000, 7.033017491833586377 ) ) ;
#34390 = ORIENTED_EDGE ( 'NONE', *, *, #26500, .T. ) ;
#34391 = ORIENTED_EDGE ( 'NONE', *, *, #54330, .F. ) ;
#34392 = CARTESIAN_POINT ( 'NONE',  ( -58.00000000000000711, -9.250000000000000000, 3.457106781186559896 ) ) ;
#34393 = DIRECTION ( 'NONE',  ( -0.6427681459581293666, -0.7660444431189770143, -0.005002170337467561935 ) ) ;
#34394 = VERTEX_POINT ( 'NONE', #48218 ) ;
#34395 = CARTESIAN_POINT ( 'NONE',  ( 2.072287782118878319, 0.000000000000000000, -2.950529333540147015 ) ) ;
#34396 = ADVANCED_FACE ( 'NONE', ( #9328 ), #4795, .F. ) ;
#34397 = ORIENTED_EDGE ( 'NONE', *, *, #31772, .T. ) ;
#34398 = DIRECTION ( 'NONE',  ( 0.000000000000000000, -0.000000000000000000, -1.000000000000000000 ) ) ;
#34399 = ORIENTED_EDGE ( 'NONE', *, *, #8617, .T. ) ;
#34400 = CARTESIAN_POINT ( 'NONE',  ( -10.00813838035478298, 0.000000000000000000, 10.77830692922518452 ) ) ;
#34401 = EDGE_CURVE ( 'NONE', #2695, #33003, #12498, .T. ) ;
#34402 = ORIENTED_EDGE ( 'NONE', *, *, #54064, .F. ) ;
#34403 = VERTEX_POINT ( 'NONE', #13592 ) ;
#34404 = ORIENTED_EDGE ( 'NONE', *, *, #11624, .T. ) ;
#34405 = CARTESIAN_POINT ( 'NONE',  ( -17.67305526240241065, 0.000000000000000000, 6.360205658449882726 ) ) ;
#34406 = LINE ( 'NONE', #11427, #32326 ) ;
#34407 = CARTESIAN_POINT ( 'NONE',  ( 2.072287782118878319, 0.000000000000000000, -2.950529333540147015 ) ) ;
#34408 = CARTESIAN_POINT ( 'NONE',  ( -22.40478740399063895, 0.000000000000000000, 5.384712028983816623 ) ) ;
#34409 = ORIENTED_EDGE ( 'NONE', *, *, #281, .T. ) ;
#34410 = ORIENTED_EDGE ( 'NONE', *, *, #42694, .F. ) ;
#34411 = ORIENTED_EDGE ( 'NONE', *, *, #34822, .F. ) ;
#34412 = CARTESIAN_POINT ( 'NONE',  ( -64.10539783498545319, 7.375519243179410545, -3.000000000000000000 ) ) ;
#34413 = ORIENTED_EDGE ( 'NONE', *, *, #2477, .F. ) ;
#34414 = FACE_OUTER_BOUND ( 'NONE', #54451, .T. ) ;
#34415 = ORIENTED_EDGE ( 'NONE', *, *, #16540, .F. ) ;
#34416 = DIRECTION ( 'NONE',  ( 0.6427681459581294776, -0.7660444431189769032, 0.005002170337467562802 ) ) ;
#34417 = DIRECTION ( 'NONE',  ( 0.005961354470445682716, -0.6427876096865404731, -0.7660212471507180654 ) ) ;
#34418 = VERTEX_POINT ( 'NONE', #34350 ) ;
#34419 = PLANE ( 'NONE',  #28605 ) ;
#34420 = EDGE_CURVE ( 'NONE', #8019, #29009, #13340, .T. ) ;
#34421 = ORIENTED_EDGE ( 'NONE', *, *, #13492, .F. ) ;
#34422 = DIRECTION ( 'NONE',  ( 0.000000000000000000, -0.000000000000000000, -1.000000000000000000 ) ) ;
#34423 = LINE ( 'NONE', #8294, #38359 ) ;
#34424 = ORIENTED_EDGE ( 'NONE', *, *, #35926, .T. ) ;
#34425 = CARTESIAN_POINT ( 'NONE',  ( -56.48844206942440138, 5.522788861961955398, 2.999999999999993339 ) ) ;
#34426 = LINE ( 'NONE', #42396, #28436 ) ;
#34427 = FACE_OUTER_BOUND ( 'NONE', #25990, .T. ) ;
#34428 = ORIENTED_EDGE ( 'NONE', *, *, #44441, .F. ) ;
#34429 = LINE ( 'NONE', #34703, #4746 ) ;
#34430 = FACE_OUTER_BOUND ( 'NONE', #43215, .T. ) ;
#34431 = CARTESIAN_POINT ( 'NONE',  ( -17.73140113748535285, 0.000000000000000000, 13.85752530597602039 ) ) ;
#34432 = DIRECTION ( 'NONE',  ( 0.000000000000000000, -0.000000000000000000, -1.000000000000000000 ) ) ;
#34434 = ADVANCED_FACE ( 'NONE', ( #9061 ), #43973, .F. ) ;
#34433 = DIRECTION ( 'NONE',  ( -0.000000000000000000, -0.000000000000000000, -1.000000000000000000 ) ) ;
#34435 = VERTEX_POINT ( 'NONE', #808 ) ;
#34436 = CARTESIAN_POINT ( 'NONE',  ( -9.342070512798265725, 0.000000000000000000, 10.59882438848031505 ) ) ;
#34437 = FACE_OUTER_BOUND ( 'NONE', #10549, .T. ) ;
#34438 = DIRECTION ( 'NONE',  ( 0.005961354470445682716, -0.6427876096865404731, -0.7660212471507180654 ) ) ;
#34439 = EDGE_LOOP ( 'NONE', ( #19598, #16503, #14733, #27266 ) ) ;
#34440 = DIRECTION ( 'NONE',  ( 0.005002170337468016433, -0.7660444431189770143, -0.6427681459581293666 ) ) ;
#34441 = DIRECTION ( 'NONE',  ( 0.5449076811759707706, 0.6444004775717708799, -0.5364919789714476250 ) ) ;
#34442 = ORIENTED_EDGE ( 'NONE', *, *, #33992, .F. ) ;
#34443 = CARTESIAN_POINT ( 'NONE',  ( -27.99923088623136636, 0.000000000000000000, 7.757173251277078130 ) ) ;
#34444 = DIRECTION ( 'NONE',  ( -0.5449076811759708816, 0.6444004775717707689, 0.5364919789714475140 ) ) ;
#34445 = ADVANCED_FACE ( 'NONE', ( #26366 ), #18128, .F. ) ;
#34446 = DIRECTION ( 'NONE',  ( 0.9999697198139515519, 0.000000000000000000, 0.007781995580013368816 ) ) ;
#34447 = EDGE_CURVE ( 'NONE', #18, #22349, #56198, .T. ) ;
#34448 = CARTESIAN_POINT ( 'NONE',  ( -68.95754730983136938, 2.000000000004385825, -6.247493715005127513 ) ) ;
#34449 = VERTEX_POINT ( 'NONE', #17284 ) ;
#34450 = VERTEX_POINT ( 'NONE', #8504 ) ;
#34451 = EDGE_CURVE ( 'NONE', #23008, #12964, #234, .T. ) ;
#34452 = FACE_OUTER_BOUND ( 'NONE', #6207, .T. ) ;
#34453 = CARTESIAN_POINT ( 'NONE',  ( -20.54049170961573267, 0.000000000000000000, 4.660556269540326646 ) ) ;
#34454 = CARTESIAN_POINT ( 'NONE',  ( -12.57759610834895447, 2.553033558614007603, 5.956849598244149391 ) ) ;
#34455 = PLANE ( 'NONE',  #46541 ) ;
#34456 = EDGE_CURVE ( 'NONE', #36489, #5931, #51925, .T. ) ;
#34457 = CARTESIAN_POINT ( 'NONE',  ( -24.57312852195785524, 18.34675584111407787, 4.549864924635812713 ) ) ;
#34458 = LINE ( 'NONE', #8924, #12195 ) ;
#34459 = ORIENTED_EDGE ( 'NONE', *, *, #4388, .F. ) ;
#34460 = CARTESIAN_POINT ( 'NONE',  ( -14.93495759592298988, 0.000000000000000000, 12.77129166681078409 ) ) ;
#34461 = ADVANCED_FACE ( 'NONE', ( #14717 ), #28058, .F. ) ;
#34462 = CARTESIAN_POINT ( 'NONE',  ( -17.53328333432119379, 2.391131607591508335, 3.416164794119107562 ) ) ;
#34463 = ORIENTED_EDGE ( 'NONE', *, *, #43837, .T. ) ;
#34464 = PLANE ( 'NONE',  #41979 ) ;
#34465 = FACE_OUTER_BOUND ( 'NONE', #43888, .T. ) ;
#34466 = CARTESIAN_POINT ( 'NONE',  ( -26.13415699229845757, -0.1191753592594197858, 6.933020519852192365 ) ) ;
#34467 = EDGE_LOOP ( 'NONE', ( #44053, #6892, #45683, #13645 ) ) ;
#34468 = DIRECTION ( 'NONE',  ( 0.5364919789714477361, 0.6444004775717706579, 0.5449076811759711036 ) ) ;
#34469 = ORIENTED_EDGE ( 'NONE', *, *, #1904, .F. ) ;
#34470 = VECTOR ( 'NONE', #28576, 999.9999999999998863 ) ;
#34471 = ORIENTED_EDGE ( 'NONE', *, *, #12549, .F. ) ;
#34472 = ORIENTED_EDGE ( 'NONE', *, *, #51181, .F. ) ;
#34473 = VERTEX_POINT ( 'NONE', #10172 ) ;
#34474 = DIRECTION ( 'NONE',  ( -0.005961354470445682716, -0.6427876096865404731, 0.7660212471507180654 ) ) ;
#34476 = EDGE_CURVE ( 'NONE', #34233, #29943, #1911, .T. ) ;
#34475 = ORIENTED_EDGE ( 'NONE', *, *, #19630, .F. ) ;
#34477 = DIRECTION ( 'NONE',  ( 0.6427681459581294776, -0.7660444431189769032, 0.005002170337467562802 ) ) ;
#34478 = ORIENTED_EDGE ( 'NONE', *, *, #41686, .F. ) ;
#34479 = DIRECTION ( 'NONE',  ( 0.3535533905932738974, -0.6123724356957929160, 0.7071067811865487940 ) ) ;
#34480 = ORIENTED_EDGE ( 'NONE', *, *, #21946, .T. ) ;
#34481 = CARTESIAN_POINT ( 'NONE',  ( -24.27063949748155380, 0.000000000000000000, 6.308861732390097288 ) ) ;
#34482 = EDGE_CURVE ( 'NONE', #12427, #18417, #46493, .T. ) ;
#34483 = VERTEX_POINT ( 'NONE', #1374 ) ;
#34484 = DIRECTION ( 'NONE',  ( 0.005002170337468016433, -0.7660444431189770143, -0.6427681459581293666 ) ) ;
#34485 = CARTESIAN_POINT ( 'NONE',  ( -18.39746900504187010, 0.000000000000000000, 14.03700784672088808 ) ) ;
#34486 = ADVANCED_FACE ( 'NONE', ( #35747 ), #45365, .F. ) ;
#34487 = CARTESIAN_POINT ( 'NONE',  ( -12.07729412577240602, 0.000000000000000000, 3.818428676861645776 ) ) ;
#34488 = CARTESIAN_POINT ( 'NONE',  ( -18.39746900504187010, 0.000000000000000000, 14.03700784672088808 ) ) ;
#34489 = CARTESIAN_POINT ( 'NONE',  ( -11.17676086714305761, 0.000000000000000000, 7.518757532975309132 ) ) ;
#34490 = EDGE_LOOP ( 'NONE', ( #2813, #32536, #40909, #42560 ) ) ;
#34491 = EDGE_CURVE ( 'NONE', #6556, #35938, #23521, .T. ) ;
#34492 = EDGE_CURVE ( 'NONE', #28751, #31964, #53067, .T. ) ;
#34493 = EDGE_CURVE ( 'NONE', #45180, #18779, #23257, .T. ) ;
#34494 = ORIENTED_EDGE ( 'NONE', *, *, #14738, .F. ) ;
#34495 = DIRECTION ( 'NONE',  ( 0.000000000000000000, -0.000000000000000000, -1.000000000000000000 ) ) ;
#34496 = CARTESIAN_POINT ( 'NONE',  ( -13.53673582514181106, 0.000000000000000000, 12.22817484722816772 ) ) ;
#34497 = CARTESIAN_POINT ( 'NONE',  ( -16.81267852042391198, -0.1191753592594197858, 3.312241722634738039 ) ) ;
#34498 = LINE ( 'NONE', #22837, #18554 ) ;
#34499 = DIRECTION ( 'NONE',  ( -0.5364919789714478471, 0.6444004775717705469, -0.5449076811759709926 ) ) ;
#34500 = DIRECTION ( 'NONE',  ( -0.5449076811759708816, 0.6444004775717707689, 0.5364919789714475140 ) ) ;
#34501 = ORIENTED_EDGE ( 'NONE', *, *, #29084, .T. ) ;
#34502 = DIRECTION ( 'NONE',  ( 0.007781995580012662783, 0.000000000000000000, -0.9999697198139514409 ) ) ;
#34503 = CYLINDRICAL_SURFACE ( 'NONE', #2280, 0.2499999999999998612 ) ;
#34504 = ORIENTED_EDGE ( 'NONE', *, *, #47633, .F. ) ;
#34505 = DIRECTION ( 'NONE',  ( -0.6427681459581293666, -0.7660444431189770143, -0.005002170337467561935 ) ) ;
#34506 = CARTESIAN_POINT ( 'NONE',  ( -11.67244013076689946, 0.000000000000000000, 11.50401908778467863 ) ) ;
#34507 = ADVANCED_FACE ( 'NONE', ( #14182 ), #53354, .F. ) ;
#34508 = LINE ( 'NONE', #51821, #7794 ) ;
#34509 = LINE ( 'NONE', #39895, #38687 ) ;
#34510 = VECTOR ( 'NONE', #33532, 1000.000000000000114 ) ;
#34511 = ADVANCED_FACE ( 'NONE', ( #14450 ), #35451, .F. ) ;
#34512 = EDGE_LOOP ( 'NONE', ( #24157, #40611, #52095, #32945 ) ) ;
#34513 = ORIENTED_EDGE ( 'NONE', *, *, #2183, .F. ) ;
#34514 = ADVANCED_FACE ( 'NONE', ( #5371 ), #31193, .F. ) ;
#34515 = CARTESIAN_POINT ( 'NONE',  ( -8.578754870427481194, 0.000000000000000000, 6.230973550731281563 ) ) ;
#34516 = CARTESIAN_POINT ( 'NONE',  ( -17.86312967602380652, 2.229229656569006401, 3.549453834752706705 ) ) ;
#34517 = DIRECTION ( 'NONE',  ( -0.9999697198139514409, -0.000000000000000000, -0.007781995580013368816 ) ) ;
#34518 = ADVANCED_FACE ( 'NONE', ( #27493 ), #27897, .F. ) ;
#34519 = CARTESIAN_POINT ( 'NONE',  ( -22.03895693409927858, 19.66185913055325685, -4.421689025564675468 ) ) ;
#34520 = DIRECTION ( 'NONE',  ( -0.7660212471507179544, -0.6427876096865405842, -0.005961354470445141482 ) ) ;
#34521 = DIRECTION ( 'NONE',  ( -0.005002170337468016433, -0.7660444431189770143, 0.6427681459581293666 ) ) ;
#34522 = DIRECTION ( 'NONE',  ( -0.005961354470445682716, -0.6427876096865404731, 0.7660212471507180654 ) ) ;
#34523 = EDGE_CURVE ( 'NONE', #38038, #18836, #51863, .T. ) ;
#34524 = B_SPLINE_CURVE_WITH_KNOTS ( 'NONE', 3,
 ( #53796, #19437, #6392, #45842, #10919, #49262 ),
 .UNSPECIFIED., .F., .F.,
 ( 4, 2, 4 ),
 ( 0.000000000000000000, 0.5000000000000000000, 1.000000000000000000 ),
 .UNSPECIFIED. ) ;
#34525 = ORIENTED_EDGE ( 'NONE', *, *, #44838, .F. ) ;
#34526 = LINE ( 'NONE', #34813, #33227 ) ;
#34527 = LINE ( 'NONE', #35655, #15161 ) ;
#34528 = ORIENTED_EDGE ( 'NONE', *, *, #52367, .T. ) ;
#34529 = CARTESIAN_POINT ( 'NONE',  ( 2.072287782118878319, 0.000000000000000000, -2.950529333540147015 ) ) ;
#34530 = VERTEX_POINT ( 'NONE', #55565 ) ;
#34531 = LINE ( 'NONE', #4171, #44921 ) ;
#34532 = ORIENTED_EDGE ( 'NONE', *, *, #21644, .F. ) ;
#34533 = VECTOR ( 'NONE', #23852, 999.9999999999998863 ) ;
#34534 = ORIENTED_EDGE ( 'NONE', *, *, #6342, .T. ) ;
#34535 = ORIENTED_EDGE ( 'NONE', *, *, #10794, .F. ) ;
#34536 = ORIENTED_EDGE ( 'NONE', *, *, #18085, .T. ) ;
#34537 = VERTEX_POINT ( 'NONE', #21208 ) ;
#34538 = ORIENTED_EDGE ( 'NONE', *, *, #38593, .F. ) ;
#34539 = DIRECTION ( 'NONE',  ( -0.5364919789714478471, 0.6444004775717705469, -0.5449076811759709926 ) ) ;
#34540 = FACE_OUTER_BOUND ( 'NONE', #17815, .T. ) ;
#34541 = CARTESIAN_POINT ( 'NONE',  ( -7.860905869600908424, 1.712176620043476140E-14, 2.600000000000000089 ) ) ;
#34542 = AXIS2_PLACEMENT_3D ( 'NONE', #11077, #50264, #50815 ) ;
#34543 = VERTEX_POINT ( 'NONE', #55872 ) ;
#34544 = PLANE ( 'NONE',  #40350 ) ;
#34545 = VERTEX_POINT ( 'NONE', #30855 ) ;
#34546 = PLANE ( 'NONE',  #25907 ) ;
#34547 = ORIENTED_EDGE ( 'NONE', *, *, #7928, .T. ) ;
#34548 = VECTOR ( 'NONE', #26626, 1000.000000000000000 ) ;
#34549 = DIRECTION ( 'NONE',  ( 0.9999697198139515519, 0.000000000000000000, 0.007781995580013368816 ) ) ;
#34550 = FACE_OUTER_BOUND ( 'NONE', #1714, .T. ) ;
#34551 = EDGE_LOOP ( 'NONE', ( #31274, #5297, #2808, #13206 ) ) ;
#34552 = CARTESIAN_POINT ( 'NONE',  ( -11.87243407472968926, 0.000000000000000000, 11.50246268866867361 ) ) ;
#34553 = ORIENTED_EDGE ( 'NONE', *, *, #10620, .T. ) ;
#34554 = ADVANCED_FACE ( 'NONE', ( #16974 ), #12981, .F. ) ;
#34555 = ADVANCED_FACE ( 'NONE', ( #43373 ), #3884, .F. ) ;
#34556 = CARTESIAN_POINT ( 'NONE',  ( -11.69649624729248316, 2.067327705546507133, 4.817474438081196908 ) ) ;
#34557 = DIRECTION ( 'NONE',  ( -0.7660212471507179544, -0.6427876096865405842, -0.005961354470445141482 ) ) ;
#34558 = EDGE_CURVE ( 'NONE', #43904, #13447, #39095, .T. ) ;
#34559 = CYLINDRICAL_SURFACE ( 'NONE', #32407, 0.5000000000000004441 ) ;
#34560 = DIRECTION ( 'NONE',  ( 0.9999697198139515519, 0.000000000000000000, 0.007781995580013368816 ) ) ;
#34561 = DIRECTION ( 'NONE',  ( 0.005961354470445682716, -0.6427876096865404731, -0.7660212471507180654 ) ) ;
#34562 = DIRECTION ( 'NONE',  ( -0.6427681459581293666, -0.7660444431189770143, -0.005002170337467561935 ) ) ;
#34563 = CARTESIAN_POINT ( 'NONE',  ( -17.74560456716937296, 0.000000000000000000, 3.774316574337878372 ) ) ;
#34564 = CARTESIAN_POINT ( 'NONE',  ( -66.64009219722507282, -11.34960557684216020, -2.652841686095987139 ) ) ;
#34565 = EDGE_LOOP ( 'NONE', ( #13583, #47610, #47572, #55713 ) ) ;
#34566 = CARTESIAN_POINT ( 'NONE',  ( -12.06579791175127525, 0.000000000000000000, 2.341189863830586582 ) ) ;
#34567 = ORIENTED_EDGE ( 'NONE', *, *, #43848, .F. ) ;
#34568 = VECTOR ( 'NONE', #35183, 1000.000000000000000 ) ;
#34569 = VECTOR ( 'NONE', #43433, 1000.000000000000000 ) ;
#34570 = CARTESIAN_POINT ( 'NONE',  ( -69.43545830293986398, -9.790829293527439248, 7.501778215771295777 ) ) ;
#34571 = DIRECTION ( 'NONE',  ( -0.5364919789714478471, 0.6444004775717705469, -0.5449076811759709926 ) ) ;
#34572 = DIRECTION ( 'NONE',  ( -0.6427681459581293666, -0.7660444431189770143, -0.005002170337467561935 ) ) ;
#34573 = CARTESIAN_POINT ( 'NONE',  ( -19.16331067184377801, -0.1191753592594172323, 5.879273048348689024 ) ) ;
#34574 = CARTESIAN_POINT ( 'NONE',  ( -18.31888538305858916, 0.000000000000000000, 3.939181184056494089 ) ) ;
#34575 = CARTESIAN_POINT ( 'NONE',  ( -50.02554558092695913, 3.776013638374817294, 5.000000000000000000 ) ) ;
#34576 = FACE_OUTER_BOUND ( 'NONE', #29815, .T. ) ;
#34577 = ITEM_DEFINED_TRANSFORMATION ( 'NONE', 'NONE', #55268,  #2610 ) ;
#34578 = ORIENTED_EDGE ( 'NONE', *, *, #49239, .F. ) ;
#34579 = LINE ( 'NONE', #17549, #25701 ) ;
#34580 = DIRECTION ( 'NONE',  ( 0.005961354470445682716, -0.6427876096865404731, -0.7660212471507180654 ) ) ;
#34581 = LINE ( 'NONE', #22091, #19139 ) ;
#34582 = EDGE_CURVE ( 'NONE', #5827, #35406, #52444, .T. ) ;
#34583 = LINE ( 'NONE', #789, #38210 ) ;
#34584 = DIRECTION ( 'NONE',  ( -0.5449076811759708816, 0.6444004775717707689, 0.5364919789714475140 ) ) ;
#34585 = EDGE_CURVE ( 'NONE', #18526, #36044, #47323, .T. ) ;
#34586 = CARTESIAN_POINT ( 'NONE',  ( -29.86274838104827367, -0.1191753592594197858, 8.381332038739175871 ) ) ;
#34587 = FACE_OUTER_BOUND ( 'NONE', #969, .T. ) ;
#34588 = AXIS2_PLACEMENT_3D ( 'NONE', #55941, #51091, #13047 ) ;
#34589 = FACE_OUTER_BOUND ( 'NONE', #43501, .T. ) ;
#34590 = LINE ( 'NONE', #212, #35977 ) ;
#34591 = EDGE_CURVE ( 'NONE', #18, #13860, #1906, .T. ) ;
#34592 = ORIENTED_EDGE ( 'NONE', *, *, #48709, .T. ) ;
#34593 = LINE ( 'NONE', #13326, #48263 ) ;
#34594 = EDGE_CURVE ( 'NONE', #31864, #26534, #56143, .T. ) ;
#34595 = ORIENTED_EDGE ( 'NONE', *, *, #33631, .T. ) ;
#34596 = ADVANCED_FACE ( 'NONE', ( #30018 ), #17230, .F. ) ;
#34597 = ORIENTED_EDGE ( 'NONE', *, *, #3914, .T. ) ;
#34598 = EDGE_LOOP ( 'NONE', ( #9976, #48674, #7122, #55217 ) ) ;
#34599 = ORIENTED_EDGE ( 'NONE', *, *, #25176, .T. ) ;
#34600 = EDGE_LOOP ( 'NONE', ( #29701, #15216, #20686, #11350 ) ) ;
#34601 = DIRECTION ( 'NONE',  ( -0.6427681459581293666, -0.7660444431189770143, -0.005002170337467561935 ) ) ;
#34602 = LINE ( 'NONE', #18402, #27605 ) ;
#34603 = VECTOR ( 'NONE', #12092, 1000.000000000000227 ) ;
#34604 = VECTOR ( 'NONE', #55292, 999.9999999999998863 ) ;
#34605 = ORIENTED_EDGE ( 'NONE', *, *, #18198, .T. ) ;
#34606 = VECTOR ( 'NONE', #4442, 1000.000000000000227 ) ;
#34607 = CARTESIAN_POINT ( 'NONE',  ( 2.072287782118878319, 0.000000000000000000, -2.950529333540147015 ) ) ;
#34608 = ORIENTED_EDGE ( 'NONE', *, *, #32486, .F. ) ;
#34609 = LINE ( 'NONE', #51927, #37294 ) ;
#34610 = LINE ( 'NONE', #16743, #34999 ) ;
#34611 = ORIENTED_EDGE ( 'NONE', *, *, #29677, .F. ) ;
#34612 = CARTESIAN_POINT ( 'NONE',  ( -13.63673279712320507, -0.1191753592594197858, 12.22739664767016521 ) ) ;
#34614 = ORIENTED_EDGE ( 'NONE', *, *, #43984, .T. ) ;
#34613 = ADVANCED_FACE ( 'NONE', ( #25758 ), #26594, .F. ) ;
#34615 = CARTESIAN_POINT ( 'NONE',  ( -19.12962290826653700, 0.000000000000000000, 14.40064212555863854 ) ) ;
#34616 = VECTOR ( 'NONE', #43376, 1000.000000000000227 ) ;
#34617 = EDGE_CURVE ( 'NONE', #30608, #3673, #48160, .T. ) ;
#34618 = EDGE_CURVE ( 'NONE', #19103, #50804, #4199, .T. ) ;
#34619 = VECTOR ( 'NONE', #50746, 999.9999999999998863 ) ;
#34620 = CARTESIAN_POINT ( 'NONE',  ( -16.76521749764649982, 0.000000000000000000, 9.121921164085227574 ) ) ;
#34621 = ORIENTED_EDGE ( 'NONE', *, *, #52757, .T. ) ;
#34622 = DIRECTION ( 'NONE',  ( 0.000000000000000000, -0.000000000000000000, -1.000000000000000000 ) ) ;
#34623 = CARTESIAN_POINT ( 'NONE',  ( -16.81190032086591302, 0.000000000000000000, 3.212244750653343583 ) ) ;
#34624 = CARTESIAN_POINT ( 'NONE',  ( -13.53673582514181106, 0.000000000000000000, 12.22817484722816772 ) ) ;
#34625 = LINE ( 'NONE', #38325, #5674 ) ;
#34626 = ORIENTED_EDGE ( 'NONE', *, *, #43840, .F. ) ;
#34627 = CARTESIAN_POINT ( 'NONE',  ( -15.53549445463335488, 0.000000000000000000, 4.530180301885105010 ) ) ;
#34628 = DIRECTION ( 'NONE',  ( 0.9999697198139515519, 0.000000000000000000, 0.007781995580013368816 ) ) ;
#34629 = FACE_OUTER_BOUND ( 'NONE', #45202, .T. ) ;
#34630 = LINE ( 'NONE', #48241, #2373 ) ;
#34631 = DIRECTION ( 'NONE',  ( 0.007781995580012662783, 0.000000000000000000, -0.9999697198139514409 ) ) ;
#34632 = CARTESIAN_POINT ( 'NONE',  ( -6.110905869600904872, 1.712176620043476140E-14, -4.599999999999999645 ) ) ;
#34633 = LINE ( 'NONE', #43449, #49729 ) ;
#34634 = ADVANCED_FACE ( 'NONE', ( #35149 ), #8745, .F. ) ;
#34635 = CARTESIAN_POINT ( 'NONE',  ( -16.53317331066696383, 0.000000000000000000, 13.31285208727739899 ) ) ;
#34636 = CARTESIAN_POINT ( 'NONE',  ( 0.09621548157177385596, -1.683565401097096181, -2.125000000000000444 ) ) ;
#34637 = ORIENTED_EDGE ( 'NONE', *, *, #21277, .T. ) ;
#34638 = CARTESIAN_POINT ( 'NONE',  ( 0.000000000000000000, 0.000000000000000000, 0.000000000000000000 ) ) ;
#34639 = LINE ( 'NONE', #26687, #49573 ) ;
#34640 = ORIENTED_EDGE ( 'NONE', *, *, #32062, .T. ) ;
#34641 = LINE ( 'NONE', #585, #30209 ) ;
#34642 = CARTESIAN_POINT ( 'NONE',  ( -12.60458797795435615, 0.000000000000000000, 11.86609696750642229 ) ) ;
#34643 = AXIS2_PLACEMENT_3D ( 'NONE', #55077, #11884, #55331 ) ;
#34644 = AXIS2_PLACEMENT_3D ( 'NONE', #22694, #39752, #45133 ) ;
#34645 = CARTESIAN_POINT ( 'NONE',  ( -14.94760462649100496, 0.000000000000000000, 2.488088991209854051 ) ) ;
#34646 = EDGE_CURVE ( 'NONE', #27953, #36809, #38240, .T. ) ;
#34647 = CARTESIAN_POINT ( 'NONE',  ( -12.84690689054629154, -1.489407457353159048, 1.823976140470426444 ) ) ;
#34648 = DIRECTION ( 'NONE',  ( 0.6427681459581294776, -0.7660444431189769032, 0.005002170337467562802 ) ) ;
#34649 = ORIENTED_EDGE ( 'NONE', *, *, #27903, .T. ) ;
#34650 = VECTOR ( 'NONE', #9663, 1000.000000000000227 ) ;
#34651 = ORIENTED_EDGE ( 'NONE', *, *, #32956, .F. ) ;
#34652 = EDGE_CURVE ( 'NONE', #27029, #39457, #16670, .T. ) ;
#34653 = FACE_OUTER_BOUND ( 'NONE', #12086, .T. ) ;
#34654 = CARTESIAN_POINT ( 'NONE',  ( -12.13851405436063047, 0.000000000000000000, 11.68505802764555135 ) ) ;
#34655 = ORIENTED_EDGE ( 'NONE', *, *, #54063, .T. ) ;
#34656 = PLANE ( 'NONE',  #1187 ) ;
#34657 = EDGE_LOOP ( 'NONE', ( #32104, #43461, #41004, #47685 ) ) ;
#34658 = PLANE ( 'NONE',  #54879 ) ;
#34659 = ADVANCED_FACE ( 'NONE', ( #39385 ), #12439, .F. ) ;
#34660 = AXIS2_PLACEMENT_3D ( 'NONE', #22900, #18081, #30859 ) ;
#34661 = ORIENTED_EDGE ( 'NONE', *, *, #3965, .T. ) ;
#34662 = LINE ( 'NONE', #13097, #20195 ) ;
#34663 = ORIENTED_EDGE ( 'NONE', *, *, #11076, .T. ) ;
#34664 = ORIENTED_EDGE ( 'NONE', *, *, #5494, .F. ) ;
#34665 = VERTEX_POINT ( 'NONE', #35997 ) ;
#34666 = PLANE ( 'NONE',  #49294 ) ;
#34667 = DIRECTION ( 'NONE',  ( 0.005961354470445682716, -0.6427876096865404731, -0.7660212471507180654 ) ) ;
#34668 = DIRECTION ( 'NONE',  ( 0.005961354470445682716, -0.6427876096865404731, -0.7660212471507180654 ) ) ;
#34669 = EDGE_CURVE ( 'NONE', #9132, #28372, #27737, .T. ) ;
#34670 = CARTESIAN_POINT ( 'NONE',  ( -17.73140113748535285, 0.000000000000000000, 13.85752530597602039 ) ) ;
#34671 = ORIENTED_EDGE ( 'NONE', *, *, #34073, .T. ) ;
#34672 = ORIENTED_EDGE ( 'NONE', *, *, #24608, .F. ) ;
#34673 = VECTOR ( 'NONE', #40394, 1000.000000000000227 ) ;
#34674 = ADVANCED_FACE ( 'NONE', ( #22363 ), #13806, .F. ) ;
#34675 = EDGE_CURVE ( 'NONE', #47218, #18585, #53304, .T. ) ;
#34676 = ORIENTED_EDGE ( 'NONE', *, *, #47103, .F. ) ;
#34677 = CARTESIAN_POINT ( 'NONE',  ( -13.66832470675316635, 0.000000000000000000, 3.436714839183848458 ) ) ;
#34678 = VERTEX_POINT ( 'NONE', #49597 ) ;
#34679 = AXIS2_PLACEMENT_3D ( 'NONE', #49761, #2026, #49187 ) ;
#34680 = CARTESIAN_POINT ( 'NONE',  ( -21.47263955680318404, 0.000000000000000000, 5.022634149262071190 ) ) ;
#34681 = EDGE_CURVE ( 'NONE', #2187, #21767, #14940, .T. ) ;
#34682 = ORIENTED_EDGE ( 'NONE', *, *, #3906, .F. ) ;
#34683 = CARTESIAN_POINT ( 'NONE',  ( -18.72454025655023813, -0.1191753592594158168, 9.206676289436575900 ) ) ;
#34684 = CARTESIAN_POINT ( 'NONE',  ( -23.33849165029409889, 0.000000000000000000, 5.946783852668351855 ) ) ;
#34685 = VECTOR ( 'NONE', #49052, 999.9999999999998863 ) ;
#34686 = AXIS2_PLACEMENT_3D ( 'NONE', #2987, #3296, #29116 ) ;
#34687 = EDGE_LOOP ( 'NONE', ( #21444, #36239, #56085, #36935 ) ) ;
#34688 = EDGE_CURVE ( 'NONE', #34917, #27150, #31443, .T. ) ;
#34689 = DIRECTION ( 'NONE',  ( -0.005002170337468016433, -0.7660444431189770143, 0.6427681459581293666 ) ) ;
#34690 = ORIENTED_EDGE ( 'NONE', *, *, #27536, .F. ) ;
#34691 = EDGE_CURVE ( 'NONE', #39023, #1495, #53829, .T. ) ;
#34692 = VECTOR ( 'NONE', #8793, 1000.000000000000227 ) ;
#34693 = CARTESIAN_POINT ( 'NONE',  ( -58.00000000000000711, -9.333333333333333925, 7.102951435054649637E-15 ) ) ;
#34694 = VECTOR ( 'NONE', #2514, 999.9999999999998863 ) ;
#34695 = ORIENTED_EDGE ( 'NONE', *, *, #36075, .F. ) ;
#34696 = LINE ( 'NONE', #30467, #34090 ) ;
#34697 = CARTESIAN_POINT ( 'NONE',  ( -23.33693525117809386, 0.000000000000000000, 5.746789908705562944 ) ) ;
#34698 = LINE ( 'NONE', #29894, #9236 ) ;
#34699 = ORIENTED_EDGE ( 'NONE', *, *, #38991, .F. ) ;
#34700 = EDGE_CURVE ( 'NONE', #55928, #17587, #48456, .T. ) ;
#34701 = LINE ( 'NONE', #21914, #16606 ) ;
#34702 = ADVANCED_FACE ( 'NONE', ( #22625 ), #40524, .F. ) ;
#34703 = CARTESIAN_POINT ( 'NONE',  ( -10.00813838035478298, 0.000000000000000000, 10.77830692922518452 ) ) ;
#34704 = CARTESIAN_POINT ( 'NONE',  ( -9.908141408373387193, -0.1191753592594197858, 10.77908512878318703 ) ) ;
#34705 = DIRECTION ( 'NONE',  ( 0.5449076811759707706, 0.6444004775717708799, -0.5364919789714476250 ) ) ;
#34706 = VECTOR ( 'NONE', #16810, 1000.000000000000000 ) ;
#34707 = CARTESIAN_POINT ( 'NONE',  ( 2.072287782118878319, 0.000000000000000000, -2.950529333540147015 ) ) ;
#34708 = CARTESIAN_POINT ( 'NONE',  ( -24.26908309836554878, 0.000000000000000000, 6.108867788427308376 ) ) ;
#34709 = ADVANCED_FACE ( 'NONE', ( #26898 ), #6167, .F. ) ;
#34710 = DIRECTION ( 'NONE',  ( 0.5364919789714477361, 0.6444004775717706579, 0.5449076811759711036 ) ) ;
#34711 = VERTEX_POINT ( 'NONE', #14656 ) ;
#34712 = FACE_OUTER_BOUND ( 'NONE', #33624, .T. ) ;
#34713 = LINE ( 'NONE', #52030, #34962 ) ;
#34714 = CARTESIAN_POINT ( 'NONE',  ( -27.06552663992790997, 0.000000000000000000, 7.195101427592543786 ) ) ;
#34715 = EDGE_LOOP ( 'NONE', ( #53506, #14018, #25172, #37403 ) ) ;
#34716 = DIRECTION ( 'NONE',  ( 0.007781995580012662783, 0.000000000000000000, -0.9999697198139514409 ) ) ;
#34717 = PLANE ( 'NONE',  #34082 ) ;
#34718 = ORIENTED_EDGE ( 'NONE', *, *, #45213, .F. ) ;
#34719 = AXIS2_PLACEMENT_3D ( 'NONE', #29761, #10115, #14116 ) ;
#34720 = CARTESIAN_POINT ( 'NONE',  ( -17.73140113748535285, 0.000000000000000000, 13.85752530597602039 ) ) ;
#34721 = DIRECTION ( 'NONE',  ( 0.9999697198139515519, 0.000000000000000000, 0.007781995580013368816 ) ) ;
#34722 = VECTOR ( 'NONE', #38075, 999.9999999999998863 ) ;
#34723 = FACE_OUTER_BOUND ( 'NONE', #36846, .T. ) ;
#34724 = CARTESIAN_POINT ( 'NONE',  ( -69.24559741778114130, 0.1329209457098951275, 6.496570960379585813 ) ) ;
#34725 = ORIENTED_EDGE ( 'NONE', *, *, #17283, .F. ) ;
#34726 = ORIENTED_EDGE ( 'NONE', *, *, #50958, .T. ) ;
#34727 = FACE_OUTER_BOUND ( 'NONE', #9904, .T. ) ;
#34728 = DIRECTION ( 'NONE',  ( 0.5449076811759707706, 0.6444004775717708799, -0.5364919789714476250 ) ) ;
#34729 = VECTOR ( 'NONE', #4317, 1000.000000000000227 ) ;
#34730 = LINE ( 'NONE', #34454, #38666 ) ;
#34731 = VECTOR ( 'NONE', #6138, 999.9999999999998863 ) ;
#34732 = CARTESIAN_POINT ( 'NONE',  ( -15.96710241509184058, -0.1191753592594218814, 13.13259134697452879 ) ) ;
#34733 = AXIS2_PLACEMENT_3D ( 'NONE', #10659, #37034, #11171 ) ;
#34734 = FACE_OUTER_BOUND ( 'NONE', #48754, .T. ) ;
#34735 = LINE ( 'NONE', #9760, #26709 ) ;
#34736 = EDGE_CURVE ( 'NONE', #44414, #49377, #35400, .T. ) ;
#34737 = EDGE_LOOP ( 'NONE', ( #45122, #53149, #27855, #46468 ) ) ;
#34738 = CYLINDRICAL_SURFACE ( 'NONE', #50074, 1.750000000000003331 ) ;
#34739 = VECTOR ( 'NONE', #35969, 1000.000000000000114 ) ;
#34740 = DIRECTION ( 'NONE',  ( -0.5364919789714478471, 0.6444004775717705469, -0.5449076811759709926 ) ) ;
#34741 = VECTOR ( 'NONE', #39257, 1000.000000000000114 ) ;
#34742 = VERTEX_POINT ( 'NONE', #9574 ) ;
#34743 = DIRECTION ( 'NONE',  ( -0.5364919789714478471, 0.6444004775717705469, -0.5449076811759709926 ) ) ;
#34744 = LINE ( 'NONE', #48931, #54035 ) ;
#34745 = LINE ( 'NONE', #12884, #53818 ) ;
#34746 = ADVANCED_FACE ( 'NONE', ( #44756 ), #18345, .F. ) ;
#34747 = VERTEX_POINT ( 'NONE', #48758 ) ;
#34748 = CARTESIAN_POINT ( 'NONE',  ( -10.23156040681847045, 0.000000000000000000, 5.479446896259717370 ) ) ;
#34749 = VECTOR ( 'NONE', #17594, 1000.000000000000114 ) ;
#34750 = ORIENTED_EDGE ( 'NONE', *, *, #26458, .F. ) ;
#34751 = ADVANCED_FACE ( 'NONE', ( #9857 ), #52704, .F. ) ;
#34752 = VECTOR ( 'NONE', #48748, 1000.000000000000114 ) ;
#34753 = EDGE_CURVE ( 'NONE', #883, #49206, #14399, .T. ) ;
#34754 = ORIENTED_EDGE ( 'NONE', *, *, #37201, .F. ) ;
#34755 = ORIENTED_EDGE ( 'NONE', *, *, #43529, .F. ) ;
#34756 = EDGE_LOOP ( 'NONE', ( #40762, #24697, #4913, #53966 ) ) ;
#34757 = CARTESIAN_POINT ( 'NONE',  ( -23.66772770479517618, 18.99370688441070953, 4.503109509781816122 ) ) ;
#34758 = ORIENTED_EDGE ( 'NONE', *, *, #27351, .F. ) ;
#34759 = VECTOR ( 'NONE', #39617, 1000.000000000000227 ) ;
#34760 = CARTESIAN_POINT ( 'NONE',  ( -11.13054826722768098, 24.50000000000005684, -3.000000000000000000 ) ) ;
#34761 = ORIENTED_EDGE ( 'NONE', *, *, #44278, .T. ) ;
#34762 = LINE ( 'NONE', #52918, #33143 ) ;
#34763 = ADVANCED_FACE ( 'NONE', ( #22893 ), #44467, .F. ) ;
#34764 = ORIENTED_EDGE ( 'NONE', *, *, #6882, .F. ) ;
#34765 = FACE_OUTER_BOUND ( 'NONE', #3541, .T. ) ;
#34766 = VECTOR ( 'NONE', #36697, 1000.000000000000227 ) ;
#34767 = EDGE_LOOP ( 'NONE', ( #55339, #29409, #18603, #5415 ) ) ;
#34768 = EDGE_CURVE ( 'NONE', #28225, #12315, #40220, .T. ) ;
#34769 = PLANE ( 'NONE',  #49273 ) ;
#34770 = CARTESIAN_POINT ( 'NONE',  ( -9.542064456761055524, 0.000000000000000000, 10.59726798936431180 ) ) ;
#34771 = DIRECTION ( 'NONE',  ( 0.7660212471507180654, -0.6427876096865404731, 0.005961354470445141482 ) ) ;
#34772 = CARTESIAN_POINT ( 'NONE',  ( -22.40634380310664397, 0.000000000000000000, 5.584705972946605534 ) ) ;
#34773 = AXIS2_PLACEMENT_3D ( 'NONE', #51776, #25665, #29933 ) ;
#34774 = LINE ( 'NONE', #43844, #38305 ) ;
#34775 = EDGE_LOOP ( 'NONE', ( #30360, #44319, #37180, #19879 ) ) ;
#34776 = CIRCLE ( 'NONE', #52932, 6.000000000000001776 ) ;
#34777 = EDGE_CURVE ( 'NONE', #46860, #55008, #33634, .T. ) ;
#34778 = VECTOR ( 'NONE', #20097, 1000.000000000000227 ) ;
#34779 = VERTEX_POINT ( 'NONE', #24850 ) ;
#34780 = LINE ( 'NONE', #4963, #8651 ) ;
#34781 = PLANE ( 'NONE',  #3994 ) ;
#34782 = CARTESIAN_POINT ( 'NONE',  ( -16.53317331066696383, 0.000000000000000000, 13.31285208727739899 ) ) ;
#34783 = EDGE_CURVE ( 'NONE', #30486, #9050, #24552, .T. ) ;
#34784 = VECTOR ( 'NONE', #17089, 1000.000000000000114 ) ;
#34785 = AXIS2_PLACEMENT_3D ( 'NONE', #22089, #13571, #30881 ) ;
#34786 = CARTESIAN_POINT ( 'NONE',  ( -11.59541290789961998, 0.000000000000000000, 1.606186369083069332 ) ) ;
#34787 = DIRECTION ( 'NONE',  ( 0.007781995580012663651, 0.000000000000000000, -0.9999697198139515519 ) ) ;
#34788 = DIRECTION ( 'NONE',  ( 0.000000000000000000, -0.000000000000000000, -1.000000000000000000 ) ) ;
#34789 = ORIENTED_EDGE ( 'NONE', *, *, #13393, .F. ) ;
#34790 = DIRECTION ( 'NONE',  ( -0.005002170337468016433, -0.7660444431189770143, 0.6427681459581293666 ) ) ;
#34791 = DIRECTION ( 'NONE',  ( -0.6427681459581293666, -0.7660444431189770143, -0.005002170337467561935 ) ) ;
#34792 = VERTEX_POINT ( 'NONE', #7520 ) ;
#34793 = DIRECTION ( 'NONE',  ( 0.7660212471507180654, -0.6427876096865404731, 0.005961354470445141482 ) ) ;
#34794 = PLANE ( 'NONE',  #36022 ) ;
#34795 = CARTESIAN_POINT ( 'NONE',  ( -14.12433944307840861, 0.000000000000000000, 2.325169817642546821 ) ) ;
#34796 = CARTESIAN_POINT ( 'NONE',  ( -17.49039288222042998, 0.1245042932765029059, 3.471821964380750192 ) ) ;
#34797 = CARTESIAN_POINT ( 'NONE',  ( 2.072287782118878319, 0.000000000000000000, -2.950529333540147015 ) ) ;
#34798 = EDGE_LOOP ( 'NONE', ( #42764, #49261, #45031, #36946 ) ) ;
#34799 = VECTOR ( 'NONE', #27569, 1000.000000000000227 ) ;
#34800 = ORIENTED_EDGE ( 'NONE', *, *, #20617, .F. ) ;
#34801 = FACE_OUTER_BOUND ( 'NONE', #19491, .T. ) ;
#34802 = CARTESIAN_POINT ( 'NONE',  ( -16.43317633868556626, -0.1191753592594197858, 13.31363028683540151 ) ) ;
#34803 = LINE ( 'NONE', #17780, #7948 ) ;
#34804 = EDGE_CURVE ( 'NONE', #25674, #19445, #16063, .T. ) ;
#34805 = VECTOR ( 'NONE', #7598, 1000.000000000000000 ) ;
#34806 = DIRECTION ( 'NONE',  ( 0.5449076811759707706, 0.6444004775717708799, -0.5364919789714476250 ) ) ;
#34807 = LINE ( 'NONE', #52963, #29432 ) ;
#34808 = EDGE_CURVE ( 'NONE', #21782, #35835, #50110, .T. ) ;
#34809 = VECTOR ( 'NONE', #185, 999.9999999999998863 ) ;
#34810 = LINE ( 'NONE', #18615, #54535 ) ;
#34811 = LINE ( 'NONE', #52674, #43802 ) ;
#34812 = VERTEX_POINT ( 'NONE', #32800 ) ;
#34813 = CARTESIAN_POINT ( 'NONE',  ( -17.03126345885748449, 4.010151117816511679, 3.169508026948365309 ) ) ;
#34814 = LINE ( 'NONE', #13249, #36930 ) ;
#34815 = EDGE_CURVE ( 'NONE', #7643, #43820, #15232, .T. ) ;
#34816 = ADVANCED_FACE ( 'NONE', ( #7248 ), #15757, .F. ) ;
#34817 = VECTOR ( 'NONE', #52296, 999.9999999999998863 ) ;
#34818 = ORIENTED_EDGE ( 'NONE', *, *, #36328, .F. ) ;
#34819 = DIRECTION ( 'NONE',  ( -0.9999697198139514409, -0.000000000000000000, -0.007781995580013368816 ) ) ;
#34820 = VERTEX_POINT ( 'NONE', #28008 ) ;
#34821 = CARTESIAN_POINT ( 'NONE',  ( -18.86354292863559579, 0.000000000000000000, 14.21804678658176080 ) ) ;
#34822 = EDGE_CURVE ( 'NONE', #45853, #48933, #11527, .T. ) ;
#34823 = ADVANCED_FACE ( 'NONE', ( #10946 ), #28844, .F. ) ;
#34824 = CARTESIAN_POINT ( 'NONE',  ( -30.79411802867772607, 0.000000000000000000, 8.643412946479525516 ) ) ;
#34825 = EDGE_CURVE ( 'NONE', #50938, #37343, #24297, .T. ) ;
#34826 = VECTOR ( 'NONE', #25844, 999.9999999999998863 ) ;
#34827 = ORIENTED_EDGE ( 'NONE', *, *, #26977, .F. ) ;
#34828 = VERTEX_POINT ( 'NONE', #16315 ) ;
#34829 = VECTOR ( 'NONE', #15052, 1000.000000000000114 ) ;
#34830 = ORIENTED_EDGE ( 'NONE', *, *, #39394, .T. ) ;
#34831 = VERTEX_POINT ( 'NONE', #54379 ) ;
#34832 = AXIS2_PLACEMENT_3D ( 'NONE', #49624, #36847, #53856 ) ;
#34833 = ORIENTED_EDGE ( 'NONE', *, *, #17019, .T. ) ;
#34834 = VERTEX_POINT ( 'NONE', #32545 ) ;
#34835 = DIRECTION ( 'NONE',  ( 0.007781995580012663651, 0.000000000000000000, -0.9999697198139515519 ) ) ;
#34836 = CARTESIAN_POINT ( 'NONE',  ( -19.26540349777245353, 0.000000000000000000, 6.147807580067062183 ) ) ;
#34837 = LINE ( 'NONE', #38826, #6808 ) ;
#34838 = EDGE_LOOP ( 'NONE', ( #7164, #56202, #417, #14029 ) ) ;
#34839 = DIRECTION ( 'NONE',  ( 0.9999697198139515519, 0.000000000000000000, 0.007781995580013368816 ) ) ;
#34840 = EDGE_CURVE ( 'NONE', #5501, #53603, #23725, .T. ) ;
#34841 = ORIENTED_EDGE ( 'NONE', *, *, #37121, .T. ) ;
#34842 = ORIENTED_EDGE ( 'NONE', *, *, #48806, .T. ) ;
#34843 = EDGE_CURVE ( 'NONE', #5277, #27412, #46407, .T. ) ;
#34844 = VECTOR ( 'NONE', #49141, 1000.000000000000000 ) ;
#34845 = DIRECTION ( 'NONE',  ( 0.9999697198139515519, 0.000000000000000000, 0.007781995580013368816 ) ) ;
#34846 = VECTOR ( 'NONE', #19092, 1000.000000000000227 ) ;
#34847 = FACE_OUTER_BOUND ( 'NONE', #54395, .T. ) ;
#34848 = ADVANCED_FACE ( 'NONE', ( #20607 ), #45578, .F. ) ;
#34849 = DIRECTION ( 'NONE',  ( -0.005002170337468016433, -0.7660444431189770143, 0.6427681459581293666 ) ) ;
#34850 = ORIENTED_EDGE ( 'NONE', *, *, #46601, .F. ) ;
#34851 = DIRECTION ( 'NONE',  ( 0.9321478471874540261, 0.000000000000000000, -0.3620778797217457101 ) ) ;
#34852 = VECTOR ( 'NONE', #32207, 999.9999999999998863 ) ;
#34853 = EDGE_LOOP ( 'NONE', ( #49673, #47955, #33547, #358 ) ) ;
#34854 = EDGE_CURVE ( 'NONE', #14573, #26718, #37919, .T. ) ;
#34855 = CARTESIAN_POINT ( 'NONE',  ( -16.30618749709877591, 2.553033558614006271, 7.405161117131130233 ) ) ;
#34857 = AXIS2_PLACEMENT_3D ( 'NONE', #8434, #8162, #13542 ) ;
#34856 = DIRECTION ( 'NONE',  ( 0.005002170337468016433, -0.7660444431189770143, -0.6427681459581293666 ) ) ;
#34858 = B_SPLINE_CURVE_WITH_KNOTS ( 'NONE', 3,
 ( #54327, #25090, #37278, #32493, #49795, #10888, #28203, #45512, #23946, #6928 ),
 .UNSPECIFIED., .F., .F.,
 ( 4, 2, 2, 2, 4 ),
 ( 0.000000000000000000, 0.0003349897808261797561, 0.0006699795616523595123, 0.001004969342478539323, 0.001339959123304719025 ),
 .UNSPECIFIED. ) ;
#34859 = DIRECTION ( 'NONE',  ( -0.7660212471507179544, -0.6427876096865405842, -0.005961354470445141482 ) ) ;
#34860 = DIRECTION ( 'NONE',  ( -0.005002170337468016433, -0.7660444431189770143, 0.6427681459581293666 ) ) ;
#34861 = DIRECTION ( 'NONE',  ( 0.007781995580012662783, 0.000000000000000000, -0.9999697198139514409 ) ) ;
#34862 = CARTESIAN_POINT ( 'NONE',  ( 5.618093942130458096, -1.050357310661657939, 2.260478214906367800 ) ) ;
#34863 = FACE_OUTER_BOUND ( 'NONE', #22032, .T. ) ;
#34864 = VECTOR ( 'NONE', #22111, 1000.000000000000227 ) ;
#34865 = CARTESIAN_POINT ( 'NONE',  ( -67.55782011861325032, -8.435184460786505412, -3.909888324369926060 ) ) ;
#34866 = ORIENTED_EDGE ( 'NONE', *, *, #42834, .F. ) ;
#34867 = CARTESIAN_POINT ( 'NONE',  ( -20.54204810873173415, 0.000000000000000000, 4.860550213503115558 ) ) ;
#34868 = VECTOR ( 'NONE', #4214, 1000.000000000000227 ) ;
#34869 = LINE ( 'NONE', #52723, #31989 ) ;
#34870 = FACE_OUTER_BOUND ( 'NONE', #52059, .T. ) ;
#34871 = LINE ( 'NONE', #3910, #25395 ) ;
#34872 = DIRECTION ( 'NONE',  ( -0.7660212471507179544, -0.6427876096865405842, -0.005961354470445141482 ) ) ;
#34873 = DIRECTION ( 'NONE',  ( -0.9999697198139514409, -0.000000000000000000, -0.007781995580013368816 ) ) ;
#34874 = LINE ( 'NONE', #34575, #48611 ) ;
#34875 = VECTOR ( 'NONE', #35185, 999.9999999999998863 ) ;
#34876 = DIRECTION ( 'NONE',  ( 0.007781995580012662783, 0.000000000000000000, -0.9999697198139514409 ) ) ;
#34877 = VECTOR ( 'NONE', #3556, 999.9999999999998863 ) ;
#34878 = APPLICATION_PROTOCOL_DEFINITION ( 'draft international standard', 'automotive_design', 1998, #32927 ) ;
#34879 = ORIENTED_EDGE ( 'NONE', *, *, #55381, .T. ) ;
#34880 = DIRECTION ( 'NONE',  ( 0.6427681459581294776, -0.7660444431189769032, 0.005002170337467562802 ) ) ;
#34881 = DIRECTION ( 'NONE',  ( -0.005002170337468016433, -0.7660444431189770143, 0.6427681459581293666 ) ) ;
#34882 = CARTESIAN_POINT ( 'NONE',  ( -8.273148203881921958, 0.000000000000000000, 5.694693769082166845 ) ) ;
#34883 = LINE ( 'NONE', #47359, #45420 ) ;
#34884 = DIRECTION ( 'NONE',  ( 0.000000000000000000, -0.000000000000000000, -1.000000000000000000 ) ) ;
#34885 = EDGE_CURVE ( 'NONE', #38344, #1220, #2689, .T. ) ;
#34886 = CARTESIAN_POINT ( 'NONE',  ( -13.08934823687588889, -0.1166911823299076612, 1.865973795676008073 ) ) ;
#34887 = CARTESIAN_POINT ( 'NONE',  ( -20.18930731220519093, -2.460819163488159766, 4.645020693886293905 ) ) ;
#34888 = VECTOR ( 'NONE', #34190, 999.9999999999998863 ) ;
#34889 = DIRECTION ( 'NONE',  ( -0.7660212471507179544, -0.6427876096865405842, -0.005961354470445141482 ) ) ;
#34890 = EDGE_CURVE ( 'NONE', #9132, #55490, #55228, .T. ) ;
#34891 = PLANE ( 'NONE',  #16121 ) ;
#34892 = AXIS2_PLACEMENT_3D ( 'NONE', #8510, #38048, #30086 ) ;
#34893 = ORIENTED_EDGE ( 'NONE', *, *, #52536, .T. ) ;
#34894 = CARTESIAN_POINT ( 'NONE',  ( -14.01545677930355183, 0.000000000000000000, 2.126011111488108174 ) ) ;
#34895 = VECTOR ( 'NONE', #16844, 999.9999999999998863 ) ;
#34896 = EDGE_CURVE ( 'NONE', #38597, #21963, #2435, .T. ) ;
#34897 = EDGE_CURVE ( 'NONE', #2279, #43270, #28548, .T. ) ;
#34898 = ADVANCED_FACE ( 'NONE', ( #34238 ), #30537, .F. ) ;
#34899 = EDGE_LOOP ( 'NONE', ( #17355, #7879, #13767, #13804 ) ) ;
#34900 = AXIS2_PLACEMENT_3D ( 'NONE', #40368, #17667, #31838 ) ;
#34901 = ADVANCED_FACE ( 'NONE', ( #47552 ), #4666, .F. ) ;
#34902 = ORIENTED_EDGE ( 'NONE', *, *, #12284, .T. ) ;
#34903 = ORIENTED_EDGE ( 'NONE', *, *, #41617, .T. ) ;
#34904 = VECTOR ( 'NONE', #18946, 999.9999999999998863 ) ;
#34905 = ORIENTED_EDGE ( 'NONE', *, *, #41760, .T. ) ;
#34906 = VECTOR ( 'NONE', #35144, 999.9999999999998863 ) ;
#34907 = ORIENTED_EDGE ( 'NONE', *, *, #21508, .T. ) ;
#34908 = CARTESIAN_POINT ( 'NONE',  ( -12.33850799832341849, 0.000000000000000000, 11.68350162852954632 ) ) ;
#34909 = FACE_OUTER_BOUND ( 'NONE', #10039, .T. ) ;
#34910 = VECTOR ( 'NONE', #27891, 1000.000000000000000 ) ;
#34911 = VERTEX_POINT ( 'NONE', #4119 ) ;
#34912 = ORIENTED_EDGE ( 'NONE', *, *, #18101, .F. ) ;
#34913 = EDGE_CURVE ( 'NONE', #22163, #37012, #46709, .T. ) ;
#34914 = VECTOR ( 'NONE', #41230, 999.9999999999998863 ) ;
#34915 = VECTOR ( 'NONE', #29105, 999.9999999999998863 ) ;
#34916 = DIRECTION ( 'NONE',  ( 0.000000000000000000, -0.000000000000000000, -1.000000000000000000 ) ) ;
#34917 = VERTEX_POINT ( 'NONE', #13199 ) ;
#34918 = EDGE_CURVE ( 'NONE', #6114, #44308, #25994, .T. ) ;
#34919 = DIRECTION ( 'NONE',  ( 0.6427681459581294776, -0.7660444431189769032, 0.005002170337467562802 ) ) ;
#34920 = DIRECTION ( 'NONE',  ( 0.9999697198139515519, 0.000000000000000000, 0.007781995580013368816 ) ) ;
#34921 = EDGE_LOOP ( 'NONE', ( #42741, #14593, #11049, #31616 ) ) ;
#34922 = FACE_OUTER_BOUND ( 'NONE', #6265, .T. ) ;
#34923 = ORIENTED_EDGE ( 'NONE', *, *, #2743, .F. ) ;
#34924 = ADVANCED_FACE ( 'NONE', ( #52089 ), #8950, .F. ) ;
#34925 = DIRECTION ( 'NONE',  ( 0.9999697198139515519, 0.000000000000000000, 0.007781995580013368816 ) ) ;
#34926 = EDGE_CURVE ( 'NONE', #24834, #11836, #20860, .T. ) ;
#34927 = VECTOR ( 'NONE', #42277, 1000.000000000000227 ) ;
#34928 = CARTESIAN_POINT ( 'NONE',  ( -30.79411802867772607, 0.000000000000000000, 8.643412946479525516 ) ) ;
#34929 = EDGE_LOOP ( 'NONE', ( #6584, #36347, #36351, #36165 ) ) ;
#34930 = LINE ( 'NONE', #26379, #37645 ) ;
#34931 = DIRECTION ( 'NONE',  ( 0.007781995580012663651, 0.000000000000000000, -0.9999697198139515519 ) ) ;
#34933 = VECTOR ( 'NONE', #5567, 1000.000000000000227 ) ;
#34932 = PLANE ( 'NONE',  #23026 ) ;
#34934 = VERTEX_POINT ( 'NONE', #39030 ) ;
#34935 = LINE ( 'NONE', #254, #10167 ) ;
#34936 = ORIENTED_EDGE ( 'NONE', *, *, #35615, .F. ) ;
#34937 = VECTOR ( 'NONE', #49676, 1000.000000000000114 ) ;
#34938 = PLANE ( 'NONE',  #7450 ) ;
#34939 = CARTESIAN_POINT ( 'NONE',  ( -17.36532418587302473, -0.1191753592594177458, 13.67570816655714516 ) ) ;
#34940 = LINE ( 'NONE', #43999, #5020 ) ;
#34941 = CARTESIAN_POINT ( 'NONE',  ( -30.79411802867772607, 0.000000000000000000, 8.643412946479525516 ) ) ;
#34942 = AXIS2_PLACEMENT_3D ( 'NONE', #55730, #51488, #52024 ) ;
#34943 = PLANE ( 'NONE',  #24106 ) ;
#34944 = DIRECTION ( 'NONE',  ( 0.000000000000000000, 0.000000000000000000, -1.000000000000000000 ) ) ;
#34945 = CARTESIAN_POINT ( 'NONE',  ( -21.99342909152279191, 19.77817276104758193, -4.416855321001344592 ) ) ;
#34947 = VECTOR ( 'NONE', #46498, 999.9999999999998863 ) ;
#34946 = CARTESIAN_POINT ( 'NONE',  ( -19.35744109503886889, -4.241740624735664156, 4.265074886081953842 ) ) ;
#34948 = VECTOR ( 'NONE', #46350, 999.9999999999998863 ) ;
#34949 = FILL_AREA_STYLE ('',( #56227 ) ) ;
#34951 = PLANE ( 'NONE',  #18721 ) ;
#34950 = VECTOR ( 'NONE', #18825, 999.9999999999998863 ) ;
#34952 = ORIENTED_EDGE ( 'NONE', *, *, #7814, .T. ) ;
#34953 = CARTESIAN_POINT ( 'NONE',  ( -15.87975247367846166, 0.000000000000000000, 2.850166870931599927 ) ) ;
#34954 = LINE ( 'NONE', #47994, #975 ) ;
#34956 = AXIS2_PLACEMENT_3D ( 'NONE', #21237, #7616, #194 ) ;
#34955 = LINE ( 'NONE', #21866, #14164 ) ;
#34957 = PLANE ( 'NONE',  #1363 ) ;
#34958 = CARTESIAN_POINT ( 'NONE',  ( -13.13452722693079444, -0.1191753592594185784, 7.403518714363871212 ) ) ;
#34959 = PLANE ( 'NONE',  #46497 ) ;
#34960 = ORIENTED_EDGE ( 'NONE', *, *, #6264, .F. ) ;
#34961 = VECTOR ( 'NONE', #49184, 1000.000000000000227 ) ;
#34962 = VECTOR ( 'NONE', #39557, 1000.000000000000227 ) ;
#34963 = ORIENTED_EDGE ( 'NONE', *, *, #30144, .T. ) ;
#34964 = DIRECTION ( 'NONE',  ( 0.6427681459581294776, -0.7660444431189769032, 0.005002170337467562802 ) ) ;
#34965 = FACE_OUTER_BOUND ( 'NONE', #1720, .T. ) ;
#34966 = VERTEX_POINT ( 'NONE', #3547 ) ;
#34967 = LINE ( 'NONE', #39198, #2116 ) ;
#34968 = EDGE_CURVE ( 'NONE', #50596, #38457, #8365, .T. ) ;
#34969 = ORIENTED_EDGE ( 'NONE', *, *, #55381, .F. ) ;
#34970 = CARTESIAN_POINT ( 'NONE',  ( -14.20280369269832832, 0.000000000000000000, 12.40765738797303719 ) ) ;
#34971 = ORIENTED_EDGE ( 'NONE', *, *, #40668, .T. ) ;
#34972 = FACE_OUTER_BOUND ( 'NONE', #8732, .T. ) ;
#34973 = ADVANCED_FACE ( 'NONE', ( #17436 ), #34769, .F. ) ;
#34974 = EDGE_CURVE ( 'NONE', #51694, #23998, #55494, .T. ) ;
#34975 = AXIS2_PLACEMENT_3D ( 'NONE', #36773, #49558, #1571 ) ;
#34976 = ORIENTED_EDGE ( 'NONE', *, *, #12744, .F. ) ;
#34977 = ORIENTED_EDGE ( 'NONE', *, *, #15719, .F. ) ;
#34978 = VERTEX_POINT ( 'NONE', #43563 ) ;
#34979 = VECTOR ( 'NONE', #30951, 999.9999999999998863 ) ;
#34980 = LINE ( 'NONE', #33832, #24805 ) ;
#34981 = PLANE ( 'NONE',  #20512 ) ;
#34982 = VECTOR ( 'NONE', #45075, 1000.000000000000227 ) ;
#34983 = CARTESIAN_POINT ( 'NONE',  ( -14.00280974873554030, 0.000000000000000000, 12.40921378708904044 ) ) ;
#34984 = PLANE ( 'NONE',  #39293 ) ;
#34985 = ORIENTED_EDGE ( 'NONE', *, *, #34456, .T. ) ;
#34986 = VECTOR ( 'NONE', #7136, 1000.000000000000227 ) ;
#34987 = VERTEX_POINT ( 'NONE', #21137 ) ;
#34988 = EDGE_LOOP ( 'NONE', ( #54592, #52447, #29210, #12444 ) ) ;
#34989 = VECTOR ( 'NONE', #45186, 999.9999999999998863 ) ;
#34990 = AXIS2_PLACEMENT_3D ( 'NONE', #18561, #44133, #36726 ) ;
#34991 = CARTESIAN_POINT ( 'NONE',  ( -11.18042193777012017, 0.9340140483890051470, 0.9949873626040346419 ) ) ;
#34992 = ORIENTED_EDGE ( 'NONE', *, *, #11075, .T. ) ;
#34993 = PLANE ( 'NONE',  #27542 ) ;
#34994 = ORIENTED_EDGE ( 'NONE', *, *, #53359, .F. ) ;
#34995 = DIRECTION ( 'NONE',  ( -0.005961354470445682716, -0.6427876096865404731, 0.7660212471507180654 ) ) ;
#34996 = CARTESIAN_POINT ( 'NONE',  ( -16.46476824831552932, 0.000000000000000000, 4.522948478349086088 ) ) ;
#34997 = AXIS2_PLACEMENT_3D ( 'NONE', #12080, #3303, #8389 ) ;
#34998 = ORIENTED_EDGE ( 'NONE', *, *, #8027, .T. ) ;
#34999 = VECTOR ( 'NONE', #38898, 1000.000000000000227 ) ;
#35000 = DIRECTION ( 'NONE',  ( 0.007781995580012663651, 0.000000000000000000, -0.9999697198139515519 ) ) ;
#35001 = VECTOR ( 'NONE', #5353, 999.9999999999998863 ) ;
#35002 = VERTEX_POINT ( 'NONE', #21980 ) ;
#35003 = EDGE_CURVE ( 'NONE', #9247, #49612, #25408, .T. ) ;
#35004 = VECTOR ( 'NONE', #35379, 999.9999999999998863 ) ;
#35005 = CARTESIAN_POINT ( 'NONE',  ( -27.99845268667336384, -0.1191753592594197858, 7.657176279295684118 ) ) ;
#35006 = VECTOR ( 'NONE', #4492, 999.9999999999998863 ) ;
#35008 = EDGE_CURVE ( 'NONE', #25831, #19882, #29392, .T. ) ;
#35007 = ORIENTED_EDGE ( 'NONE', *, *, #9900, .F. ) ;
#35009 = LINE ( 'NONE', #52575, #2374 ) ;
#35010 = DIRECTION ( 'NONE',  ( 0.9999697198139515519, 0.000000000000000000, 0.007781995580013368816 ) ) ;
#35011 = DIRECTION ( 'NONE',  ( 0.007781995580012662783, 0.000000000000000000, -0.9999697198139514409 ) ) ;
#35012 = ORIENTED_EDGE ( 'NONE', *, *, #25394, .F. ) ;
#35013 = LINE ( 'NONE', #13960, #30198 ) ;
#35014 = DIRECTION ( 'NONE',  ( 0.000000000000000000, -0.000000000000000000, -1.000000000000000000 ) ) ;
#35015 = EDGE_CURVE ( 'NONE', #24159, #41243, #47277, .T. ) ;
#35016 = CARTESIAN_POINT ( 'NONE',  ( -14.94760462649100496, 0.000000000000000000, 2.488088991209854051 ) ) ;
#35017 = CARTESIAN_POINT ( 'NONE',  ( 2.072287782118878319, 0.000000000000000000, -2.950529333540147015 ) ) ;
#35018 = CARTESIAN_POINT ( 'NONE',  ( -13.74590162550491890, -1.975113310420657520, 5.262804166939828221 ) ) ;
#35019 = LINE ( 'NONE', #52329, #18858 ) ;
#35020 = VECTOR ( 'NONE', #36696, 999.9999999999998863 ) ;
#35021 = CARTESIAN_POINT ( 'NONE',  ( -50.99228148001754590, 2.341865487272625668, 5.000000000000000000 ) ) ;
#35022 = ORIENTED_EDGE ( 'NONE', *, *, #34968, .T. ) ;
#35023 = CARTESIAN_POINT ( 'NONE',  ( -25.20278734466900517, 0.000000000000000000, 6.670939612111840944 ) ) ;
#35024 = PLANE ( 'NONE',  #47684 ) ;
#35025 = DIRECTION ( 'NONE',  ( 0.007781995580012662783, 0.000000000000000000, -0.9999697198139514409 ) ) ;
#35026 = ORIENTED_EDGE ( 'NONE', *, *, #54155, .F. ) ;
#35027 = CARTESIAN_POINT ( 'NONE',  ( -22.40556560354864146, -0.1191753592594197858, 5.484709000965211523 ) ) ;
#35028 = DIRECTION ( 'NONE',  ( -0.7660212471507179544, -0.6427876096865405842, -0.005961354470445141482 ) ) ;
#35029 = AXIS2_PLACEMENT_3D ( 'NONE', #56099, #17452, #34788 ) ;
#35030 = EDGE_LOOP ( 'NONE', ( #1859, #19376, #41724, #42634 ) ) ;
#35031 = PLANE ( 'NONE',  #14406 ) ;
#35032 = CARTESIAN_POINT ( 'NONE',  ( -20.25347771009236908, -0.1191753592594193140, 5.501457046573825060 ) ) ;
#35033 = VECTOR ( 'NONE', #11925, 1000.000000000000114 ) ;
#35034 = DIRECTION ( 'NONE',  ( 0.9999697198139515519, 0.000000000000000000, 0.007781995580013368816 ) ) ;
#35035 = CARTESIAN_POINT ( 'NONE',  ( -16.30304311551386931, -1.165603555308157846, 3.176787860902857918 ) ) ;
#35036 = VERTEX_POINT ( 'NONE', #38771 ) ;
#35037 = VECTOR ( 'NONE', #24105, 999.9999999999998863 ) ;
#35038 = VECTOR ( 'NONE', #32727, 999.9999999999998863 ) ;
#35039 = EDGE_LOOP ( 'NONE', ( #17662, #37909, #4002, #37852 ) ) ;
#35040 = LINE ( 'NONE', #5471, #44831 ) ;
#35041 = LINE ( 'NONE', #39837, #15944 ) ;
#35042 = CARTESIAN_POINT ( 'NONE',  ( -15.13495153988577968, 0.000000000000000000, 12.76973526769478084 ) ) ;
#35043 = EDGE_CURVE ( 'NONE', #1119, #29692, #400, .T. ) ;
#35044 = B_SPLINE_CURVE_WITH_KNOTS ( 'NONE', 3,
 ( #26021, #12661, #4149, #43335 ),
 .UNSPECIFIED., .F., .F.,
 ( 4, 4 ),
 ( 0.6614527403836476527, 0.6877732163401213406 ),
 .UNSPECIFIED. ) ;
#35045 = AXIS2_PLACEMENT_3D ( 'NONE', #19472, #36815, #9860 ) ;
#35046 = DIRECTION ( 'NONE',  ( -0.5449076811759708816, 0.6444004775717707689, 0.5364919789714475140 ) ) ;
#35048 = CARTESIAN_POINT ( 'NONE',  ( 2.072287782118878319, 0.000000000000000000, -2.950529333540147015 ) ) ;
#35047 = AXIS2_PLACEMENT_3D ( 'NONE', #24922, #20921, #21211 ) ;
#35049 = CARTESIAN_POINT ( 'NONE',  ( -10.63551161020563995, 0.2864062442990031321, 0.8039877656949352414 ) ) ;
#35050 = ORIENTED_EDGE ( 'NONE', *, *, #32641, .T. ) ;
#35051 = DIRECTION ( 'NONE',  ( 0.7660212471507180654, -0.6427876096865404731, 0.005961354470445141482 ) ) ;
#35052 = EDGE_CURVE ( 'NONE', #2799, #55479, #29702, .T. ) ;
#35053 = AXIS2_PLACEMENT_3D ( 'NONE', #27632, #10860, #11123 ) ;
#35054 = VECTOR ( 'NONE', #25950, 999.9999999999998863 ) ;
#35055 = CARTESIAN_POINT ( 'NONE',  ( -13.90497357559251590, 4.172053068839010947, 1.949985347149532533 ) ) ;
#35056 = ORIENTED_EDGE ( 'NONE', *, *, #5023, .F. ) ;
#35057 = CARTESIAN_POINT ( 'NONE',  ( -56.75000000000000711, -9.000000000000000000, 2.449489742783185875 ) ) ;
#35058 = DIRECTION ( 'NONE',  ( 0.9321478471874540261, 0.000000000000000000, -0.3620778797217457101 ) ) ;
#35059 = LINE ( 'NONE', #52363, #29381 ) ;
#35060 = ORIENTED_EDGE ( 'NONE', *, *, #13979, .T. ) ;
#35061 = PRODUCT_DEFINITION ( 'UNKNOWN', '', #19916, #29710 ) ;
#35062 = DIRECTION ( 'NONE',  ( 0.000000000000000000, 1.000000000000000000, 0.000000000000000000 ) ) ;
#35063 = ORIENTED_EDGE ( 'NONE', *, *, #9501, .T. ) ;
#35064 = AXIS2_PLACEMENT_3D ( 'NONE', #45291, #10922, #23444 ) ;
#35065 = EDGE_CURVE ( 'NONE', #18119, #14885, #17172, .T. ) ;
#35066 = VERTEX_POINT ( 'NONE', #47255 ) ;
#35067 = ORIENTED_EDGE ( 'NONE', *, *, #36145, .T. ) ;
#35068 = ORIENTED_EDGE ( 'NONE', *, *, #48998, .F. ) ;
#35069 = FACE_OUTER_BOUND ( 'NONE', #47163, .T. ) ;
#35070 = VECTOR ( 'NONE', #14286, 999.9999999999998863 ) ;
#35071 = ORIENTED_EDGE ( 'NONE', *, *, #36270, .F. ) ;
#35072 = LINE ( 'NONE', #39861, #27688 ) ;
#35073 = ORIENTED_EDGE ( 'NONE', *, *, #7955, .F. ) ;
#35074 = LINE ( 'NONE', #35332, #48583 ) ;
#35075 = AXIS2_PLACEMENT_3D ( 'NONE', #38739, #42976, #56050 ) ;
#35076 = ORIENTED_EDGE ( 'NONE', *, *, #27727, .T. ) ;
#35077 = CARTESIAN_POINT ( 'NONE',  ( -14.10280672071693431, -0.1191753592594197858, 12.40843558753103792 ) ) ;
#35078 = ORIENTED_EDGE ( 'NONE', *, *, #27574, .T. ) ;
#35079 = VECTOR ( 'NONE', #41626, 1000.000000000000227 ) ;
#35080 = CARTESIAN_POINT ( 'NONE',  ( -9.993945985744899119, -0.4219234865752066743, 1.264602792408272114 ) ) ;
#35081 = DIRECTION ( 'NONE',  ( 0.007781995580012662783, 0.000000000000000000, -0.9999697198139514409 ) ) ;
#35082 = LINE ( 'NONE', #42718, #43085 ) ;
#35083 = DIRECTION ( 'NONE',  ( -0.9999697198139514409, -0.000000000000000000, -0.007781995580013368816 ) ) ;
#35084 = CARTESIAN_POINT ( 'NONE',  ( -31.72782227498118601, 0.000000000000000000, 9.205484770164058972 ) ) ;
#35085 = VERTEX_POINT ( 'NONE', #30237 ) ;
#35086 = ORIENTED_EDGE ( 'NONE', *, *, #54254, .T. ) ;
#35087 = VECTOR ( 'NONE', #35083, 1000.000000000000227 ) ;
#35088 = CARTESIAN_POINT ( 'NONE',  ( -13.07066190154808361, 0.000000000000000000, 12.04713590736729678 ) ) ;
#35089 = ADVANCED_FACE ( 'NONE', ( #48687 ), #53487, .F. ) ;
#35090 = FACE_OUTER_BOUND ( 'NONE', #11553, .T. ) ;
#35091 = VECTOR ( 'NONE', #17570, 999.9999999999998863 ) ;
#35092 = PLANE ( 'NONE',  #35169 ) ;
#35093 = AXIS2_PLACEMENT_3D ( 'NONE', #13629, #35790, #27538 ) ;
#35094 = LINE ( 'NONE', #52395, #50279 ) ;
#35095 = PLANE ( 'NONE',  #44874 ) ;
#35096 = CARTESIAN_POINT ( 'NONE',  ( -8.397167190602280229, -10.18620209871003190, 6.480118481491868643 ) ) ;
#35097 = EDGE_LOOP ( 'NONE', ( #15588, #50632, #44727, #10226 ) ) ;
#35098 = CARTESIAN_POINT ( 'NONE',  ( -11.71762410836527479, -0.1191753592594190225, 4.459888823605786534 ) ) ;
#35099 = CARTESIAN_POINT ( 'NONE',  ( -19.60990026154428278, 0.000000000000000000, 4.498472333781370125 ) ) ;
#35100 = ORIENTED_EDGE ( 'NONE', *, *, #2556, .F. ) ;
#35101 = EDGE_CURVE ( 'NONE', #36934, #20261, #35608, .T. ) ;
#35102 = CARTESIAN_POINT ( 'NONE',  ( -16.04002523658126833, -0.8417996532631565332, 4.293958898594414819 ) ) ;
#35103 = FACE_OUTER_BOUND ( 'NONE', #25362, .T. ) ;
#35104 = LINE ( 'NONE', #52658, #20461 ) ;
#35105 = ADVANCED_FACE ( 'NONE', ( #1535 ), #5505, .F. ) ;
#35106 = EDGE_CURVE ( 'NONE', #12574, #21773, #14587, .T. ) ;
#35107 = FACE_OUTER_BOUND ( 'NONE', #30433, .T. ) ;
#35108 = AXIS2_PLACEMENT_3D ( 'NONE', #32672, #44916, #49456 ) ;
#35109 = CARTESIAN_POINT ( 'NONE',  ( -16.79925329029790149, 0.000000000000000000, 13.49544742625427496 ) ) ;
#35110 = ORIENTED_EDGE ( 'NONE', *, *, #37841, .F. ) ;
#35111 = ORIENTED_EDGE ( 'NONE', *, *, #1643, .T. ) ;
#35112 = CARTESIAN_POINT ( 'NONE',  ( -30.79489622823572859, -0.1191753592594197858, 8.743409918460921304 ) ) ;
#35113 = LINE ( 'NONE', #39344, #7717 ) ;
#35114 = CARTESIAN_POINT ( 'NONE',  ( -16.08797912965199473, -0.3560938001956556742, 3.119077304627356106 ) ) ;
#35115 = ADVANCED_FACE ( 'NONE', ( #30799 ), #35337, .F. ) ;
#35116 = CARTESIAN_POINT ( 'NONE',  ( -27.06708303904391144, 0.000000000000000000, 7.395095371555332697 ) ) ;
#35117 = EDGE_CURVE ( 'NONE', #31029, #41476, #40143, .T. ) ;
#35118 = VECTOR ( 'NONE', #41018, 1000.000000000000000 ) ;
#35119 = DIRECTION ( 'NONE',  ( -0.5449076811759708816, 0.6444004775717707689, 0.5364919789714475140 ) ) ;
#35120 = DIRECTION ( 'NONE',  ( -0.5449076811759708816, 0.6444004775717707689, 0.5364919789714475140 ) ) ;
#35121 = CARTESIAN_POINT ( 'NONE',  ( -8.829027555779365599, 0.000000000000000000, 4.382365521790453577 ) ) ;
#35122 = EDGE_CURVE ( 'NONE', #48589, #30223, #35913, .T. ) ;
#35123 = ORIENTED_EDGE ( 'NONE', *, *, #41772, .T. ) ;
#35125 = AXIS2_PLACEMENT_3D ( 'NONE', #39336, #30817, #43581 ) ;
#35124 = DIRECTION ( 'NONE',  ( 0.007781995580012663651, 0.000000000000000000, -0.9999697198139515519 ) ) ;
#35126 = CARTESIAN_POINT ( 'NONE',  ( -16.81345671998191449, 0.000000000000000000, 3.412238694616132495 ) ) ;
#35127 = ORIENTED_EDGE ( 'NONE', *, *, #45290, .T. ) ;
#35128 = DIRECTION ( 'NONE',  ( 0.000000000000000000, -0.000000000000000000, -1.000000000000000000 ) ) ;
#35129 = ORIENTED_EDGE ( 'NONE', *, *, #39249, .T. ) ;
#35130 = CARTESIAN_POINT ( 'NONE',  ( -15.60102546347950536, 0.000000000000000000, 12.95077420755565356 ) ) ;
#35131 = CARTESIAN_POINT ( 'NONE',  ( -19.01105676419016888, -2.137015261443157232, 7.573677912176790095 ) ) ;
#35132 = EDGE_CURVE ( 'NONE', #52593, #19873, #27098, .T. ) ;
#35133 = ORIENTED_EDGE ( 'NONE', *, *, #45254, .T. ) ;
#35134 = VECTOR ( 'NONE', #2506, 1000.000000000000227 ) ;
#35135 = ORIENTED_EDGE ( 'NONE', *, *, #8948, .T. ) ;
#35136 = EDGE_CURVE ( 'NONE', #53425, #7643, #31902, .T. ) ;
#35137 = ORIENTED_EDGE ( 'NONE', *, *, #31713, .F. ) ;
#35138 = VECTOR ( 'NONE', #25379, 1000.000000000000227 ) ;
#35139 = ORIENTED_EDGE ( 'NONE', *, *, #52405, .F. ) ;
#35140 = ORIENTED_EDGE ( 'NONE', *, *, #34808, .T. ) ;
#35141 = ORIENTED_EDGE ( 'NONE', *, *, #6062, .F. ) ;
#35142 = DIRECTION ( 'NONE',  ( -0.5364919789714478471, 0.6444004775717705469, -0.5449076811759709926 ) ) ;
#35143 = CARTESIAN_POINT ( 'NONE',  ( 2.072287782118878319, 0.000000000000000000, -2.950529333540147015 ) ) ;
#35144 = DIRECTION ( 'NONE',  ( 0.007781995580012663651, 0.000000000000000000, -0.9999697198139515519 ) ) ;
#35145 = ORIENTED_EDGE ( 'NONE', *, *, #26749, .T. ) ;
#35146 = CARTESIAN_POINT ( 'NONE',  ( -10.86745071256952144, 0.000000000000000000, 1.781177552798060670 ) ) ;
#35147 = EDGE_LOOP ( 'NONE', ( #24061, #27868, #44600, #31699 ) ) ;
#35148 = VERTEX_POINT ( 'NONE', #18275 ) ;
#35149 = FACE_OUTER_BOUND ( 'NONE', #26871, .T. ) ;
#35150 = FACE_OUTER_BOUND ( 'NONE', #55763, .T. ) ;
#35151 = CARTESIAN_POINT ( 'NONE',  ( -67.86783029729696182, -11.27546072583064785, -7.472022508502797145 ) ) ;
#35152 = VERTEX_POINT ( 'NONE', #22560 ) ;
#35153 = DIRECTION ( 'NONE',  ( -0.005961354470445682716, -0.6427876096865404731, 0.7660212471507180654 ) ) ;
#35154 = ORIENTED_EDGE ( 'NONE', *, *, #10998, .F. ) ;
#35155 = DIRECTION ( 'NONE',  ( 0.005002170337468016433, -0.7660444431189770143, -0.6427681459581293666 ) ) ;
#35156 = EDGE_CURVE ( 'NONE', #678, #34349, #31060, .T. ) ;
#35157 = CARTESIAN_POINT ( 'NONE',  ( -18.92936932203669542, 0.000000000000000000, 4.134436313103331706 ) ) ;
#35158 = DIRECTION ( 'NONE',  ( 0.9999697198139515519, 0.000000000000000000, 0.007781995580013368816 ) ) ;
#35159 = VECTOR ( 'NONE', #25721, 1000.000000000000227 ) ;
#35160 = FACE_OUTER_BOUND ( 'NONE', #9410, .T. ) ;
#35161 = LINE ( 'NONE', #13821, #41349 ) ;
#35162 = CARTESIAN_POINT ( 'NONE',  ( 5.520171279030146039, -1.061450403529338837, -2.502362106692468835 ) ) ;
#35163 = PLANE ( 'NONE',  #24831 ) ;
#35164 = DIRECTION ( 'NONE',  ( 0.5449076811759707706, 0.6444004775717708799, -0.5364919789714476250 ) ) ;
#35165 = ORIENTED_EDGE ( 'NONE', *, *, #22632, .F. ) ;
#35166 = CARTESIAN_POINT ( 'NONE',  ( -18.32175943656386963, 0.000000000000000000, 4.308490887314260220 ) ) ;
#35167 = EDGE_CURVE ( 'NONE', #52074, #37125, #44144, .T. ) ;
#35168 = EDGE_CURVE ( 'NONE', #48125, #32400, #5795, .T. ) ;
#35169 = AXIS2_PLACEMENT_3D ( 'NONE', #35622, #22836, #1246 ) ;
#35170 = LINE ( 'NONE', #18673, #52846 ) ;
#35171 = PLANE ( 'NONE',  #31426 ) ;
#35172 = FACE_OUTER_BOUND ( 'NONE', #16079, .T. ) ;
#35173 = FACE_OUTER_BOUND ( 'NONE', #50161, .T. ) ;
#35174 = PLANE ( 'NONE',  #7743 ) ;
#35175 = ADVANCED_FACE ( 'NONE', ( #10332 ), #1232, .F. ) ;
#35176 = LINE ( 'NONE', #22389, #42242 ) ;
#35177 = CARTESIAN_POINT ( 'NONE',  ( -1.246832498358330099E-15, 2.000000000000000000, 0.000000000000000000 ) ) ;
#35178 = B_SPLINE_CURVE_WITH_KNOTS ( 'NONE', 3,
 ( #22859, #52671, #9238, #26558 ),
 .UNSPECIFIED., .F., .F.,
 ( 4, 4 ),
 ( 0.3613060669372403777, 0.3753454237082048950 ),
 .UNSPECIFIED. ) ;
#35179 = ORIENTED_EDGE ( 'NONE', *, *, #3492, .F. ) ;
#35180 = CARTESIAN_POINT ( 'NONE',  ( -15.48150113315929488, -0.1191753592594177180, 9.231914369774386842 ) ) ;
#35181 = DIRECTION ( 'NONE',  ( 0.000000000000000000, -1.000000000000000000, 0.000000000000000000 ) ) ;
#35182 = CARTESIAN_POINT ( 'NONE',  ( -20.54126990917373519, -0.1191753592594197858, 4.760553241521720658 ) ) ;
#35183 = DIRECTION ( 'NONE',  ( -0.5364919789714478471, 0.6444004775717705469, -0.5449076811759709926 ) ) ;
#35184 = ADVANCED_FACE ( 'NONE', ( #23117 ), #27658, .F. ) ;
#35185 = DIRECTION ( 'NONE',  ( -0.8531650599175529814, -0.4028455766673920135, 0.3313982828793697877 ) ) ;
#35186 = PLANE ( 'NONE',  #25015 ) ;
#35187 = LINE ( 'NONE', #53042, #28356 ) ;
#35188 = EDGE_CURVE ( 'NONE', #4038, #5849, #32929, .T. ) ;
#35189 = DIRECTION ( 'NONE',  ( 0.005002170337468016433, -0.7660444431189770143, -0.6427681459581293666 ) ) ;
#35190 = LINE ( 'NONE', #47948, #10219 ) ;
#35191 = EDGE_CURVE ( 'NONE', #9106, #7467, #22283, .T. ) ;
#35192 = ORIENTED_EDGE ( 'NONE', *, *, #38990, .F. ) ;
#35193 = ORIENTED_EDGE ( 'NONE', *, *, #29418, .T. ) ;
#35194 = ORIENTED_EDGE ( 'NONE', *, *, #21574, .F. ) ;
#35195 = ORIENTED_EDGE ( 'NONE', *, *, #46398, .T. ) ;
#35196 = EDGE_LOOP ( 'NONE', ( #52145, #18176, #6747, #50695, #11211 ) ) ;
#35197 = FACE_OUTER_BOUND ( 'NONE', #25919, .T. ) ;
#35198 = CARTESIAN_POINT ( 'NONE',  ( 5.515120863165694942, -1.062156740595928683, 2.500028430129012325 ) ) ;
#35199 = VECTOR ( 'NONE', #3760, 1000.000000000000227 ) ;
#35200 = EDGE_LOOP ( 'NONE', ( #8295, #46397, #21523, #7945 ) ) ;
#35201 = ORIENTED_EDGE ( 'NONE', *, *, #33611, .F. ) ;
#35202 = DIRECTION ( 'NONE',  ( 0.000000000000000000, -1.000000000000000000, 0.000000000000000000 ) ) ;
#35203 = ORIENTED_EDGE ( 'NONE', *, *, #21811, .F. ) ;
#35204 = DIRECTION ( 'NONE',  ( -1.000000000000000000, 0.000000000000000000, 0.000000000000000000 ) ) ;
#35205 = DIRECTION ( 'NONE',  ( 0.007781995580012662783, 0.000000000000000000, -0.9999697198139514409 ) ) ;
#35206 = VERTEX_POINT ( 'NONE', #696 ) ;
#35207 = LINE ( 'NONE', #26372, #14809 ) ;
#35208 = EDGE_CURVE ( 'NONE', #47771, #15181, #48378, .T. ) ;
#35209 = VERTEX_POINT ( 'NONE', #53751 ) ;
#35210 = DIRECTION ( 'NONE',  ( -0.2426528472758541499, 0.7422098413412800966, -0.6246952433987894571 ) ) ;
#35211 = ADVANCED_FACE ( 'NONE', ( #36735 ), #49521, .F. ) ;
#35212 = CARTESIAN_POINT ( 'NONE',  ( -18.14763197414862717, 0.000000000000000000, 7.633834615750140884 ) ) ;
#35213 = DIRECTION ( 'NONE',  ( -1.000000000000000000, 0.000000000000000000, 0.000000000000000000 ) ) ;
#35214 = ORIENTED_EDGE ( 'NONE', *, *, #37437, .F. ) ;
#35215 = DIRECTION ( 'NONE',  ( 0.005002170337468016433, -0.7660444431189770143, -0.6427681459581293666 ) ) ;
#35216 = CARTESIAN_POINT ( 'NONE',  ( -20.25783497214359130, 5.629170628041515911, 4.371162778664604787 ) ) ;
#35217 = CARTESIAN_POINT ( 'NONE',  ( -16.06709938707323460, 0.000000000000000000, 13.13181314741652628 ) ) ;
#35218 = EDGE_CURVE ( 'NONE', #40640, #13570, #15992, .T. ) ;
#35219 = ORIENTED_EDGE ( 'NONE', *, *, #47951, .T. ) ;
#35220 = DIRECTION ( 'NONE',  ( 0.5364919789714477361, 0.6444004775717706579, 0.5449076811759711036 ) ) ;
#35221 = ORIENTED_EDGE ( 'NONE', *, *, #9191, .T. ) ;
#35222 = EDGE_CURVE ( 'NONE', #3481, #5914, #2893, .T. ) ;
#35223 = EDGE_CURVE ( 'NONE', #14453, #44396, #20222, .T. ) ;
#35224 = EDGE_CURVE ( 'NONE', #26864, #41020, #54317, .T. ) ;
#35225 = CARTESIAN_POINT ( 'NONE',  ( -9.382943410138716800, -0.1191753592594192307, 3.000729569414776421 ) ) ;
#35226 = CARTESIAN_POINT ( 'NONE',  ( -10.74029228357944987, 0.000000000000000000, 11.14194120806293320 ) ) ;
#35227 = LINE ( 'NONE', #5123, #53967 ) ;
#35228 = CARTESIAN_POINT ( 'NONE',  ( -14.00280974873554030, 0.000000000000000000, 12.40921378708904044 ) ) ;
#35229 = CARTESIAN_POINT ( 'NONE',  ( -11.37928600064400086, -0.8417996532631553119, 2.483569499985687656 ) ) ;
#35230 = ADVANCED_FACE ( 'NONE', ( #11149 ), #10879, .F. ) ;
#35231 = LINE ( 'NONE', #52525, #22212 ) ;
#35232 = PLANE ( 'NONE',  #10747 ) ;
#35233 = CARTESIAN_POINT ( 'NONE',  ( -14.93495759592298988, 0.000000000000000000, 12.77129166681078409 ) ) ;
#35234 = DIRECTION ( 'NONE',  ( 0.7660212471507180654, -0.6427876096865404731, 0.005961354470445141482 ) ) ;
#35235 = ORIENTED_EDGE ( 'NONE', *, *, #14700, .T. ) ;
#35236 = LINE ( 'NONE', #52533, #2137 ) ;
#35237 = CARTESIAN_POINT ( 'NONE',  ( -12.20812748675390758, -0.1191753592594177180, 7.780060241157652712 ) ) ;
#35238 = FACE_OUTER_BOUND ( 'NONE', #43895, .T. ) ;
#35239 = VECTOR ( 'NONE', #9939, 999.9999999999998863 ) ;
#35240 = FACE_OUTER_BOUND ( 'NONE', #30559, .T. ) ;
#35241 = ADVANCED_FACE ( 'NONE', ( #3197 ), #24234, .F. ) ;
#35242 = LINE ( 'NONE', #40619, #44158 ) ;
#35243 = CARTESIAN_POINT ( 'NONE',  ( -16.99924723426068951, 0.000000000000000000, 13.49389102713827171 ) ) ;
#35244 = ORIENTED_EDGE ( 'NONE', *, *, #37041, .T. ) ;
#35245 = EDGE_CURVE ( 'NONE', #51166, #22994, #54882, .T. ) ;
#35246 = ORIENTED_EDGE ( 'NONE', *, *, #17011, .F. ) ;
#35247 = EDGE_CURVE ( 'NONE', #54087, #19901, #32726, .T. ) ;
#35248 = DIRECTION ( 'NONE',  ( 0.005002170337468016433, -0.7660444431189770143, -0.6427681459581293666 ) ) ;
#35249 = DIRECTION ( 'NONE',  ( 0.005961354470445682716, -0.6427876096865404731, -0.7660212471507180654 ) ) ;
#35250 = EDGE_CURVE ( 'NONE', #12574, #3673, #14869, .T. ) ;
#35251 = ORIENTED_EDGE ( 'NONE', *, *, #13046, .F. ) ;
#35252 = CARTESIAN_POINT ( 'NONE',  ( -29.86352658060627618, 0.000000000000000000, 8.481329010720569883 ) ) ;
#35253 = EDGE_LOOP ( 'NONE', ( #11474, #43516, #14321, #14605 ) ) ;
#35254 = CARTESIAN_POINT ( 'NONE',  ( -30.79489622823572859, -0.1191753592594197858, 8.743409918460921304 ) ) ;
#35255 = EDGE_CURVE ( 'NONE', #54647, #29905, #33020, .T. ) ;
#35256 = VERTEX_POINT ( 'NONE', #19950 ) ;
#35257 = ORIENTED_EDGE ( 'NONE', *, *, #5710, .T. ) ;
#35258 = ORIENTED_EDGE ( 'NONE', *, *, #8901, .F. ) ;
#35259 = DIRECTION ( 'NONE',  ( 0.7660212471507180654, -0.6427876096865404731, 0.005961354470445141482 ) ) ;
#35260 = DIRECTION ( 'NONE',  ( -0.05705673239519651330, 0.9983709377222391712, 2.351258244848514932E-16 ) ) ;
#35261 = CARTESIAN_POINT ( 'NONE',  ( -16.95527162670416033, 0.000000000000000000, 7.843119895900956706 ) ) ;
#35262 = CARTESIAN_POINT ( 'NONE',  ( -12.08435988717225129, 0.000000000000000000, 4.726363842672150817 ) ) ;
#35263 = EDGE_LOOP ( 'NONE', ( #28872, #55149, #20823, #8561 ) ) ;
#35264 = VERTEX_POINT ( 'NONE', #29035 ) ;
#35265 = LINE ( 'NONE', #31566, #29997 ) ;
#35266 = ORIENTED_EDGE ( 'NONE', *, *, #42934, .F. ) ;
#35267 = DIRECTION ( 'NONE',  ( 0.8531650599175527594, 0.4028455766673922356, -0.3313982828793700652 ) ) ;
#35268 = VERTEX_POINT ( 'NONE', #32197 ) ;
#35269 = FACE_OUTER_BOUND ( 'NONE', #40897, .T. ) ;
#35270 = DIRECTION ( 'NONE',  ( 0.000000000000000000, -0.000000000000000000, -1.000000000000000000 ) ) ;
#35271 = AXIS2_PLACEMENT_3D ( 'NONE', #342, #43266, #8608 ) ;
#35272 = EDGE_LOOP ( 'NONE', ( #17326, #33821, #45134, #10932 ) ) ;
#35273 = DIRECTION ( 'NONE',  ( 0.007781995580012663651, -3.146120232559066537E-19, -0.9999697198139514409 ) ) ;
#35274 = ORIENTED_EDGE ( 'NONE', *, *, #47787, .T. ) ;
#35275 = DIRECTION ( 'NONE',  ( -0.9999697198139514409, -0.000000000000000000, -0.007781995580013368816 ) ) ;
#35276 = ORIENTED_EDGE ( 'NONE', *, *, #24588, .T. ) ;
#35277 = CARTESIAN_POINT ( 'NONE',  ( -15.55848688267561641, 0.000000000000000000, 7.484657927947219846 ) ) ;
#35278 = DIRECTION ( 'NONE',  ( 0.5449076811759707706, 0.6444004775717708799, -0.5364919789714476250 ) ) ;
#35279 = LINE ( 'NONE', #43769, #37318 ) ;
#35280 = ORIENTED_EDGE ( 'NONE', *, *, #22612, .T. ) ;
#35281 = EDGE_CURVE ( 'NONE', #11834, #51473, #28776, .T. ) ;
#35282 = ADVANCED_FACE ( 'NONE', ( #27947 ), #7186, .F. ) ;
#35283 = DIRECTION ( 'NONE',  ( 0.000000000000000000, -1.000000000000000000, 0.000000000000000000 ) ) ;
#35284 = FACE_OUTER_BOUND ( 'NONE', #20064, .T. ) ;
#35285 = CARTESIAN_POINT ( 'NONE',  ( -69.33582967021771992, 1.350899166405607588, 7.487487041937091803 ) ) ;
#35286 = DIRECTION ( 'NONE',  ( 0.000000000000000000, 0.000000000000000000, -1.000000000000000000 ) ) ;
#35287 = EDGE_CURVE ( 'NONE', #1004, #50871, #6351, .T. ) ;
#35288 = DIRECTION ( 'NONE',  ( 0.007781995580012663651, -3.146120232559066537E-19, -0.9999697198139514409 ) ) ;
#35289 = DIRECTION ( 'NONE',  ( 0.005002170337468016433, -0.7660444431189770143, -0.6427681459581293666 ) ) ;
#35290 = DIRECTION ( 'NONE',  ( -0.7660212471507179544, -0.6427876096865405842, -0.005961354470445141482 ) ) ;
#35291 = EDGE_LOOP ( 'NONE', ( #1931, #56130, #13520, #50541 ) ) ;
#35292 = CARTESIAN_POINT ( 'NONE',  ( -19.22961988024793101, -0.1191753592594177458, 14.39986392600063603 ) ) ;
#35293 = DIRECTION ( 'NONE',  ( 0.9999697198139515519, 0.000000000000000000, 0.007781995580013368816 ) ) ;
#35294 = VERTEX_POINT ( 'NONE', #23652 ) ;
#35295 = DIRECTION ( 'NONE',  ( -0.9999697198139514409, -0.000000000000000000, -0.007781995580013368816 ) ) ;
#35296 = CARTESIAN_POINT ( 'NONE',  ( -16.06709938707323460, 0.000000000000000000, 13.13181314741652628 ) ) ;
#35297 = ORIENTED_EDGE ( 'NONE', *, *, #24412, .F. ) ;
#35298 = DIRECTION ( 'NONE',  ( 0.7660212471507180654, -0.6427876096865404731, 0.005961354470445141482 ) ) ;
#35299 = CARTESIAN_POINT ( 'NONE',  ( -17.73140113748535285, 0.000000000000000000, 13.85752530597602039 ) ) ;
#35300 = DIRECTION ( 'NONE',  ( -0.5449076811759708816, 0.6444004775717707689, 0.5364919789714475140 ) ) ;
#35301 = PLANE ( 'NONE',  #16596 ) ;
#35302 = ORIENTED_EDGE ( 'NONE', *, *, #50598, .F. ) ;
#35303 = ORIENTED_EDGE ( 'NONE', *, *, #45068, .F. ) ;
#35304 = LINE ( 'NONE', #31319, #24893 ) ;
#35305 = CARTESIAN_POINT ( 'NONE',  ( -24.83619032682412353, 18.20871928901600256, 4.561852666301203563 ) ) ;
#35306 = CARTESIAN_POINT ( 'NONE',  ( -19.58586870846074390, -5.536956232915663634, 13.37683675498699998 ) ) ;
#35307 = CARTESIAN_POINT ( 'NONE',  ( -11.88054826722768276, 25.79903810567671130, -3.000000000000000000 ) ) ;
#35308 = MECHANICAL_DESIGN_GEOMETRIC_PRESENTATION_REPRESENTATION (  '', ( #20778 ), #52518 ) ;
#35309 = LINE ( 'NONE', #31024, #32820 ) ;
#35310 = DIRECTION ( 'NONE',  ( -0.005002170337468016433, -0.7660444431189770143, 0.6427681459581293666 ) ) ;
#35311 = ORIENTED_EDGE ( 'NONE', *, *, #51155, .T. ) ;
#35312 = LINE ( 'NONE', #48925, #11122 ) ;
#35313 = EDGE_CURVE ( 'NONE', #33893, #39017, #41545, .T. ) ;
#35314 = CARTESIAN_POINT ( 'NONE',  ( -10.64080840018947605, 0.2864062442990034651, 1.484613903501102117 ) ) ;
#35315 = ORIENTED_EDGE ( 'NONE', *, *, #1723, .F. ) ;
#35316 = EDGE_CURVE ( 'NONE', #25539, #35767, #2060, .T. ) ;
#35317 = CARTESIAN_POINT ( 'NONE',  ( -21.47419595591918906, 0.000000000000000000, 5.222628093224860102 ) ) ;
#35318 = CARTESIAN_POINT ( 'NONE',  ( -15.86710544311044302, 0.000000000000000000, 13.13336954653252953 ) ) ;
#35319 = ADVANCED_FACE ( 'NONE', ( #45797 ), #37269, .F. ) ;
#35320 = CARTESIAN_POINT ( 'NONE',  ( -12.29165833726160884, 0.000000000000000000, 5.663420794034463412 ) ) ;
#35321 = ORIENTED_EDGE ( 'NONE', *, *, #39879, .F. ) ;
#35322 = DIRECTION ( 'NONE',  ( 0.007781995580012663651, -3.146120232559066537E-19, -0.9999697198139514409 ) ) ;
#35323 = EDGE_CURVE ( 'NONE', #32995, #31598, #18139, .T. ) ;
#35324 = EDGE_LOOP ( 'NONE', ( #28481, #16117, #39742, #53246 ) ) ;
#35325 = VERTEX_POINT ( 'NONE', #50880 ) ;
#35326 = ORIENTED_EDGE ( 'NONE', *, *, #22725, .T. ) ;
#35327 = EDGE_LOOP ( 'NONE', ( #15788, #20588, #51847, #47427 ) ) ;
#35328 = CARTESIAN_POINT ( 'NONE',  ( -27.99767448711536133, 0.000000000000000000, 7.557179307314289218 ) ) ;
#35329 = EDGE_LOOP ( 'NONE', ( #12526, #39684, #16364, #53964 ) ) ;
#35330 = DIRECTION ( 'NONE',  ( -0.5364919789714478471, 0.6444004775717705469, -0.5449076811759709926 ) ) ;
#35331 = ORIENTED_EDGE ( 'NONE', *, *, #32404, .F. ) ;
#35332 = CARTESIAN_POINT ( 'NONE',  ( -16.66588516698283584, -3.756034771668160577, 9.319820460963413211 ) ) ;
#35333 = EDGE_LOOP ( 'NONE', ( #22888, #48363, #21056, #6439 ) ) ;
#35334 = DIRECTION ( 'NONE',  ( -0.005961354470445682716, -0.6427876096865404731, 0.7660212471507180654 ) ) ;
#35335 = ORIENTED_EDGE ( 'NONE', *, *, #44801, .F. ) ;
#35336 = DIRECTION ( 'NONE',  ( -0.7660212471507179544, -0.6427876096865405842, -0.005961354470445141482 ) ) ;
#35337 = PLANE ( 'NONE',  #37465 ) ;
#35338 = DIRECTION ( 'NONE',  ( 0.2113248654051873565, 0.7886751345948123104, 0.5773502691896265082 ) ) ;
#35339 = CARTESIAN_POINT ( 'NONE',  ( -18.70729593551854464, -0.1191753592594171213, 6.990818069889991548 ) ) ;
#35340 = CARTESIAN_POINT ( 'NONE',  ( -57.29829478218162109, -10.27834239552269757, 4.211285351864063224E-15 ) ) ;
#35341 = LINE ( 'NONE', #17748, #12942 ) ;
#35342 = ORIENTED_EDGE ( 'NONE', *, *, #10070, .T. ) ;
#35343 = ADVANCED_FACE ( 'NONE', ( #20796 ), #55718, .T. ) ;
#35344 = ORIENTED_EDGE ( 'NONE', *, *, #15787, .T. ) ;
#35345 = DIRECTION ( 'NONE',  ( 0.007781995580012663651, 0.000000000000000000, -0.9999697198139515519 ) ) ;
#35346 = DIRECTION ( 'NONE',  ( 0.000000000000000000, -1.000000000000000000, 0.000000000000000000 ) ) ;
#35347 = EDGE_CURVE ( 'NONE', #45853, #32666, #55165, .T. ) ;
#35348 = EDGE_CURVE ( 'NONE', #29854, #40359, #55426, .T. ) ;
#35349 = DIRECTION ( 'NONE',  ( 0.5364919789714477361, 0.6444004775717706579, 0.5449076811759711036 ) ) ;
#35350 = FACE_OUTER_BOUND ( 'NONE', #45523, .T. ) ;
#35351 = CARTESIAN_POINT ( 'NONE',  ( -18.52282235942901778, 1.905425754524006532, 3.816031916019901438 ) ) ;
#35352 = DIRECTION ( 'NONE',  ( 0.9999697198139515519, 0.000000000000000000, 0.007781995580013368816 ) ) ;
#35353 = ORIENTED_EDGE ( 'NONE', *, *, #46627, .F. ) ;
#35354 = CARTESIAN_POINT ( 'NONE',  ( -32.65841372305263235, 0.000000000000000000, 9.367568705923016381 ) ) ;
#35355 = DIRECTION ( 'NONE',  ( 0.000000000000000000, 1.000000000000000000, 0.000000000000000000 ) ) ;
#35356 = ORIENTED_EDGE ( 'NONE', *, *, #23281, .T. ) ;
#35357 = CARTESIAN_POINT ( 'NONE',  ( -9.775545670493231754, 0.000000000000000000, 6.590991917801018118 ) ) ;
#35358 = LINE ( 'NONE', #9518, #11513 ) ;
#35359 = DIRECTION ( 'NONE',  ( 1.000000000000000000, 0.000000000000000000, -8.673617379884027583E-16 ) ) ;
#35360 = DIRECTION ( 'NONE',  ( 0.7660212471507180654, -0.6427876096865404731, 0.005961354470445141482 ) ) ;
#35361 = ADVANCED_FACE ( 'NONE', ( #42649 ), #9339, .F. ) ;
#35362 = FACE_OUTER_BOUND ( 'NONE', #13747, .T. ) ;
#35363 = ORIENTED_EDGE ( 'NONE', *, *, #21527, .F. ) ;
#35364 = ORIENTED_EDGE ( 'NONE', *, *, #825, .T. ) ;
#35365 = DIRECTION ( 'NONE',  ( 0.005002170337468016433, -0.7660444431189770143, -0.6427681459581293666 ) ) ;
#35366 = CARTESIAN_POINT ( 'NONE',  ( -14.94838282604900748, -0.1191753592594197858, 2.588085963191248506 ) ) ;
#35367 = CARTESIAN_POINT ( 'NONE',  ( -10.40856192273900049, 0.000000000000000000, 2.523412871081599285 ) ) ;
#35368 = CARTESIAN_POINT ( 'NONE',  ( -12.33850799832341849, 0.000000000000000000, 11.68350162852954632 ) ) ;
#35369 = DIRECTION ( 'NONE',  ( -0.6427681459581293666, -0.7660444431189770143, -0.005002170337467561935 ) ) ;
#35370 = EDGE_LOOP ( 'NONE', ( #6246, #18076, #4719, #26700 ) ) ;
#35371 = CARTESIAN_POINT ( 'NONE',  ( -16.53317331066696383, 0.000000000000000000, 13.31285208727739899 ) ) ;
#35372 = LINE ( 'NONE', #4162, #22939 ) ;
#35373 = VECTOR ( 'NONE', #22873, 1000.000000000000227 ) ;
#35374 = LINE ( 'NONE', #22601, #46794 ) ;
#35375 = PLANE ( 'NONE',  #6095 ) ;
#35376 = ORIENTED_EDGE ( 'NONE', *, *, #47172, .F. ) ;
#35377 = DIRECTION ( 'NONE',  ( 0.6427681459581294776, -0.7660444431189769032, 0.005002170337467562802 ) ) ;
#35378 = ORIENTED_EDGE ( 'NONE', *, *, #45037, .F. ) ;
#35379 = DIRECTION ( 'NONE',  ( 0.9999697198139515519, 0.000000000000000000, 0.007781995580013368816 ) ) ;
#35380 = CARTESIAN_POINT ( 'NONE',  ( -15.83462604957504283, 0.000000000000000000, 8.959837228326271941 ) ) ;
#35381 = ORIENTED_EDGE ( 'NONE', *, *, #47741, .F. ) ;
#35382 = DIRECTION ( 'NONE',  ( -0.6427681459581293666, -0.7660444431189770143, -0.005002170337467561935 ) ) ;
#35383 = ADVANCED_FACE ( 'NONE', ( #13878 ), #30918, .F. ) ;
#35384 = ORIENTED_EDGE ( 'NONE', *, *, #8880, .F. ) ;
#35385 = ORIENTED_EDGE ( 'NONE', *, *, #54873, .F. ) ;
#35386 = EDGE_LOOP ( 'NONE', ( #50999, #22750, #54233, #23392 ) ) ;
#35387 = LINE ( 'NONE', #1002, #13056 ) ;
#35388 = VERTEX_POINT ( 'NONE', #51476 ) ;
#35389 = ORIENTED_EDGE ( 'NONE', *, *, #31094, .T. ) ;
#35390 = DIRECTION ( 'NONE',  ( 0.007781995580012663651, -3.146120232559066537E-19, -0.9999697198139514409 ) ) ;
#35391 = DIRECTION ( 'NONE',  ( 0.6246952433987893460, 0.7422098413412802076, -0.2426528472758539279 ) ) ;
#35392 = ORIENTED_EDGE ( 'NONE', *, *, #42686, .F. ) ;
#35393 = EDGE_CURVE ( 'NONE', #31757, #40214, #7751, .T. ) ;
#35394 = ORIENTED_EDGE ( 'NONE', *, *, #21166, .T. ) ;
#35395 = DIRECTION ( 'NONE',  ( 0.007781995580012663651, 0.000000000000000000, -0.9999697198139515519 ) ) ;
#35396 = ORIENTED_EDGE ( 'NONE', *, *, #36781, .F. ) ;
#35397 = EDGE_CURVE ( 'NONE', #19674, #32400, #12292, .T. ) ;
#35398 = ORIENTED_EDGE ( 'NONE', *, *, #56190, .F. ) ;
#35399 = EDGE_CURVE ( 'NONE', #38932, #56078, #3744, .T. ) ;
#35400 = LINE ( 'NONE', #1017, #51931 ) ;
#35401 = CARTESIAN_POINT ( 'NONE',  ( -19.56975256245720729, 0.9340140483890051470, 4.253688280099741981 ) ) ;
#35402 = CARTESIAN_POINT ( 'NONE',  ( -20.20936687189512071, 3.848249166794008413, 11.04695801043525094 ) ) ;
#35403 = EDGE_CURVE ( 'NONE', #52700, #41193, #51176, .T. ) ;
#35404 = ORIENTED_EDGE ( 'NONE', *, *, #17158, .T. ) ;
#35405 = DIRECTION ( 'NONE',  ( 0.6246952433987893460, 0.7422098413412802076, -0.2426528472758539279 ) ) ;
#35406 = VERTEX_POINT ( 'NONE', #43982 ) ;
#35407 = EDGE_CURVE ( 'NONE', #3706, #6183, #34423, .T. ) ;
#35408 = LINE ( 'NONE', #52710, #330 ) ;
#35409 = EDGE_CURVE ( 'NONE', #34792, #48505, #26663, .T. ) ;
#35410 = AXIS2_PLACEMENT_3D ( 'NONE', #52267, #586, #22712 ) ;
#35411 = CARTESIAN_POINT ( 'NONE',  ( -21.47419595591918906, 0.000000000000000000, 5.222628093224860102 ) ) ;
#35412 = DIRECTION ( 'NONE',  ( -0.005002170337468016433, -0.7660444431189770143, 0.6427681459581293666 ) ) ;
#35413 = LINE ( 'NONE', #22636, #21413 ) ;
#35414 = FACE_OUTER_BOUND ( 'NONE', #39368, .T. ) ;
#35415 = CARTESIAN_POINT ( 'NONE',  ( -11.87243407472968926, 0.000000000000000000, 11.50246268866867361 ) ) ;
#35416 = DIRECTION ( 'NONE',  ( 0.007781995580012663651, -3.146120232559066537E-19, -0.9999697198139514409 ) ) ;
#35417 = VERTEX_POINT ( 'NONE', #48530 ) ;
#35418 = DIRECTION ( 'NONE',  ( 0.7660212471507180654, -0.6427876096865404731, 0.005961354470445141482 ) ) ;
#35419 = EDGE_CURVE ( 'NONE', #51697, #530, #46933, .T. ) ;
#35420 = CARTESIAN_POINT ( 'NONE',  ( -17.39691609550298068, 0.000000000000000000, 4.885026358070830632 ) ) ;
#35421 = CARTESIAN_POINT ( 'NONE',  ( -19.45503627000849889, 0.000000000000000000, 7.556996783084074742 ) ) ;
#35422 = CARTESIAN_POINT ( 'NONE',  ( -25.20123094555300369, 0.000000000000000000, 6.470945668149052032 ) ) ;
#35423 = CARTESIAN_POINT ( 'NONE',  ( -28.66953870280127248, 14.37385915070733944, -4.739290323461024634 ) ) ;
#35424 = CARTESIAN_POINT ( 'NONE',  ( -24.27063949748155380, 0.000000000000000000, 6.308861732390097288 ) ) ;
#35425 = DIRECTION ( 'NONE',  ( 0.5449076811759707706, 0.6444004775717708799, -0.5364919789714476250 ) ) ;
#35426 = EDGE_CURVE ( 'NONE', #34820, #18978, #42938, .T. ) ;
#35427 = CARTESIAN_POINT ( 'NONE',  ( -66.40965317132554446, 8.186939909977519321E-16, 1.512899686938069088 ) ) ;
#35428 = VERTEX_POINT ( 'NONE', #42393 ) ;
#35429 = FACE_OUTER_BOUND ( 'NONE', #45355, .T. ) ;
#35430 = LINE ( 'NONE', #44495, #4967 ) ;
#35431 = DIRECTION ( 'NONE',  ( 0.7660212471507180654, -0.6427876096865404731, 0.005961354470445141482 ) ) ;
#35432 = DIRECTION ( 'NONE',  ( -0.9999697198139514409, -0.000000000000000000, -0.007781995580013368816 ) ) ;
#35433 = CARTESIAN_POINT ( 'NONE',  ( -17.46532115785441519, 0.000000000000000000, 13.67492996699914265 ) ) ;
#35434 = LINE ( 'NONE', #52480, #52349 ) ;
#35435 = DIRECTION ( 'NONE',  ( 0.007781995580012662783, 0.000000000000000000, -0.9999697198139514409 ) ) ;
#35436 = LINE ( 'NONE', #47672, #39611 ) ;
#35437 = DIRECTION ( 'NONE',  ( 0.9999697198139515519, 0.000000000000000000, 0.007781995580013368816 ) ) ;
#35438 = ORIENTED_EDGE ( 'NONE', *, *, #42416, .F. ) ;
#35439 = VECTOR ( 'NONE', #4531, 1000.000000000000227 ) ;
#35440 = EDGE_CURVE ( 'NONE', #20635, #31613, #5107, .T. ) ;
#35441 = VECTOR ( 'NONE', #13014, 999.9999999999998863 ) ;
#35442 = ORIENTED_EDGE ( 'NONE', *, *, #50895, .T. ) ;
#35443 = ORIENTED_EDGE ( 'NONE', *, *, #51502, .T. ) ;
#35444 = VERTEX_POINT ( 'NONE', #16252 ) ;
#35445 = ORIENTED_EDGE ( 'NONE', *, *, #40275, .F. ) ;
#35446 = LINE ( 'NONE', #17875, #32371 ) ;
#35447 = CARTESIAN_POINT ( 'NONE',  ( 2.072287782118878319, 0.000000000000000000, -2.950529333540147015 ) ) ;
#35448 = ORIENTED_EDGE ( 'NONE', *, *, #68, .T. ) ;
#35449 = ORIENTED_EDGE ( 'NONE', *, *, #54389, .T. ) ;
#35450 = EDGE_CURVE ( 'NONE', #8803, #15287, #56019, .T. ) ;
#35451 = PLANE ( 'NONE',  #22930 ) ;
#35452 = ORIENTED_EDGE ( 'NONE', *, *, #41091, .T. ) ;
#35453 = LINE ( 'NONE', #17884, #42762 ) ;
#35454 = DIRECTION ( 'NONE',  ( -0.005961354470445682716, -0.6427876096865404731, 0.7660212471507180654 ) ) ;
#35455 = ORIENTED_EDGE ( 'NONE', *, *, #14701, .T. ) ;
#35456 = CARTESIAN_POINT ( 'NONE',  ( -18.29747203306047609, -0.1191753592594177458, 14.03778604627889059 ) ) ;
#35457 = ORIENTED_EDGE ( 'NONE', *, *, #39523, .T. ) ;
#35458 = VECTOR ( 'NONE', #1692, 1000.000000000000227 ) ;
#35459 = VECTOR ( 'NONE', #24685, 1000.000000000000000 ) ;
#35460 = CARTESIAN_POINT ( 'NONE',  ( -15.71229329214178883, -1.003701604285656579, 4.432365365500901433 ) ) ;
#35461 = ADVANCED_FACE ( 'NONE', ( #17109 ), #51729, .F. ) ;
#35462 = CARTESIAN_POINT ( 'NONE',  ( -27.06708303904391144, 0.000000000000000000, 7.395095371555332697 ) ) ;
#35463 = EDGE_CURVE ( 'NONE', #56189, #6902, #45371, .T. ) ;
#35464 = DIRECTION ( 'NONE',  ( 0.7660212471507180654, -0.6427876096865404731, 0.005961354470445141482 ) ) ;
#35465 = CARTESIAN_POINT ( 'NONE',  ( -14.01701317841955508, 0.000000000000000000, 2.326005055450897085 ) ) ;
#35466 = ORIENTED_EDGE ( 'NONE', *, *, #11212, .F. ) ;
#35467 = CARTESIAN_POINT ( 'NONE',  ( -27.06552663992790997, 0.000000000000000000, 7.195101427592543786 ) ) ;
#35468 = FACE_OUTER_BOUND ( 'NONE', #20329, .T. ) ;
#35469 = DIRECTION ( 'NONE',  ( -0.005002170337468016433, -0.7660444431189770143, 0.6427681459581293666 ) ) ;
#35470 = ORIENTED_EDGE ( 'NONE', *, *, #14544, .T. ) ;
#35471 = CARTESIAN_POINT ( 'NONE',  ( -11.72624626888112154, -0.1191753592594179401, 5.567817933379076045 ) ) ;
#35472 = ORIENTED_EDGE ( 'NONE', *, *, #1015, .T. ) ;
#35473 = EDGE_CURVE ( 'NONE', #46599, #5827, #15291, .T. ) ;
#35474 = VECTOR ( 'NONE', #9651, 999.9999999999998863 ) ;
#35475 = DIRECTION ( 'NONE',  ( 0.5449076811759707706, 0.6444004775717708799, -0.5364919789714476250 ) ) ;
#35476 = CARTESIAN_POINT ( 'NONE',  ( -17.49243126037356788, 0.000000000000000000, 3.576280771331394437 ) ) ;
#35477 = DIRECTION ( 'NONE',  ( 1.000000000000000000, 0.000000000000000000, 0.000000000000000000 ) ) ;
#35478 = FACE_OUTER_BOUND ( 'NONE', #1964, .T. ) ;
#35479 = DIRECTION ( 'NONE',  ( 0.5449076811759707706, 0.6444004775717708799, -0.5364919789714476250 ) ) ;
#35480 = PLANE ( 'NONE',  #5928 ) ;
#35481 = LINE ( 'NONE', #47726, #48808 ) ;
#35482 = VECTOR ( 'NONE', #13377, 999.9999999999998863 ) ;
#35483 = ADVANCED_FACE ( 'NONE', ( #32350 ), #11009, .F. ) ;
#35484 = FACE_OUTER_BOUND ( 'NONE', #49785, .T. ) ;
#35485 = CARTESIAN_POINT ( 'NONE',  ( -18.42529324785141398, -4.241740624735664156, 3.902997006360208410 ) ) ;
#35486 = VERTEX_POINT ( 'NONE', #15015 ) ;
#35487 = DIRECTION ( 'NONE',  ( -0.5364919789714478471, 0.6444004775717705469, -0.5449076811759709926 ) ) ;
#35488 = DIRECTION ( 'NONE',  ( 0.007781995580012663651, -3.146120232559066537E-19, -0.9999697198139514409 ) ) ;
#35489 = LINE ( 'NONE', #51963, #22719 ) ;
#35490 = DIRECTION ( 'NONE',  ( -0.6427681459581293666, -0.7660444431189770143, -0.005002170337467561935 ) ) ;
#35491 = CARTESIAN_POINT ( 'NONE',  ( -9.044948166384569888, 0.000000000000000000, 6.427351582926061013 ) ) ;
#35492 = CARTESIAN_POINT ( 'NONE',  ( 4.930947970565946470, -1.129146301979396139, -1.967953638240999670 ) ) ;
#35493 = DIRECTION ( 'NONE',  ( -0.005961354470445682716, -0.6427876096865404731, 0.7660212471507180654 ) ) ;
#35494 = EDGE_LOOP ( 'NONE', ( #35951, #8928, #4529, #38037 ) ) ;
#35495 = EDGE_LOOP ( 'NONE', ( #35692, #48762, #55980, #47242 ) ) ;
#35496 = CARTESIAN_POINT ( 'NONE',  ( -19.70704694140911073, 2.714935509636507316, 8.991879102924601241 ) ) ;
#35497 = DIRECTION ( 'NONE',  ( 0.007781995580012663651, 0.000000000000000000, -0.9999697198139515519 ) ) ;
#35498 = ADVANCED_FACE ( 'NONE', ( #2208 ), #49368, .F. ) ;
#35499 = CIRCLE ( 'NONE', #38246, 6.000000000000001776 ) ;
#35500 = AXIS2_PLACEMENT_3D ( 'NONE', #34615, #51933, #30381 ) ;
#35501 = ORIENTED_EDGE ( 'NONE', *, *, #36421, .T. ) ;
#35502 = PLANE ( 'NONE',  #25877 ) ;
#35503 = EDGE_CURVE ( 'NONE', #37777, #8893, #49663, .T. ) ;
#35504 = ORIENTED_EDGE ( 'NONE', *, *, #23547, .F. ) ;
#35505 = CARTESIAN_POINT ( 'NONE',  ( -18.58122884748872039, -3.270328918600660995, 9.266678939965695250 ) ) ;
#35506 = ORIENTED_EDGE ( 'NONE', *, *, #47646, .F. ) ;
#35507 = ORIENTED_EDGE ( 'NONE', *, *, #44318, .T. ) ;
#35508 = ADVANCED_FACE ( 'NONE', ( #53362 ), #23791, .F. ) ;
#35509 = VECTOR ( 'NONE', #18877, 999.9999999999998863 ) ;
#35510 = VERTEX_POINT ( 'NONE', #41121 ) ;
#35511 = EDGE_CURVE ( 'NONE', #43483, #55490, #22967, .T. ) ;
#35512 = CYLINDRICAL_SURFACE ( 'NONE', #14842, 2.749999999999997780 ) ;
#35513 = PLANE ( 'NONE',  #37754 ) ;
#35514 = CARTESIAN_POINT ( 'NONE',  ( -23.33693525117809386, 0.000000000000000000, 5.746789908705562944 ) ) ;
#35515 = ADVANCED_FACE ( 'NONE', ( #1663 ), #40290, .T. ) ;
#35516 = EDGE_CURVE ( 'NONE', #49068, #31601, #10758, .T. ) ;
#35517 = ADVANCED_FACE ( 'NONE', ( #28066 ), #19545, .F. ) ;
#35518 = FACE_OUTER_BOUND ( 'NONE', #53945, .T. ) ;
#35519 = ORIENTED_EDGE ( 'NONE', *, *, #26162, .T. ) ;
#35520 = ORIENTED_EDGE ( 'NONE', *, *, #50663, .F. ) ;
#35521 = AXIS2_PLACEMENT_3D ( 'NONE', #48596, #35824, #9712 ) ;
#35522 = PLANE ( 'NONE',  #47214 ) ;
#35523 = ORIENTED_EDGE ( 'NONE', *, *, #21644, .T. ) ;
#35524 = PLANE ( 'NONE',  #11914 ) ;
#35525 = ORIENTED_EDGE ( 'NONE', *, *, #55046, .T. ) ;
#35526 = FACE_OUTER_BOUND ( 'NONE', #22941, .T. ) ;
#35527 = CARTESIAN_POINT ( 'NONE',  ( -12.55342723663462046, 0.000000000000000000, 5.292051578124692846 ) ) ;
#35528 = EDGE_LOOP ( 'NONE', ( #45269, #47776, #2283, #1299 ) ) ;
#35529 = PLANE ( 'NONE',  #18648 ) ;
#35530 = ADVANCED_FACE ( 'NONE', ( #39998 ), #48821, .F. ) ;
#35531 = ORIENTED_EDGE ( 'NONE', *, *, #37949, .F. ) ;
#35532 = EDGE_CURVE ( 'NONE', #9855, #42909, #1920, .T. ) ;
#35533 = DIRECTION ( 'NONE',  ( -0.005002170337468016433, -0.7660444431189770143, 0.6427681459581293666 ) ) ;
#35534 = ORIENTED_EDGE ( 'NONE', *, *, #56223, .F. ) ;
#35535 = PLANE ( 'NONE',  #4085 ) ;
#35536 = DIRECTION ( 'NONE',  ( -0.6427681459581293666, -0.7660444431189770143, -0.005002170337467561935 ) ) ;
#35537 = ADVANCED_FACE ( 'NONE', ( #23528 ), #19253, .F. ) ;
#35538 = CARTESIAN_POINT ( 'NONE',  ( -14.99594886780042025, -0.1191753592594194527, 7.758364770549599498 ) ) ;
#35539 = VERTEX_POINT ( 'NONE', #14192 ) ;
#35541 = DIRECTION ( 'NONE',  ( -0.9999697198139514409, -0.000000000000000000, -0.007781995580013368816 ) ) ;
#35540 = VECTOR ( 'NONE', #8630, 1000.000000000000227 ) ;
#35542 = EDGE_CURVE ( 'NONE', #44660, #8547, #27224, .T. ) ;
#35543 = VECTOR ( 'NONE', #20801, 1000.000000000000227 ) ;
#35544 = FACE_OUTER_BOUND ( 'NONE', #16509, .T. ) ;
#35545 = FACE_OUTER_BOUND ( 'NONE', #45560, .T. ) ;
#35546 = CARTESIAN_POINT ( 'NONE',  ( -27.33717112119440174, 16.68270265044663603, 4.490773887887534954 ) ) ;
#35547 = PLANE ( 'NONE',  #18608 ) ;
#35548 = LINE ( 'NONE', #35848, #29734 ) ;
#35549 = LINE ( 'NONE', #12854, #29462 ) ;
#35550 = AXIS2_PLACEMENT_3D ( 'NONE', #21849, #39171, #258 ) ;
#35551 = VERTEX_POINT ( 'NONE', #36307 ) ;
#35552 = PLANE ( 'NONE',  #43411 ) ;
#35553 = CARTESIAN_POINT ( 'NONE',  ( -15.87975247367846166, 0.000000000000000000, 2.850166870931599927 ) ) ;
#35554 = LINE ( 'NONE', #48054, #23261 ) ;
#35555 = VERTEX_POINT ( 'NONE', #53618 ) ;
#35556 = CARTESIAN_POINT ( 'NONE',  ( -13.93141126051546408, 0.000000000000000000, 3.234661382569052446 ) ) ;
#35557 = LINE ( 'NONE', #5204, #44476 ) ;
#35558 = ORIENTED_EDGE ( 'NONE', *, *, #4635, .F. ) ;
#35559 = LINE ( 'NONE', #18518, #56104 ) ;
#35560 = FACE_OUTER_BOUND ( 'NONE', #1291, .T. ) ;
#35561 = VECTOR ( 'NONE', #21522, 999.9999999999998863 ) ;
#35562 = DIRECTION ( 'NONE',  ( -1.000000000000000000, 0.000000000000000000, 0.000000000000000000 ) ) ;
#35563 = VECTOR ( 'NONE', #54185, 999.9999999999998863 ) ;
#35564 = FACE_OUTER_BOUND ( 'NONE', #1710, .T. ) ;
#35565 = VERTEX_POINT ( 'NONE', #15543 ) ;
#35566 = ORIENTED_EDGE ( 'NONE', *, *, #50722, .F. ) ;
#35567 = LINE ( 'NONE', #31608, #48487 ) ;
#35568 = DIRECTION ( 'NONE',  ( -0.9999697198139514409, -0.000000000000000000, -0.007781995580013368816 ) ) ;
#35569 = DIRECTION ( 'NONE',  ( 0.9999697198139515519, 0.000000000000000000, 0.007781995580013368816 ) ) ;
#35570 = DIRECTION ( 'NONE',  ( -0.5364919789714478471, 0.6444004775717705469, -0.5449076811759709926 ) ) ;
#35571 = CARTESIAN_POINT ( 'NONE',  ( -27.06552663992790997, 0.000000000000000000, 7.195101427592543786 ) ) ;
#35572 = DIRECTION ( 'NONE',  ( 0.9999697198139515519, 0.000000000000000000, 0.007781995580013368816 ) ) ;
#35573 = VECTOR ( 'NONE', #1567, 1000.000000000000227 ) ;
#35574 = EDGE_LOOP ( 'NONE', ( #39068, #41185, #53729 ) ) ;
#35575 = DIRECTION ( 'NONE',  ( 0.005961354470445682716, -0.6427876096865404731, -0.7660212471507180654 ) ) ;
#35576 = CARTESIAN_POINT ( 'NONE',  ( 4.902479726011971906, 0.000000000000000000, 2.247047898273224931 ) ) ;
#35577 = ADVANCED_FACE ( 'NONE', ( #50189 ), #7061, .F. ) ;
#35578 = ORIENTED_EDGE ( 'NONE', *, *, #46697, .T. ) ;
#35579 = DIRECTION ( 'NONE',  ( 0.000000000000000000, -1.000000000000000000, 0.000000000000000000 ) ) ;
#35580 = VECTOR ( 'NONE', #51892, 1000.000000000000000 ) ;
#35581 = DIRECTION ( 'NONE',  ( 0.2113248654051873565, 0.7886751345948121994, -0.5773502691896263972 ) ) ;
#35582 = CARTESIAN_POINT ( 'NONE',  ( -9.861950574506215261, -0.1191753592594181482, 4.843662173935586956 ) ) ;
#35583 = ADVANCED_FACE ( 'NONE', ( #11298 ), #2503, .F. ) ;
#35584 = EDGE_CURVE ( 'NONE', #38157, #34381, #37717, .T. ) ;
#35585 = VERTEX_POINT ( 'NONE', #42250 ) ;
#35586 = VECTOR ( 'NONE', #33973, 1000.000000000000227 ) ;
#35587 = VECTOR ( 'NONE', #31840, 1000.000000000000114 ) ;
#35588 = FACE_OUTER_BOUND ( 'NONE', #24903, .T. ) ;
#35589 = ORIENTED_EDGE ( 'NONE', *, *, #44687, .T. ) ;
#35590 = EDGE_CURVE ( 'NONE', #33592, #10988, #12450, .T. ) ;
#35591 = ORIENTED_EDGE ( 'NONE', *, *, #46527, .F. ) ;
#35592 = VECTOR ( 'NONE', #35437, 999.9999999999998863 ) ;
#35593 = ORIENTED_EDGE ( 'NONE', *, *, #46179, .F. ) ;
#35594 = AXIS2_PLACEMENT_3D ( 'NONE', #13828, #53324, #39953 ) ;
#35595 = ORIENTED_EDGE ( 'NONE', *, *, #46818, .T. ) ;
#35596 = CARTESIAN_POINT ( 'NONE',  ( -18.20244891691826084, -3.917936722690661178, 10.18238268731339247 ) ) ;
#35597 = ORIENTED_EDGE ( 'NONE', *, *, #51491, .T. ) ;
#35598 = LINE ( 'NONE', #52914, #21311 ) ;
#35599 = LINE ( 'NONE', #44667, #27736 ) ;
#35600 = ORIENTED_EDGE ( 'NONE', *, *, #2039, .T. ) ;
#35601 = CARTESIAN_POINT ( 'NONE',  ( -20.10016216420208579, 4.333955019861511992, 4.351241464568151862 ) ) ;
#35602 = EDGE_LOOP ( 'NONE', ( #26035, #10096, #49480, #36741 ) ) ;
#35604 = AXIS2_PLACEMENT_3D ( 'NONE', #2973, #29101, #28849 ) ;
#35603 = CARTESIAN_POINT ( 'NONE',  ( -13.84799759776688433, -1.003701604285656579, 3.708209606057412344 ) ) ;
#35605 = ORIENTED_EDGE ( 'NONE', *, *, #40174, .T. ) ;
#35606 = EDGE_CURVE ( 'NONE', #18658, #20294, #45648, .T. ) ;
#35607 = CARTESIAN_POINT ( 'NONE',  ( -14.01701317841955508, 0.000000000000000000, 2.326005055450897085 ) ) ;
#35608 = LINE ( 'NONE', #52925, #3905 ) ;
#35609 = CARTESIAN_POINT ( 'NONE',  ( -24.26908309836554878, 0.000000000000000000, 6.108867788427308376 ) ) ;
#35610 = SURFACE_STYLE_FILL_AREA ( #18278 ) ;
#35611 = EDGE_CURVE ( 'NONE', #54767, #42246, #6769, .T. ) ;
#35612 = CARTESIAN_POINT ( 'NONE',  ( -17.74482636761137044, -0.1191753592594197858, 3.674319602356483916 ) ) ;
#35613 = PLANE ( 'NONE',  #14724 ) ;
#35614 = ORIENTED_EDGE ( 'NONE', *, *, #518, .T. ) ;
#35616 = ORIENTED_EDGE ( 'NONE', *, *, #8540, .F. ) ;
#35615 = EDGE_CURVE ( 'NONE', #43426, #37711, #24089, .T. ) ;
#35617 = DIRECTION ( 'NONE',  ( -0.9999697198139514409, -0.000000000000000000, -0.007781995580013368816 ) ) ;
#35618 = CARTESIAN_POINT ( 'NONE',  ( -69.11683642851026832, -9.015837829197110409, 7.493101075386320531 ) ) ;
#35619 = AXIS2_PLACEMENT_3D ( 'NONE', #590, #26407, #5410 ) ;
#35620 = B_SPLINE_CURVE_WITH_KNOTS ( 'NONE', 3,
 ( #3603, #3337, #38234, #11279, #55554, #42232, #33433, #7292 ),
 .UNSPECIFIED., .F., .F.,
 ( 4, 2, 2, 4 ),
 ( 4.816871102115739456E-16, 0.0004770940840306825957, 0.0009541881680608834803, 0.001908376336121245676 ),
 .UNSPECIFIED. ) ;
#35621 = ADVANCED_FACE ( 'NONE', ( #45952 ), #29170, .F. ) ;
#35622 = CARTESIAN_POINT ( 'NONE',  ( -13.08486533123210194, 0.000000000000000000, 1.963927175729152541 ) ) ;
#35623 = CARTESIAN_POINT ( 'NONE',  ( -13.67251641464773115, 0.000000000000000000, 3.975340301736589588 ) ) ;
#35624 = ORIENTED_EDGE ( 'NONE', *, *, #8814, .T. ) ;
#35625 = CARTESIAN_POINT ( 'NONE',  ( -20.54049170961573267, 0.000000000000000000, 4.660556269540326646 ) ) ;
#35626 = DIRECTION ( 'NONE',  ( 0.7660212471507180654, -0.6427876096865404731, 0.005961354470445141482 ) ) ;
#35627 = ORIENTED_EDGE ( 'NONE', *, *, #16576, .T. ) ;
#35629 = FACE_OUTER_BOUND ( 'NONE', #45775, .T. ) ;
#35628 = AXIS2_PLACEMENT_3D ( 'NONE', #22557, #22279, #31055 ) ;
#35630 = CARTESIAN_POINT ( 'NONE',  ( -17.74560456716937296, 0.000000000000000000, 3.774316574337878372 ) ) ;
#35631 = VERTEX_POINT ( 'NONE', #24358 ) ;
#35632 = VECTOR ( 'NONE', #19793, 1000.000000000000227 ) ;
#35633 = VECTOR ( 'NONE', #18094, 1000.000000000000000 ) ;
#35634 = LINE ( 'NONE', #4978, #28863 ) ;
#35635 = LINE ( 'NONE', #36761, #32396 ) ;
#35636 = CARTESIAN_POINT ( 'NONE',  ( -19.69569380384165669, -0.1191753592594177458, 14.58090286586150697 ) ) ;
#35637 = DIRECTION ( 'NONE',  ( 0.5449076811759707706, 0.6444004775717708799, -0.5364919789714476250 ) ) ;
#35638 = DIRECTION ( 'NONE',  ( -0.7660212471507179544, -0.6427876096865405842, -0.005961354470445141482 ) ) ;
#35639 = ORIENTED_EDGE ( 'NONE', *, *, #6050, .F. ) ;
#35640 = AXIS2_PLACEMENT_3D ( 'NONE', #34275, #10680, #14917 ) ;
#35641 = VECTOR ( 'NONE', #54827, 1000.000000000000000 ) ;
#35642 = ORIENTED_EDGE ( 'NONE', *, *, #9461, .T. ) ;
#35643 = DIRECTION ( 'NONE',  ( -0.7660212471507179544, -0.6427876096865405842, -0.005961354470445141482 ) ) ;
#35644 = LINE ( 'NONE', #39061, #13198 ) ;
#35645 = PLANE ( 'NONE',  #53280 ) ;
#35646 = B_SPLINE_CURVE_WITH_KNOTS ( 'NONE', 3,
 ( #33794, #12220, #27235, #30393 ),
 .UNSPECIFIED., .F., .F.,
 ( 4, 4 ),
 ( 0.000000000000000000, 1.000000000000000000 ),
 .UNSPECIFIED. ) ;
#35647 = PLANE ( 'NONE',  #49994 ) ;
#35648 = VECTOR ( 'NONE', #42590, 1000.000000000000000 ) ;
#35649 = CARTESIAN_POINT ( 'NONE',  ( -13.08408713167412074, -0.1191753592594190225, 1.863930203747756975 ) ) ;
#35650 = VERTEX_POINT ( 'NONE', #24929 ) ;
#35652 = VECTOR ( 'NONE', #24342, 1000.000000000000000 ) ;
#35651 = CARTESIAN_POINT ( 'NONE',  ( -12.74479902008156174, 0.000000000000000000, 4.182566069235397421 ) ) ;
#35653 = DIRECTION ( 'NONE',  ( -0.005002170337468016433, -0.7660444431189770143, 0.6427681459581293666 ) ) ;
#35654 = DIRECTION ( 'NONE',  ( 0.5364919789714477361, 0.6444004775717706579, 0.5449076811759711036 ) ) ;
#35655 = CARTESIAN_POINT ( 'NONE',  ( -16.89925026227929195, -0.1191753592594197858, 13.49466922669627422 ) ) ;
#35656 = ORIENTED_EDGE ( 'NONE', *, *, #44650, .F. ) ;
#35657 = LINE ( 'NONE', #10091, #23827 ) ;
#35658 = ORIENTED_EDGE ( 'NONE', *, *, #26887, .F. ) ;
#35659 = CARTESIAN_POINT ( 'NONE',  ( -12.08723394067753176, 0.000000000000000000, 5.095673545929914283 ) ) ;
#35660 = AXIS2_PLACEMENT_3D ( 'NONE', #16834, #818, #48227 ) ;
#35661 = DIRECTION ( 'NONE',  ( 0.5449076811759707706, 0.6444004775717708799, -0.5364919789714476250 ) ) ;
#35662 = EDGE_CURVE ( 'NONE', #32862, #48142, #41668, .T. ) ;
#35663 = ORIENTED_EDGE ( 'NONE', *, *, #18478, .F. ) ;
#35664 = DIRECTION ( 'NONE',  ( 0.007781995580012662783, 0.000000000000000000, -0.9999697198139514409 ) ) ;
#35665 = AXIS2_PLACEMENT_3D ( 'NONE', #53710, #23617, #10287 ) ;
#35666 = EDGE_LOOP ( 'NONE', ( #9546, #2123, #43416, #28024 ) ) ;
#35667 = EDGE_CURVE ( 'NONE', #6678, #18137, #12136, .T. ) ;
#35668 = EDGE_CURVE ( 'NONE', #931, #25817, #2753, .T. ) ;
#35669 = ORIENTED_EDGE ( 'NONE', *, *, #40678, .F. ) ;
#35670 = ORIENTED_EDGE ( 'NONE', *, *, #2856, .F. ) ;
#35671 = FACE_OUTER_BOUND ( 'NONE', #35333, .T. ) ;
#35672 = ORIENTED_EDGE ( 'NONE', *, *, #14519, .F. ) ;
#35673 = ORIENTED_EDGE ( 'NONE', *, *, #53089, .T. ) ;
#35674 = VECTOR ( 'NONE', #32644, 1000.000000000000114 ) ;
#35675 = CARTESIAN_POINT ( 'NONE',  ( -18.86992194539476131, -3.108426967578160838, 4.111864531351901775 ) ) ;
#35676 = LINE ( 'NONE', #27153, #54826 ) ;
#35677 = ORIENTED_EDGE ( 'NONE', *, *, #45270, .F. ) ;
#35678 = VECTOR ( 'NONE', #14370, 1000.000000000000114 ) ;
#35679 = VECTOR ( 'NONE', #22576, 1000.000000000000227 ) ;
#35680 = EDGE_LOOP ( 'NONE', ( #2947, #55007, #12380, #7658 ) ) ;
#35681 = DIRECTION ( 'NONE',  ( 0.5449076811759707706, 0.6444004775717708799, -0.5364919789714476250 ) ) ;
#35682 = ORIENTED_EDGE ( 'NONE', *, *, #10070, .F. ) ;
#35683 = VERTEX_POINT ( 'NONE', #41416 ) ;
#35684 = VECTOR ( 'NONE', #46913, 1000.000000000000000 ) ;
#35685 = VECTOR ( 'NONE', #16213, 1000.000000000000227 ) ;
#35686 = CARTESIAN_POINT ( 'NONE',  ( -28.92982233430281980, 0.000000000000000000, 7.919257187036034651 ) ) ;
#35687 = FACE_OUTER_BOUND ( 'NONE', #54008, .T. ) ;
#35688 = CARTESIAN_POINT ( 'NONE',  ( 2.602374448188125350E-16, 0.000000000000000000, -2.125000000000000000 ) ) ;
#35689 = DIRECTION ( 'NONE',  ( -0.5364919789714478471, 0.6444004775717705469, -0.5449076811759709926 ) ) ;
#35690 = ORIENTED_EDGE ( 'NONE', *, *, #20968, .F. ) ;
#35691 = CARTESIAN_POINT ( 'NONE',  ( -13.08408713167409942, -0.1191753592594197858, 1.863930203747758085 ) ) ;
#35692 = ORIENTED_EDGE ( 'NONE', *, *, #56223, .T. ) ;
#35693 = CARTESIAN_POINT ( 'NONE',  ( -27.99845268667336384, -0.1191753592594197858, 7.657176279295684118 ) ) ;
#35694 = EDGE_CURVE ( 'NONE', #43321, #10765, #46793, .T. ) ;
#35695 = CARTESIAN_POINT ( 'NONE',  ( -12.27441401622991002, 0.000000000000000000, 3.447562574487877729 ) ) ;
#35696 = LINE ( 'NONE', #31456, #24957 ) ;
#35697 = CARTESIAN_POINT ( 'NONE',  ( -27.06552663992790997, 0.000000000000000000, 7.195101427592543786 ) ) ;
#35698 = VECTOR ( 'NONE', #16896, 1000.000000000000227 ) ;
#35699 = ADVANCED_FACE ( 'NONE', ( #20078 ), #54442, .F. ) ;
#35700 = LINE ( 'NONE', #53016, #390 ) ;
#35701 = LINE ( 'NONE', #23481, #43882 ) ;
#35702 = LINE ( 'NONE', #498, #54905 ) ;
#35703 = ORIENTED_EDGE ( 'NONE', *, *, #2101, .T. ) ;
#35704 = CARTESIAN_POINT ( 'NONE',  ( -10.32083936433673621, -0.1191753592594190225, 4.101426855652049674 ) ) ;
#35705 = EDGE_CURVE ( 'NONE', #24424, #23097, #46481, .T. ) ;
#35706 = AXIS2_PLACEMENT_3D ( 'NONE', #30313, #17523, #34856 ) ;
#35707 = CARTESIAN_POINT ( 'NONE',  ( 2.072287782118878319, 0.000000000000000000, -2.950529333540147015 ) ) ;
#35708 = DIRECTION ( 'NONE',  ( 0.000000000000000000, -0.000000000000000000, -1.000000000000000000 ) ) ;
#35709 = CARTESIAN_POINT ( 'NONE',  ( -19.12962290826653700, 0.000000000000000000, 14.40064212555863854 ) ) ;
#35710 = EDGE_CURVE ( 'NONE', #11776, #1716, #33177, .T. ) ;
#35711 = VECTOR ( 'NONE', #41577, 999.9999999999998863 ) ;
#35712 = CARTESIAN_POINT ( 'NONE',  ( -19.69488366597744289, 19.55537865210161996, -4.316569728936750394 ) ) ;
#35713 = DIRECTION ( 'NONE',  ( -0.6427681459581293666, -0.7660444431189770143, -0.005002170337467561935 ) ) ;
#35714 = DIRECTION ( 'NONE',  ( 0.007781995580012663651, 0.000000000000000000, -0.9999697198139515519 ) ) ;
#35715 = CARTESIAN_POINT ( 'NONE',  ( -67.56320601492518563, -0.9999999999999978906, -2.442027903730110250 ) ) ;
#35716 = EDGE_LOOP ( 'NONE', ( #23563, #4513, #35145, #55347 ) ) ;
#35717 = AXIS2_PLACEMENT_3D ( 'NONE', #50091, #2946, #2112 ) ;
#35718 = CARTESIAN_POINT ( 'NONE',  ( -12.19088316572221231, -0.1191753592594179401, 5.564202021611067472 ) ) ;
#35719 = FACE_OUTER_BOUND ( 'NONE', #12496, .T. ) ;
#35720 = CARTESIAN_POINT ( 'NONE',  ( -8.875996589204540044, 0.000000000000000000, 10.41778544861944233 ) ) ;
#35721 = VECTOR ( 'NONE', #8038, 1000.000000000000227 ) ;
#35722 = DIRECTION ( 'NONE',  ( -0.5364919789714478471, 0.6444004775717705469, -0.5449076811759709926 ) ) ;
#35723 = FACE_OUTER_BOUND ( 'NONE', #7141, .T. ) ;
#35724 = CYLINDRICAL_SURFACE ( 'NONE', #15926, 3.000000000000001332 ) ;
#35725 = EDGE_CURVE ( 'NONE', #9862, #38231, #28910, .T. ) ;
#35726 = PLANE ( 'NONE',  #25603 ) ;
#35727 = VECTOR ( 'NONE', #26473, 999.9999999999998863 ) ;
#35728 = AXIS2_PLACEMENT_3D ( 'NONE', #9367, #22710, #36081 ) ;
#35729 = CARTESIAN_POINT ( 'NONE',  ( -24.62525945952572215, 18.15220053346460105, -4.407437592157546824 ) ) ;
#35730 = CARTESIAN_POINT ( 'NONE',  ( -22.40478740399063895, 0.000000000000000000, 5.384712028983816623 ) ) ;
#35731 = EDGE_CURVE ( 'NONE', #18997, #24292, #41941, .T. ) ;
#35732 = ORIENTED_EDGE ( 'NONE', *, *, #22007, .T. ) ;
#35733 = ADVANCED_FACE ( 'NONE', ( #490 ), #34303, .F. ) ;
#35734 = EDGE_CURVE ( 'NONE', #42927, #47502, #43919, .T. ) ;
#35735 = EDGE_LOOP ( 'NONE', ( #3595, #33780, #11494 ) ) ;
#35736 = VERTEX_POINT ( 'NONE', #35157 ) ;
#35737 = ORIENTED_EDGE ( 'NONE', *, *, #38943, .T. ) ;
#35738 = AXIS2_PLACEMENT_3D ( 'NONE', #50314, #41530, #40952 ) ;
#35739 = ORIENTED_EDGE ( 'NONE', *, *, #3863, .T. ) ;
#35740 = PLANE ( 'NONE',  #34194 ) ;
#35741 = DIRECTION ( 'NONE',  ( 0.005002170337468016433, -0.7660444431189770143, -0.6427681459581293666 ) ) ;
#35742 = AXIS2_PLACEMENT_3D ( 'NONE', #1797, #44995, #9802 ) ;
#35743 = ORIENTED_EDGE ( 'NONE', *, *, #53944, .T. ) ;
#35744 = ORIENTED_EDGE ( 'NONE', *, *, #2956, .F. ) ;
#35745 = AXIS2_PLACEMENT_3D ( 'NONE', #24987, #50550, #46257 ) ;
#35746 = EDGE_CURVE ( 'NONE', #36489, #25453, #18084, .T. ) ;
#35747 = FACE_OUTER_BOUND ( 'NONE', #42883, .T. ) ;
#35748 = ORIENTED_EDGE ( 'NONE', *, *, #40815, .T. ) ;
#35749 = VECTOR ( 'NONE', #24465, 1000.000000000000114 ) ;
#35750 = LINE ( 'NONE', #18717, #45477 ) ;
#35751 = LINE ( 'NONE', #5938, #36823 ) ;
#35752 = ORIENTED_EDGE ( 'NONE', *, *, #48684, .T. ) ;
#35753 = CARTESIAN_POINT ( 'NONE',  ( -15.06798350428698896, 0.000000000000000000, 4.164486510395348340 ) ) ;
#35754 = AXIS2_PLACEMENT_3D ( 'NONE', #40656, #18803, #36124 ) ;
#35755 = EDGE_LOOP ( 'NONE', ( #17580, #23691, #36230, #50729 ) ) ;
#35756 = CARTESIAN_POINT ( 'NONE',  ( -14.10280672071693431, -0.1191753592594197858, 12.40843558753103792 ) ) ;
#35757 = DIRECTION ( 'NONE',  ( 0.007781995580012663651, 0.000000000000000000, -0.9999697198139515519 ) ) ;
#35758 = AXIS2_PLACEMENT_3D ( 'NONE', #30641, #52204, #34884 ) ;
#35759 = LINE ( 'NONE', #36059, #20955 ) ;
#35760 = CARTESIAN_POINT ( 'NONE',  ( -26.13493519185646008, 0.000000000000000000, 7.033017491833586377 ) ) ;
#35761 = ORIENTED_EDGE ( 'NONE', *, *, #15688, .T. ) ;
#35762 = FACE_OUTER_BOUND ( 'NONE', #49763, .T. ) ;
#35763 = DIRECTION ( 'NONE',  ( 0.9999697198139515519, 0.000000000000000000, 0.007781995580013368816 ) ) ;
#35764 = CARTESIAN_POINT ( 'NONE',  ( -19.77061338776520216, 21.24370688441071664, -4.657437592157546824 ) ) ;
#35765 = ORIENTED_EDGE ( 'NONE', *, *, #30444, .T. ) ;
#35766 = CARTESIAN_POINT ( 'NONE',  ( -19.60834386242827776, 0.000000000000000000, 4.298478389818581213 ) ) ;
#35767 = VERTEX_POINT ( 'NONE', #30025 ) ;
#35768 = CARTESIAN_POINT ( 'NONE',  ( -23.33849165029409889, 0.000000000000000000, 5.946783852668351855 ) ) ;
#35769 = DIRECTION ( 'NONE',  ( 0.005961354470445682716, -0.6427876096865404731, -0.7660212471507180654 ) ) ;
#35770 = LINE ( 'NONE', #5654, #24060 ) ;
#35771 = PLANE ( 'NONE',  #48645 ) ;
#35772 = EDGE_CURVE ( 'NONE', #55300, #12199, #43633, .T. ) ;
#35773 = LINE ( 'NONE', #53095, #21402 ) ;
#35774 = DIRECTION ( 'NONE',  ( -0.005961354470445682716, -0.6427876096865404731, 0.7660212471507180654 ) ) ;
#35775 = DIRECTION ( 'NONE',  ( 0.000000000000000000, -1.000000000000000000, 0.000000000000000000 ) ) ;
#35776 = VECTOR ( 'NONE', #33387, 999.9999999999998863 ) ;
#35777 = DIRECTION ( 'NONE',  ( 0.7660212471507180654, -0.6427876096865404731, 0.005961354470445141482 ) ) ;
#35778 =( NAMED_UNIT ( * ) PLANE_ANGLE_UNIT ( ) SI_UNIT ( $, .RADIAN. ) );
#35779 = VECTOR ( 'NONE', #33776, 999.9999999999998863 ) ;
#35780 = CARTESIAN_POINT ( 'NONE',  ( -19.72742537039871280, 2.229229656569007734, 4.273609594196196682 ) ) ;
#35781 = ORIENTED_EDGE ( 'NONE', *, *, #12978, .F. ) ;
#35782 = CARTESIAN_POINT ( 'NONE',  ( -16.33317936670417225, 0.000000000000000000, 13.31440848639340224 ) ) ;
#35783 = FACE_OUTER_BOUND ( 'NONE', #42614, .T. ) ;
#35784 = CARTESIAN_POINT ( 'NONE',  ( -16.89925026227929195, -0.1191753592594197858, 13.49466922669627422 ) ) ;
#35785 = AXIS2_PLACEMENT_3D ( 'NONE', #52581, #31845, #30992 ) ;
#35786 = DIRECTION ( 'NONE',  ( -0.005002170337468016433, -0.7660444431189770143, 0.6427681459581293666 ) ) ;
#35787 = EDGE_CURVE ( 'NONE', #5570, #21771, #22065, .T. ) ;
#35788 = DIRECTION ( 'NONE',  ( 0.007781995580012663651, -3.146120232559066537E-19, -0.9999697198139514409 ) ) ;
#35789 = ADVANCED_FACE ( 'NONE', ( #39395 ), #21526, .F. ) ;
#35790 = DIRECTION ( 'NONE',  ( 0.000000000000000000, -1.000000000000000000, 0.000000000000000000 ) ) ;
#35791 = EDGE_CURVE ( 'NONE', #3166, #21903, #39687, .T. ) ;
#35792 = CARTESIAN_POINT ( 'NONE',  ( -20.51801655564820237, -5.536956232915664522, 13.73891463470874186 ) ) ;
#35793 = ORIENTED_EDGE ( 'NONE', *, *, #10484, .T. ) ;
#35794 = AXIS2_PLACEMENT_3D ( 'NONE', #43636, #48171, #47922 ) ;
#35795 = ORIENTED_EDGE ( 'NONE', *, *, #667, .T. ) ;
#35796 = CARTESIAN_POINT ( 'NONE',  ( 0.1285714285714296967, 2.000000000000000000, -5.998622290806041590 ) ) ;
#35797 = AXIS2_PLACEMENT_3D ( 'NONE', #7358, #229, #805 ) ;
#35798 = PLANE ( 'NONE',  #17744 ) ;
#35799 = ADVANCED_FACE ( 'NONE', ( #8441 ), #52453, .F. ) ;
#35800 = VECTOR ( 'NONE', #23948, 1000.000000000000227 ) ;
#35801 = ORIENTED_EDGE ( 'NONE', *, *, #24960, .T. ) ;
#35802 = ADVANCED_FACE ( 'NONE', ( #30862 ), #3893, .F. ) ;
#35803 = FACE_OUTER_BOUND ( 'NONE', #11962, .T. ) ;
#35804 = VERTEX_POINT ( 'NONE', #48167 ) ;
#35805 = LINE ( 'NONE', #53401, #51051 ) ;
#35806 = EDGE_CURVE ( 'NONE', #41646, #52618, #43380, .T. ) ;
#35807 = VECTOR ( 'NONE', #49260, 1000.000000000000000 ) ;
#35808 = ORIENTED_EDGE ( 'NONE', *, *, #31364, .F. ) ;
#35809 = AXIS2_PLACEMENT_3D ( 'NONE', #8790, #38284, #17266 ) ;
#35810 = VERTEX_POINT ( 'NONE', #22371 ) ;
#35811 = EDGE_LOOP ( 'NONE', ( #47460, #55813, #7243, #6467 ) ) ;
#35812 = DIRECTION ( 'NONE',  ( 0.007781995580012662783, 0.000000000000000000, -0.9999697198139514409 ) ) ;
#35813 = LINE ( 'NONE', #5998, #28669 ) ;
#35814 = DIRECTION ( 'NONE',  ( 1.000000000000000000, 0.000000000000000000, 0.000000000000000000 ) ) ;
#35815 = EDGE_CURVE ( 'NONE', #31029, #37945, #35408, .T. ) ;
#35816 = CARTESIAN_POINT ( 'NONE',  ( -18.78507867901567252, 0.000000000000000000, 4.135559216251272652 ) ) ;
#35817 = EDGE_LOOP ( 'NONE', ( #46310, #7999, #27635, #31493 ) ) ;
#35818 = ORIENTED_EDGE ( 'NONE', *, *, #3116, .F. ) ;
#35819 = VECTOR ( 'NONE', #11034, 1000.000000000000227 ) ;
#35820 = ADVANCED_FACE ( 'NONE', ( #177 ), #52169, .F. ) ;
#35821 = CARTESIAN_POINT ( 'NONE',  ( -68.84267254591711094, -9.186009798224464618, -7.487678583014048428 ) ) ;
#35822 = VECTOR ( 'NONE', #14110, 999.9999999999998863 ) ;
#35823 = ORIENTED_EDGE ( 'NONE', *, *, #18487, .T. ) ;
#35824 = DIRECTION ( 'NONE',  ( 0.7660212471507180654, -0.6427876096865404731, 0.005961354470445141482 ) ) ;
#35825 = ORIENTED_EDGE ( 'NONE', *, *, #27734, .F. ) ;
#35826 = VECTOR ( 'NONE', #14604, 999.9999999999998863 ) ;
#35827 = CYLINDRICAL_SURFACE ( 'NONE', #22412, 2.125000000000000000 ) ;
#35828 = CARTESIAN_POINT ( 'NONE',  ( 2.072287782118878319, 0.000000000000000000, -2.950529333540147015 ) ) ;
#35829 = ORIENTED_EDGE ( 'NONE', *, *, #27128, .F. ) ;
#35830 = CARTESIAN_POINT ( 'NONE',  ( -18.23978498517217517, -0.1191753592594166911, 6.625124278400236655 ) ) ;
#35831 = VECTOR ( 'NONE', #20149, 1000.000000000000114 ) ;
#35832 = ORIENTED_EDGE ( 'NONE', *, *, #33158, .T. ) ;
#35833 = CARTESIAN_POINT ( 'NONE',  ( -15.44621549711509090, -0.1191753592594185784, 5.908200342492767376 ) ) ;
#35834 = AXIS2_PLACEMENT_3D ( 'NONE', #15405, #24476, #28183 ) ;
#35835 = VERTEX_POINT ( 'NONE', #8169 ) ;
#35836 = DIRECTION ( 'NONE',  ( 0.9999697198139515519, 0.000000000000000000, 0.007781995580013368816 ) ) ;
#35837 = CARTESIAN_POINT ( 'NONE',  ( -17.93139508144814442, 0.000000000000000000, 13.85596890686001537 ) ) ;
#35838 = AXIS2_PLACEMENT_3D ( 'NONE', #56089, #47847, #102 ) ;
#35839 = CARTESIAN_POINT ( 'NONE',  ( -56.00000000000000711, 3.800000000000001599, 1.887458608817694561 ) ) ;
#35840 = ORIENTED_EDGE ( 'NONE', *, *, #47318, .F. ) ;
#35841 = VECTOR ( 'NONE', #8306, 1000.000000000000114 ) ;
#35842 = DIRECTION ( 'NONE',  ( -0.6427681459581293666, -0.7660444431189770143, -0.005002170337467561935 ) ) ;
#35843 = CARTESIAN_POINT ( 'NONE',  ( -19.45497020661647269, 1.905425754524007642, 4.178109795741645982 ) ) ;
#35844 = ADVANCED_FACE ( 'NONE', ( #42787 ), #21218, .F. ) ;
#35845 = EDGE_CURVE ( 'NONE', #32241, #24728, #38549, .T. ) ;
#35846 = CARTESIAN_POINT ( 'NONE',  ( -56.56312404709360919, 4.044422194259722936, -2.346569400431943730 ) ) ;
#35847 = CARTESIAN_POINT ( 'NONE',  ( -11.66794108741423308, 2.067327705546508021, 1.148197717334086043 ) ) ;
#35848 = CARTESIAN_POINT ( 'NONE',  ( -14.66887761629205222, 0.000000000000000000, 12.58869632783390990 ) ) ;
#35849 = VECTOR ( 'NONE', #31250, 1000.000000000000000 ) ;
#35850 = VECTOR ( 'NONE', #50956, 1000.000000000000114 ) ;
#35851 = CARTESIAN_POINT ( 'NONE',  ( -66.21705755929110637, -11.30109441652609270, 6.550948917181726117 ) ) ;
#35852 = ORIENTED_EDGE ( 'NONE', *, *, #2381, .F. ) ;
#35853 = CARTESIAN_POINT ( 'NONE',  ( -15.86710544311044302, 0.000000000000000000, 13.13336954653252953 ) ) ;
#35854 = LINE ( 'NONE', #39821, #10476 ) ;
#35855 = PLANE ( 'NONE',  #45035 ) ;
#35856 = EDGE_LOOP ( 'NONE', ( #20684, #43995, #42063, #21337 ) ) ;
#35857 = CARTESIAN_POINT ( 'NONE',  ( -12.80458192191714595, 0.000000000000000000, 11.86454056839041726 ) ) ;
#35858 = DIRECTION ( 'NONE',  ( -0.6427681459581293666, -0.7660444431189770143, -0.005002170337467561935 ) ) ;
#35859 = ORIENTED_EDGE ( 'NONE', *, *, #37571, .F. ) ;
#35860 = ADVANCED_FACE ( 'NONE', ( #43094 ), #12990, .F. ) ;
#35861 = EDGE_CURVE ( 'NONE', #16010, #55867, #48464, .T. ) ;
#35862 = DIRECTION ( 'NONE',  ( -0.9321478471874540261, 0.000000000000000000, 0.3620778797217457656 ) ) ;
#35863 = CARTESIAN_POINT ( 'NONE',  ( -13.07066190154808361, 0.000000000000000000, 12.04713590736729678 ) ) ;
#35864 = DIRECTION ( 'NONE',  ( -0.5449076811759708816, 0.6444004775717707689, 0.5364919789714475140 ) ) ;
#35865 = EDGE_CURVE ( 'NONE', #54123, #52222, #49304, .T. ) ;
#35866 = DIRECTION ( 'NONE',  ( 1.000000000000000000, 0.000000000000000000, -0.000000000000000000 ) ) ;
#35867 = VECTOR ( 'NONE', #31092, 1000.000000000000227 ) ;
#35868 = VERTEX_POINT ( 'NONE', #53837 ) ;
#35869 = ORIENTED_EDGE ( 'NONE', *, *, #16808, .F. ) ;
#35870 = VECTOR ( 'NONE', #20008, 999.9999999999998863 ) ;
#35871 = CARTESIAN_POINT ( 'NONE',  ( -22.05458030558363092, -5.698858183938162902, 14.60147686105872111 ) ) ;
#35872 = DIRECTION ( 'NONE',  ( 0.007781995580012662783, 0.000000000000000000, -0.9999697198139514409 ) ) ;
#35873 = CARTESIAN_POINT ( 'NONE',  ( -15.87975247367846166, 0.000000000000000000, 2.850166870931599927 ) ) ;
#35874 = VECTOR ( 'NONE', #6712, 999.9999999999998863 ) ;
#35875 = LINE ( 'NONE', #53715, #23893 ) ;
#35876 = CARTESIAN_POINT ( 'NONE',  ( -18.17048319147368218, 2.553033558614007603, 8.129316876574623763 ) ) ;
#35877 = EDGE_CURVE ( 'NONE', #3706, #28890, #6431, .T. ) ;
#35878 = DIRECTION ( 'NONE',  ( 0.5449076811759707706, 0.6444004775717708799, -0.5364919789714476250 ) ) ;
#35879 = VECTOR ( 'NONE', #20380, 1000.000000000000227 ) ;
#35880 = ORIENTED_EDGE ( 'NONE', *, *, #45389, .F. ) ;
#35881 = DIRECTION ( 'NONE',  ( -0.9999697198139514409, -0.000000000000000000, -0.007781995580013368816 ) ) ;
#35882 = ADVANCED_FACE ( 'NONE', ( #10710 ), #36825, .F. ) ;
#35883 = LINE ( 'NONE', #14309, #54960 ) ;
#35884 = VECTOR ( 'NONE', #35273, 1000.000000000000227 ) ;
#35886 = ORIENTED_EDGE ( 'NONE', *, *, #26952, .T. ) ;
#35885 = VECTOR ( 'NONE', #23394, 1000.000000000000114 ) ;
#35887 = EDGE_CURVE ( 'NONE', #16295, #19155, #6175, .T. ) ;
#35888 = LINE ( 'NONE', #27631, #47420 ) ;
#35889 = FACE_OUTER_BOUND ( 'NONE', #5735, .T. ) ;
#35890 = DIRECTION ( 'NONE',  ( 0.5449076811759707706, 0.6444004775717708799, -0.5364919789714476250 ) ) ;
#35891 = VECTOR ( 'NONE', #4227, 1000.000000000000227 ) ;
#35892 = ORIENTED_EDGE ( 'NONE', *, *, #32249, .T. ) ;
#35893 = ADVANCED_FACE ( 'NONE', ( #41058 ), #53559, .F. ) ;
#35894 = VECTOR ( 'NONE', #2346, 1000.000000000000114 ) ;
#35895 = DIRECTION ( 'NONE',  ( 0.000000000000000000, 0.000000000000000000, 1.000000000000000000 ) ) ;
#35896 = VERTEX_POINT ( 'NONE', #28018 ) ;
#35897 = AXIS2_PLACEMENT_3D ( 'NONE', #10093, #4714, #44191 ) ;
#35898 = ORIENTED_EDGE ( 'NONE', *, *, #24418, .T. ) ;
#35899 = VECTOR ( 'NONE', #46652, 999.9999999999998863 ) ;
#35900 = ORIENTED_EDGE ( 'NONE', *, *, #48930, .F. ) ;
#35901 = EDGE_LOOP ( 'NONE', ( #54739, #14360, #22955, #40885 ) ) ;
#35902 = CARTESIAN_POINT ( 'NONE',  ( -67.55782011861325032, -8.435184460786505412, -3.909888324369926060 ) ) ;
#35903 = ORIENTED_EDGE ( 'NONE', *, *, #27194, .T. ) ;
#35904 = CARTESIAN_POINT ( 'NONE',  ( -10.37421533196711465, -0.1191753592594197858, 10.96012406864405975 ) ) ;
#35905 = DIRECTION ( 'NONE',  ( 0.005002170337468016433, -0.7660444431189770143, -0.6427681459581293666 ) ) ;
#35906 = EDGE_LOOP ( 'NONE', ( #48277, #54242, #32805, #28145 ) ) ;
#35907 = CARTESIAN_POINT ( 'NONE',  ( -12.73749451395499577, 0.000000000000000000, 3.243952718757078912 ) ) ;
#35908 = ORIENTED_EDGE ( 'NONE', *, *, #4456, .F. ) ;
#35909 = CARTESIAN_POINT ( 'NONE',  ( -10.40724426834971794, 0.000000000000000000, 2.354097111786622065 ) ) ;
#35910 = ORIENTED_EDGE ( 'NONE', *, *, #37786, .T. ) ;
#35911 = AXIS2_PLACEMENT_3D ( 'NONE', #37518, #54282, #19658 ) ;
#35912 = PLANE ( 'NONE',  #31012 ) ;
#35913 = LINE ( 'NONE', #52384, #22076 ) ;
#35914 = VECTOR ( 'NONE', #23832, 1000.000000000000227 ) ;
#35915 = DIRECTION ( 'NONE',  ( 0.005002170337468016433, -0.7660444431189770143, -0.6427681459581293666 ) ) ;
#35916 = DIRECTION ( 'NONE',  ( 0.6246952433987893460, 0.7422098413412802076, -0.2426528472758539279 ) ) ;
#35917 = DIRECTION ( 'NONE',  ( 0.9999697198139515519, 0.000000000000000000, 0.007781995580013368816 ) ) ;
#35918 = DIRECTION ( 'NONE',  ( -0.5449076811759708816, 0.6444004775717707689, 0.5364919789714475140 ) ) ;
#35919 = VECTOR ( 'NONE', #29714, 1000.000000000000227 ) ;
#35920 = ORIENTED_EDGE ( 'NONE', *, *, #51624, .F. ) ;
#35921 = ADVANCED_FACE ( 'NONE', ( #45323 ), #23477, .F. ) ;
#35922 = VERTEX_POINT ( 'NONE', #40794 ) ;
#35923 = CYLINDRICAL_SURFACE ( 'NONE', #20081, 2.749999999999999112 ) ;
#35924 = LINE ( 'NONE', #44154, #30310 ) ;
#35925 = VECTOR ( 'NONE', #8898, 1000.000000000000114 ) ;
#35926 = EDGE_CURVE ( 'NONE', #40269, #24198, #1864, .T. ) ;
#35927 = DIRECTION ( 'NONE',  ( -0.5449076811759708816, 0.6444004775717707689, 0.5364919789714475140 ) ) ;
#35928 = VECTOR ( 'NONE', #1934, 1000.000000000000114 ) ;
#35929 = VECTOR ( 'NONE', #8366, 1000.000000000000227 ) ;
#35930 = LINE ( 'NONE', #48962, #21313 ) ;
#35931 = ORIENTED_EDGE ( 'NONE', *, *, #5016, .F. ) ;
#35932 = DIRECTION ( 'NONE',  ( 0.7660212471507180654, -0.6427876096865404731, 0.005961354470445141482 ) ) ;
#35933 = CARTESIAN_POINT ( 'NONE',  ( -16.79925329029790149, 0.000000000000000000, 13.49544742625427496 ) ) ;
#35934 = ORIENTED_EDGE ( 'NONE', *, *, #38197, .F. ) ;
#35935 = CARTESIAN_POINT ( 'NONE',  ( -13.07066190154808361, 0.000000000000000000, 12.04713590736729678 ) ) ;
#35936 = VECTOR ( 'NONE', #15772, 999.9999999999998863 ) ;
#35937 = DIRECTION ( 'NONE',  ( 0.005002170337468016433, -0.7660444431189770143, -0.6427681459581293666 ) ) ;
#35938 = VERTEX_POINT ( 'NONE', #9585 ) ;
#35939 = ADVANCED_FACE ( 'NONE', ( #26906 ), #5324, .F. ) ;
#35940 = AXIS2_PLACEMENT_3D ( 'NONE', #42484, #47022, #29122 ) ;
#35941 = ADVANCED_FACE ( 'NONE', ( #39940 ), #36258, .F. ) ;
#35942 = EDGE_CURVE ( 'NONE', #44182, #44163, #36520, .T. ) ;
#35943 = CARTESIAN_POINT ( 'NONE',  ( -66.99840443968177794, -8.772812340773230133, 3.326521589947848412 ) ) ;
#35944 = CARTESIAN_POINT ( 'NONE',  ( -9.864824628011497509, -0.1191753592594181482, 5.212971877193351311 ) ) ;
#35945 = AXIS2_PLACEMENT_3D ( 'NONE', #42523, #8436, #38242 ) ;
#35946 = DIRECTION ( 'NONE',  ( 0.007781995580012663651, -3.146120232559066537E-19, -0.9999697198139514409 ) ) ;
#35947 = EDGE_CURVE ( 'NONE', #52744, #38022, #14663, .T. ) ;
#35948 = CARTESIAN_POINT ( 'NONE',  ( -17.83139810946674686, -0.1191753592594197858, 13.85674710641801788 ) ) ;
#35949 = VECTOR ( 'NONE', #35581, 1000.000000000000114 ) ;
#35950 = PLANE ( 'NONE',  #55545 ) ;
#35951 = ORIENTED_EDGE ( 'NONE', *, *, #31565, .T. ) ;
#35952 = VECTOR ( 'NONE', #7860, 1000.000000000000227 ) ;
#35953 = ORIENTED_EDGE ( 'NONE', *, *, #34675, .T. ) ;
#35954 = CARTESIAN_POINT ( 'NONE',  ( -16.29483249379484633, 0.000000000000000000, 8.386917669337709214 ) ) ;
#35955 = CARTESIAN_POINT ( 'NONE',  ( -14.46888367232926420, 0.000000000000000000, 12.59025272694991315 ) ) ;
#35956 = DIRECTION ( 'NONE',  ( -0.7660212471507179544, -0.6427876096865405842, -0.005961354470445141482 ) ) ;
#35957 = DIRECTION ( 'NONE',  ( 0.5364919789714477361, 0.6444004775717706579, 0.5449076811759711036 ) ) ;
#35958 = CARTESIAN_POINT ( 'NONE',  ( -27.06630483948590893, -0.1191753592594197858, 7.295098399573937797 ) ) ;
#35959 = ORIENTED_EDGE ( 'NONE', *, *, #44688, .F. ) ;
#35960 = LINE ( 'NONE', #53277, #45503 ) ;
#35961 = DIRECTION ( 'NONE',  ( -0.005961354470445682716, -0.6427876096865404731, 0.7660212471507180654 ) ) ;
#35962 = EDGE_CURVE ( 'NONE', #6097, #36189, #44475, .T. ) ;
#35963 = AXIS2_PLACEMENT_3D ( 'NONE', #45408, #38507, #23831 ) ;
#35964 = ADVANCED_FACE ( 'NONE', ( #40227 ), #1314, .F. ) ;
#35965 = DIRECTION ( 'NONE',  ( 0.7660212471507180654, -0.6427876096865404731, 0.005961354470445141482 ) ) ;
#35966 = PLANE ( 'NONE',  #10631 ) ;
#35967 = ORIENTED_EDGE ( 'NONE', *, *, #43866, .F. ) ;
#35968 = ADVANCED_FACE ( 'NONE', ( #10123 ), #31986, .F. ) ;
#35969 = DIRECTION ( 'NONE',  ( -0.6246952433987894571, 0.7422098413412802076, 0.2426528472758539834 ) ) ;
#35970 = ORIENTED_EDGE ( 'NONE', *, *, #41013, .T. ) ;
#35971 = CARTESIAN_POINT ( 'NONE',  ( 2.072287782118878319, 0.000000000000000000, -2.950529333540147015 ) ) ;
#35972 = VECTOR ( 'NONE', #13076, 999.9999999999998863 ) ;
#35973 = CARTESIAN_POINT ( 'NONE',  ( -17.41835212442924430, 0.000000000000000000, 7.639510040170157446 ) ) ;
#35974 = ORIENTED_EDGE ( 'NONE', *, *, #51187, .F. ) ;
#35975 = ADVANCED_FACE ( 'NONE', ( #45067 ), #7531, .F. ) ;
#35976 = DIRECTION ( 'NONE',  ( 0.000000000000000000, -0.000000000000000000, -1.000000000000000000 ) ) ;
#35977 = VECTOR ( 'NONE', #13847, 1000.000000000000227 ) ;
#35978 = ORIENTED_EDGE ( 'NONE', *, *, #25470, .T. ) ;
#35979 = EDGE_CURVE ( 'NONE', #41338, #33009, #50957, .T. ) ;
#35980 = VERTEX_POINT ( 'NONE', #46151 ) ;
#35981 = VECTOR ( 'NONE', #16082, 1000.000000000000114 ) ;
#35982 = ORIENTED_EDGE ( 'NONE', *, *, #38842, .T. ) ;
#35983 = CARTESIAN_POINT ( 'NONE',  ( -10.94028622754223967, 0.000000000000000000, 11.14038480894692995 ) ) ;
#35984 = ORIENTED_EDGE ( 'NONE', *, *, #56190, .T. ) ;
#35985 = ORIENTED_EDGE ( 'NONE', *, *, #30452, .T. ) ;
#35986 = CARTESIAN_POINT ( 'NONE',  ( 2.072287782118878319, 0.000000000000000000, -2.950529333540147015 ) ) ;
#35987 = DIRECTION ( 'NONE',  ( -0.5449076811759708816, 0.6444004775717707689, 0.5364919789714475140 ) ) ;
#35988 = ORIENTED_EDGE ( 'NONE', *, *, #15972, .T. ) ;
#35989 = VECTOR ( 'NONE', #28802, 1000.000000000000000 ) ;
#35990 = VECTOR ( 'NONE', #42719, 1000.000000000000227 ) ;
#35991 = ORIENTED_EDGE ( 'NONE', *, *, #17215, .F. ) ;
#35992 = DIRECTION ( 'NONE',  ( 0.2426528472758541499, 0.7422098413412800966, 0.6246952433987894571 ) ) ;
#35993 = VERTEX_POINT ( 'NONE', #20867 ) ;
#35994 = ORIENTED_EDGE ( 'NONE', *, *, #51623, .F. ) ;
#35995 = AXIS2_PLACEMENT_3D ( 'NONE', #50172, #37383, #26052 ) ;
#35996 = AXIS2_PLACEMENT_3D ( 'NONE', #13445, #353, #38423 ) ;
#35997 = CARTESIAN_POINT ( 'NONE',  ( -16.26321790523673982, 0.000000000000000000, 4.324510933502299537 ) ) ;
#35998 = CARTESIAN_POINT ( 'NONE',  ( -14.04166784449981442, 0.4483081953215036219, 3.071331889294571571 ) ) ;
#35999 = DIRECTION ( 'NONE',  ( 0.007781995580012663651, -3.146120232559066537E-19, -0.9999697198139514409 ) ) ;
#36000 = CARTESIAN_POINT ( 'NONE',  ( -13.63673279712320507, -0.1191753592594197858, 12.22739664767016521 ) ) ;
#36001 = VERTEX_POINT ( 'NONE', #3287 ) ;
#36002 = DIRECTION ( 'NONE',  ( 0.007781995580012663651, -3.146120232559066537E-19, -0.9999697198139514409 ) ) ;
#36003 = ORIENTED_EDGE ( 'NONE', *, *, #41459, .F. ) ;
#36004 = DIRECTION ( 'NONE',  ( 0.7660212471507180654, -0.6427876096865404731, 0.005961354470445141482 ) ) ;
#36005 = VECTOR ( 'NONE', #37211, 999.9999999999998863 ) ;
#36006 = CARTESIAN_POINT ( 'NONE',  ( -26.13337879274045505, 0.000000000000000000, 6.833023547870798353 ) ) ;
#36007 = CARTESIAN_POINT ( 'NONE',  ( -68.54039869480983782, 0.1329787028216394551, 5.224814904089852163 ) ) ;
#36008 = CARTESIAN_POINT ( 'NONE',  ( -15.34987077819697987, 0.000000000000000000, 6.378285217289930031 ) ) ;
#36009 = CARTESIAN_POINT ( 'NONE',  ( -15.35849293871282839, 0.000000000000000000, 7.486214327063223095 ) ) ;
#36010 = CARTESIAN_POINT ( 'NONE',  ( -19.52717239714547048, 0.000000000000000000, 5.776438364157291616 ) ) ;
#36011 = ORIENTED_EDGE ( 'NONE', *, *, #30697, .T. ) ;
#36012 = CARTESIAN_POINT ( 'NONE',  ( -18.33038159707971815, 0.000000000000000000, 5.416419997087551508 ) ) ;
#36013 = ORIENTED_EDGE ( 'NONE', *, *, #39666, .F. ) ;
#36014 = EDGE_CURVE ( 'NONE', #7707, #23956, #28559, .T. ) ;
#36015 = CARTESIAN_POINT ( 'NONE',  ( -13.17065887352947762, -0.1191753592594197858, 12.04635770780929427 ) ) ;
#36016 = DIRECTION ( 'NONE',  ( 0.5364919789714477361, 0.6444004775717706579, 0.5449076811759711036 ) ) ;
#36018 = DIRECTION ( 'NONE',  ( 0.005002170337468016433, -0.7660444431189770143, -0.6427681459581293666 ) ) ;
#36017 = VECTOR ( 'NONE', #26863, 1000.000000000000227 ) ;
#36019 = FACE_OUTER_BOUND ( 'NONE', #34921, .T. ) ;
#36020 = EDGE_CURVE ( 'NONE', #45510, #54842, #37928, .T. ) ;
#36021 = LINE ( 'NONE', #28031, #11438 ) ;
#36022 = AXIS2_PLACEMENT_3D ( 'NONE', #13503, #13224, #48119 ) ;
#36023 = CARTESIAN_POINT ( 'NONE',  ( -68.44026216309750055, -1.000000000000000444, 5.059064008999124340 ) ) ;
#36024 = VERTEX_POINT ( 'NONE', #55236 ) ;
#36025 = CARTESIAN_POINT ( 'NONE',  ( -16.50344859827348287, 0.000000000000000000, 9.493290379994999029 ) ) ;
#36026 = LINE ( 'NONE', #23497, #36747 ) ;
#36027 = FACE_OUTER_BOUND ( 'NONE', #50547, .T. ) ;
#36028 = VECTOR ( 'NONE', #27441, 999.9999999999998863 ) ;
#36029 = CARTESIAN_POINT ( 'NONE',  ( -69.22881859397718074, 1.437012684761762582, -7.485193420789064689 ) ) ;
#36030 = FACE_OUTER_BOUND ( 'NONE', #32924, .T. ) ;
#36031 = DIRECTION ( 'NONE',  ( 0.6427681459581294776, -0.7660444431189769032, 0.005002170337467562802 ) ) ;
#36032 = VECTOR ( 'NONE', #17621, 1000.000000000000114 ) ;
#36033 = DIRECTION ( 'NONE',  ( 0.5364919789714477361, 0.6444004775717706579, 0.5449076811759711036 ) ) ;
#36034 = FACE_OUTER_BOUND ( 'NONE', #4550, .T. ) ;
#36035 = ORIENTED_EDGE ( 'NONE', *, *, #48832, .T. ) ;
#36036 = EDGE_CURVE ( 'NONE', #32655, #25448, #54138, .T. ) ;
#36037 = ORIENTED_EDGE ( 'NONE', *, *, #52219, .T. ) ;
#36038 = ORIENTED_EDGE ( 'NONE', *, *, #39364, .T. ) ;
#36039 = ORIENTED_EDGE ( 'NONE', *, *, #55319, .T. ) ;
#36040 = EDGE_CURVE ( 'NONE', #17655, #24033, #12066, .T. ) ;
#36041 = VERTEX_POINT ( 'NONE', #7842 ) ;
#36042 = CARTESIAN_POINT ( 'NONE',  ( -27.06552663992790997, 0.000000000000000000, 7.195101427592543786 ) ) ;
#36043 = DIRECTION ( 'NONE',  ( 0.7660212471507180654, -0.6427876096865404731, 0.005961354470445141482 ) ) ;
#36044 = VERTEX_POINT ( 'NONE', #11787 ) ;
#36045 = AXIS2_PLACEMENT_3D ( 'NONE', #34212, #39282, #8927 ) ;
#36046 = ORIENTED_EDGE ( 'NONE', *, *, #22966, .T. ) ;
#36047 = ADVANCED_FACE ( 'NONE', ( #7003 ), #41616, .F. ) ;
#36048 = ORIENTED_EDGE ( 'NONE', *, *, #31022, .F. ) ;
#36049 = AXIS2_PLACEMENT_3D ( 'NONE', #37890, #3517, #7485 ) ;
#36050 = CARTESIAN_POINT ( 'NONE',  ( -67.47405682104675861, -8.826835280158354280, -4.659789304343650684 ) ) ;
#36051 = LINE ( 'NONE', #10173, #6503 ) ;
#36052 = PLANE ( 'NONE',  #9584 ) ;
#36053 = ORIENTED_EDGE ( 'NONE', *, *, #47393, .F. ) ;
#36054 = PLANE ( 'NONE',  #152 ) ;
#36055 = EDGE_LOOP ( 'NONE', ( #12025, #50733, #28235, #14339 ) ) ;
#36056 = AXIS2_PLACEMENT_3D ( 'NONE', #36195, #39880, #53497 ) ;
#36057 = CARTESIAN_POINT ( 'NONE',  ( -13.53673582514181106, 0.000000000000000000, 12.22817484722816772 ) ) ;
#36058 = CARTESIAN_POINT ( 'NONE',  ( -13.95122827149485190, -0.03228989815065406305, 2.299421746729317206 ) ) ;
#36059 = CARTESIAN_POINT ( 'NONE',  ( -23.33849165029409889, 0.000000000000000000, 5.946783852668351855 ) ) ;
#36060 = DIRECTION ( 'NONE',  ( 0.5364919789714477361, 0.6444004775717706579, 0.5449076811759711036 ) ) ;
#36061 = FACE_OUTER_BOUND ( 'NONE', #23483, .T. ) ;
#36062 = CARTESIAN_POINT ( 'NONE',  ( -11.95923551588343337, 9.532254668142648768, 1.426999636052985965 ) ) ;
#36063 = FACE_OUTER_BOUND ( 'NONE', #51614, .T. ) ;
#36064 = ORIENTED_EDGE ( 'NONE', *, *, #23683, .T. ) ;
#36065 = PLANE ( 'NONE',  #41010 ) ;
#36066 = EDGE_CURVE ( 'NONE', #41646, #38799, #29106, .T. ) ;
#36067 = ORIENTED_EDGE ( 'NONE', *, *, #38526, .F. ) ;
#36068 = ADVANCED_FACE ( 'NONE', ( #15240 ), #29400, .F. ) ;
#36069 = DIRECTION ( 'NONE',  ( -0.005002170337468016433, -0.7660444431189770143, 0.6427681459581293666 ) ) ;
#36070 = CARTESIAN_POINT ( 'NONE',  ( -14.46888367232926420, 0.000000000000000000, 12.59025272694991315 ) ) ;
#36071 = DIRECTION ( 'NONE',  ( 1.000000000000000000, 0.000000000000000000, 0.000000000000000000 ) ) ;
#36072 = FACE_OUTER_BOUND ( 'NONE', #14244, .T. ) ;
#36073 = CARTESIAN_POINT ( 'NONE',  ( -17.93139508144814442, 0.000000000000000000, 13.85596890686001537 ) ) ;
#36074 = CARTESIAN_POINT ( 'NONE',  ( -11.20636620717317378, 0.000000000000000000, 11.32298014792380414 ) ) ;
#36075 = EDGE_CURVE ( 'NONE', #43669, #1875, #39391, .T. ) ;
#36076 = ADVANCED_FACE ( 'NONE', ( #45590 ), #6707, .F. ) ;
#36077 = DIRECTION ( 'NONE',  ( 0.007781995580012662783, 0.000000000000000000, -0.9999697198139514409 ) ) ;
#36078 = DIRECTION ( 'NONE',  ( 0.007781995580012663651, 0.000000000000000000, -0.9999697198139515519 ) ) ;
#36079 = PLANE ( 'NONE',  #596 ) ;
#36080 = VERTEX_POINT ( 'NONE', #11236 ) ;
#36081 = DIRECTION ( 'NONE',  ( 0.6427681459581294776, -0.7660444431189769032, 0.005002170337467562802 ) ) ;
#36082 = FACE_OUTER_BOUND ( 'NONE', #10242, .T. ) ;
#36083 = CARTESIAN_POINT ( 'NONE',  ( -70.10169143752739274, -0.9999999999999995559, 7.503902134509972122 ) ) ;
#36084 = DIRECTION ( 'NONE',  ( -0.7660212471507179544, -0.6427876096865405842, -0.005961354470445141482 ) ) ;
#36085 = CARTESIAN_POINT ( 'NONE',  ( -15.88130887279446490, 0.000000000000000000, 3.050160814894388839 ) ) ;
#36086 = CARTESIAN_POINT ( 'NONE',  ( -9.972665560950739305, 0.000000000000000000, 6.220125815427252292 ) ) ;
#36087 = LINE ( 'NONE', #19019, #1114 ) ;
#36088 = ADVANCED_FACE ( 'NONE', ( #42177 ), #41358, .F. ) ;
#36089 = EDGE_LOOP ( 'NONE', ( #20068, #25053, #37886, #1212 ) ) ;
#36090 = VECTOR ( 'NONE', #30501, 999.9999999999998863 ) ;
#36091 = ORIENTED_EDGE ( 'NONE', *, *, #56043, .T. ) ;
#36092 = CARTESIAN_POINT ( 'NONE',  ( -13.49419724433792034, 0.000000000000000000, 6.762058567619732230 ) ) ;
#36093 = FACE_OUTER_BOUND ( 'NONE', #42220, .T. ) ;
#36094 = VECTOR ( 'NONE', #22766, 1000.000000000000000 ) ;
#36095 = EDGE_LOOP ( 'NONE', ( #48087, #47557, #18455, #48612 ) ) ;
#36096 = CARTESIAN_POINT ( 'NONE',  ( 5.515141197255969630, -1.062154408800312755, -2.500037664106760094 ) ) ;
#36097 = ORIENTED_EDGE ( 'NONE', *, *, #48184, .F. ) ;
#36098 = DIRECTION ( 'NONE',  ( 0.007781995580012662783, 0.000000000000000000, -0.9999697198139514409 ) ) ;
#36099 = EDGE_LOOP ( 'NONE', ( #13885, #807, #7491, #7242 ) ) ;
#36100 = EDGE_LOOP ( 'NONE', ( #10258, #30650, #27642, #37085 ) ) ;
#36101 = EDGE_LOOP ( 'NONE', ( #14629, #12790, #19620, #43066 ) ) ;
#36102 = DIRECTION ( 'NONE',  ( 0.2426528472758541499, 0.7422098413412800966, 0.6246952433987894571 ) ) ;
#36103 = LINE ( 'NONE', #11056, #34105 ) ;
#36104 = FACE_OUTER_BOUND ( 'NONE', #28339, .T. ) ;
#36105 = DIRECTION ( 'NONE',  ( 0.6427681459581294776, -0.7660444431189769032, 0.005002170337467562802 ) ) ;
#36106 = VERTEX_POINT ( 'NONE', #25163 ) ;
#36107 = EDGE_CURVE ( 'NONE', #14388, #39202, #42468, .T. ) ;
#36108 = VERTEX_POINT ( 'NONE', #37091 ) ;
#36109 = DIRECTION ( 'NONE',  ( -0.6427681459581293666, -0.7660444431189770143, -0.005002170337467561935 ) ) ;
#36110 = ORIENTED_EDGE ( 'NONE', *, *, #9960, .T. ) ;
#36111 = DIRECTION ( 'NONE',  ( 0.7660212471507180654, -0.6427876096865404731, 0.005961354470445141482 ) ) ;
#36112 = VERTEX_POINT ( 'NONE', #20308 ) ;
#36113 = PLANE ( 'NONE',  #29676 ) ;
#36114 = PLANE ( 'NONE',  #37592 ) ;
#36115 = ADVANCED_FACE ( 'NONE', ( #50429 ), #11536, .F. ) ;
#36116 = ORIENTED_EDGE ( 'NONE', *, *, #37865, .T. ) ;
#36117 = LINE ( 'NONE', #1155, #43133 ) ;
#36118 = VERTEX_POINT ( 'NONE', #16071 ) ;
#36119 = ADVANCED_FACE ( 'NONE', ( #13210 ), #12383, .F. ) ;
#36120 = EDGE_CURVE ( 'NONE', #35683, #28956, #47561, .T. ) ;
#36121 = LINE ( 'NONE', #52573, #45398 ) ;
#36122 = EDGE_LOOP ( 'NONE', ( #45216, #31072, #50704, #6805 ) ) ;
#36123 = CARTESIAN_POINT ( 'NONE',  ( 2.072287782118878319, 0.000000000000000000, -2.950529333540147015 ) ) ;
#36124 = DIRECTION ( 'NONE',  ( 0.6427681459581294776, -0.7660444431189769032, 0.005002170337467562802 ) ) ;
#36125 = DIRECTION ( 'NONE',  ( 0.007781995580012663651, 0.000000000000000000, -0.9999697198139515519 ) ) ;
#36126 = ADVANCED_FACE ( 'NONE', ( #35090 ), #29962, .F. ) ;
#36127 = ORIENTED_EDGE ( 'NONE', *, *, #38328, .T. ) ;
#36128 = AXIS2_PLACEMENT_3D ( 'NONE', #25173, #46734, #8386 ) ;
#36129 = ADVANCED_FACE ( 'NONE', ( #21992 ), #4674, .F. ) ;
#36130 = PLANE ( 'NONE',  #31951 ) ;
#36131 = LINE ( 'NONE', #9989, #16759 ) ;
#36132 = DIRECTION ( 'NONE',  ( 0.9335804264972041855, -0.3583679495452943287, 0.000000000000000000 ) ) ;
#36133 = CARTESIAN_POINT ( 'NONE',  ( -15.32819600454399911, 0.000000000000000000, 3.593123350522788417 ) ) ;
#36134 = EDGE_CURVE ( 'NONE', #52431, #42836, #8677, .T. ) ;
#36135 = DIRECTION ( 'NONE',  ( -0.9999697198139514409, -0.000000000000000000, -0.007781995580013368816 ) ) ;
#36136 = CARTESIAN_POINT ( 'NONE',  ( -67.25395622669698525, -9.540674738394741894, 3.391838660562430441 ) ) ;
#36137 = EDGE_LOOP ( 'NONE', ( #10169, #18855, #30775 ) ) ;
#36138 = LINE ( 'NONE', #49467, #4428 ) ;
#36139 = LINE ( 'NONE', #27304, #6863 ) ;
#36140 = CARTESIAN_POINT ( 'NONE',  ( -67.39372447183772863, -4.296715151703168435E-12, 4.869406872007187914 ) ) ;
#36141 = ORIENTED_EDGE ( 'NONE', *, *, #14953, .T. ) ;
#36142 = CARTESIAN_POINT ( 'NONE',  ( -58.00000000000000711, -9.999999999999998224, -2.749999999999999556 ) ) ;
#36143 = CARTESIAN_POINT ( 'NONE',  ( -15.00597892355332696, -0.1191753592594181482, 9.047205394761215658 ) ) ;
#36144 = EDGE_LOOP ( 'NONE', ( #47231, #35123, #5004, #19956 ) ) ;
#36145 = EDGE_CURVE ( 'NONE', #9862, #31, #25417, .T. ) ;
#36146 = LINE ( 'NONE', #53707, #45783 ) ;
#36147 = CARTESIAN_POINT ( 'NONE',  ( -19.60912206198628027, -0.1191753592594197858, 4.398475361799976113 ) ) ;
#36148 = PLANE ( 'NONE',  #25593 ) ;
#36149 = EDGE_CURVE ( 'NONE', #19918, #47466, #409, .T. ) ;
#36150 = EDGE_LOOP ( 'NONE', ( #13637, #20601, #21758, #52152 ) ) ;
#36151 = VERTEX_POINT ( 'NONE', #52097 ) ;
#36152 = DIRECTION ( 'NONE',  ( -0.000000000000000000, -1.000000000000000000, -0.000000000000000000 ) ) ;
#36153 = CARTESIAN_POINT ( 'NONE',  ( -11.67244013076689946, 0.000000000000000000, 11.50401908778467863 ) ) ;
#36154 = FACE_OUTER_BOUND ( 'NONE', #36226, .T. ) ;
#36155 = FACE_OUTER_BOUND ( 'NONE', #47311, .T. ) ;
#36156 = ORIENTED_EDGE ( 'NONE', *, *, #12249, .T. ) ;
#36157 = LINE ( 'NONE', #53718, #12240 ) ;
#36158 = EDGE_LOOP ( 'NONE', ( #27936, #12592, #49515 ) ) ;
#36159 = FACE_OUTER_BOUND ( 'NONE', #50247, .T. ) ;
#36160 = DIRECTION ( 'NONE',  ( -0.5449076811759708816, 0.6444004775717707689, 0.5364919789714475140 ) ) ;
#36161 = EDGE_LOOP ( 'NONE', ( #21122, #14317, #24667, #5990 ) ) ;
#36162 = DIRECTION ( 'NONE',  ( 0.7660212471507180654, -0.6427876096865404731, 0.005961354470445141482 ) ) ;
#36163 = CARTESIAN_POINT ( 'NONE',  ( -25.20123094555300369, 0.000000000000000000, 6.470945668149052032 ) ) ;
#36164 = CARTESIAN_POINT ( 'NONE',  ( -24.27063949748155380, 0.000000000000000000, 6.308861732390097288 ) ) ;
#36165 = ORIENTED_EDGE ( 'NONE', *, *, #28455, .F. ) ;
#36166 = AXIS2_PLACEMENT_3D ( 'NONE', #31851, #48629, #48318 ) ;
#36167 = PLANE ( 'NONE',  #2951 ) ;
#36168 = ADVANCED_FACE ( 'NONE', ( #26527 ), #111, .F. ) ;
#36169 = ORIENTED_EDGE ( 'NONE', *, *, #46464, .F. ) ;
#36170 = ORIENTED_EDGE ( 'NONE', *, *, #8142, .F. ) ;
#36171 = ORIENTED_EDGE ( 'NONE', *, *, #38165, .T. ) ;
#36172 = DIRECTION ( 'NONE',  ( 0.005961354470445682716, -0.6427876096865404731, -0.7660212471507180654 ) ) ;
#36173 = VERTEX_POINT ( 'NONE', #4131 ) ;
#36174 = DIRECTION ( 'NONE',  ( 0.000000000000000000, -1.000000000000000000, 0.000000000000000000 ) ) ;
#36175 = ORIENTED_EDGE ( 'NONE', *, *, #2727, .T. ) ;
#36176 = DIRECTION ( 'NONE',  ( -0.5449076811759708816, 0.6444004775717707689, 0.5364919789714475140 ) ) ;
#36177 = DIRECTION ( 'NONE',  ( 0.000000000000000000, -1.000000000000000000, 0.000000000000000000 ) ) ;
#36178 = VERTEX_POINT ( 'NONE', #8958 ) ;
#36179 = DIRECTION ( 'NONE',  ( -0.6427681459581293666, -0.7660444431189770143, -0.005002170337467561935 ) ) ;
#36180 = ORIENTED_EDGE ( 'NONE', *, *, #33874, .F. ) ;
#36181 = EDGE_CURVE ( 'NONE', #40214, #33948, #17180, .T. ) ;
#36182 = DIRECTION ( 'NONE',  ( 0.007781995580012663651, -3.146120232559066537E-19, -0.9999697198139514409 ) ) ;
#36183 = DIRECTION ( 'NONE',  ( 0.000000000000000000, -0.000000000000000000, -1.000000000000000000 ) ) ;
#36184 = PLANE ( 'NONE',  #54068 ) ;
#36185 = LINE ( 'NONE', #14589, #8472 ) ;
#36186 = CARTESIAN_POINT ( 'NONE',  ( -13.65781925808015629, 0.000000000000000000, 2.086787245668887625 ) ) ;
#36187 = FACE_OUTER_BOUND ( 'NONE', #18972, .T. ) ;
#36188 = CARTESIAN_POINT ( 'NONE',  ( -14.26730381667732850, 1.257817950434004128, 4.487519983270500390 ) ) ;
#36189 = VERTEX_POINT ( 'NONE', #17753 ) ;
#36190 = ORIENTED_EDGE ( 'NONE', *, *, #13098, .T. ) ;
#36191 = EDGE_CURVE ( 'NONE', #56078, #36080, #26260, .T. ) ;
#36192 = CARTESIAN_POINT ( 'NONE',  ( -13.20943591692264718, 0.000000000000000000, 4.178950157467387960 ) ) ;
#36193 = DIRECTION ( 'NONE',  ( 0.9999697198139515519, 0.000000000000000000, 0.007781995580013368816 ) ) ;
#36194 = EDGE_CURVE ( 'NONE', #13117, #31769, #30807, .T. ) ;
#36195 = CARTESIAN_POINT ( 'NONE',  ( -18.19747506107908563, 0.000000000000000000, 14.03856424583689311 ) ) ;
#36196 = CARTESIAN_POINT ( 'NONE',  ( -16.06709938707323460, 0.000000000000000000, 13.13181314741652628 ) ) ;
#36197 = ORIENTED_EDGE ( 'NONE', *, *, #44878, .T. ) ;
#36198 = FACE_OUTER_BOUND ( 'NONE', #1007, .T. ) ;
#36199 = DIRECTION ( 'NONE',  ( 0.9999697198139515519, 0.000000000000000000, 0.007781995580013368816 ) ) ;
#36200 = ORIENTED_EDGE ( 'NONE', *, *, #31239, .T. ) ;
#36201 = CARTESIAN_POINT ( 'NONE',  ( -11.80115495887297428, 0.000000000000000000, 2.343249376482593682 ) ) ;
#36202 = CARTESIAN_POINT ( 'NONE',  ( -67.50810339439870233, 2.000000000000000000, 7.448312483692316022 ) ) ;
#36203 = EDGE_LOOP ( 'NONE', ( #21763, #31841, #3881 ) ) ;
#36204 = ADVANCED_FACE ( 'NONE', ( #55804 ), #34781, .F. ) ;
#36205 = MECHANICAL_DESIGN_GEOMETRIC_PRESENTATION_REPRESENTATION (  '', ( #56136 ), #11700 ) ;
#36206 = DIRECTION ( 'NONE',  ( -0.005961354470445682716, -0.6427876096865404731, 0.7660212471507180654 ) ) ;
#36207 = PLANE ( 'NONE',  #15165 ) ;
#36208 = LINE ( 'NONE', #14610, #16872 ) ;
#36209 = CARTESIAN_POINT ( 'NONE',  ( 2.072287782118878319, 0.000000000000000000, -2.950529333540147015 ) ) ;
#36210 = PLANE ( 'NONE',  #24694 ) ;
#36211 = ADVANCED_FACE ( 'NONE', ( #26006 ), #38187, .F. ) ;
#36212 = ORIENTED_EDGE ( 'NONE', *, *, #52340, .F. ) ;
#36213 = ORIENTED_EDGE ( 'NONE', *, *, #47121, .T. ) ;
#36214 = FACE_OUTER_BOUND ( 'NONE', #37758, .T. ) ;
#36215 = CARTESIAN_POINT ( 'NONE',  ( -14.66887761629205222, 0.000000000000000000, 12.58869632783390990 ) ) ;
#36216 = PLANE ( 'NONE',  #22465 ) ;
#36217 = DIRECTION ( 'NONE',  ( 0.9999697198139515519, 0.000000000000000000, 0.007781995580013368816 ) ) ;
#36218 = DIRECTION ( 'NONE',  ( 0.6246952433987893460, 0.7422098413412802076, -0.2426528472758539279 ) ) ;
#36219 = ORIENTED_EDGE ( 'NONE', *, *, #36617, .T. ) ;
#36220 = DIRECTION ( 'NONE',  ( -0.6427681459581293666, -0.7660444431189770143, -0.005002170337467561935 ) ) ;
#36221 = CARTESIAN_POINT ( 'NONE',  ( -16.81267852042393685, -0.1191753592594198830, 3.312241722634738927 ) ) ;
#36222 = DIRECTION ( 'NONE',  ( -0.9999697198139514409, -0.000000000000000000, -0.007781995580013368816 ) ) ;
#36223 = CARTESIAN_POINT ( 'NONE',  ( -20.51047058032500559, 20.81655013512439822, -4.320899323597838126 ) ) ;
#36224 = EDGE_LOOP ( 'NONE', ( #2750, #10795, #21564, #5429 ) ) ;
#36225 = CARTESIAN_POINT ( 'NONE',  ( -66.74449147233332269, -11.36157748060019301, 7.448312483692313357 ) ) ;
#36226 = EDGE_LOOP ( 'NONE', ( #39467, #1075, #28698, #37685 ) ) ;
#36227 = CARTESIAN_POINT ( 'NONE',  ( -16.94221901356702631, 0.000000000000000000, 6.165887138907109488 ) ) ;
#36228 = EDGE_CURVE ( 'NONE', #636, #9012, #33942, .T. ) ;
#36229 = CARTESIAN_POINT ( 'NONE',  ( -15.60102546347950536, 0.000000000000000000, 12.95077420755565356 ) ) ;
#36230 = ORIENTED_EDGE ( 'NONE', *, *, #8144, .T. ) ;
#36231 = CARTESIAN_POINT ( 'NONE',  ( -17.90602012812457389, 4.495856970884009485, 3.493796664491064963 ) ) ;
#36232 = ADVANCED_FACE ( 'NONE', ( #51261 ), #47008, .F. ) ;
#36233 = ORIENTED_EDGE ( 'NONE', *, *, #43077, .F. ) ;
#36234 = ORIENTED_EDGE ( 'NONE', *, *, #16891, .T. ) ;
#36235 = VERTEX_POINT ( 'NONE', #51550 ) ;
#36236 = CARTESIAN_POINT ( 'NONE',  ( -13.99411872359561926, -2.298917212465658721, 2.243764576467674576 ) ) ;
#36237 = EDGE_LOOP ( 'NONE', ( #46275, #34415, #25685, #48272 ) ) ;
#36238 = EDGE_CURVE ( 'NONE', #42908, #49004, #53249, .T. ) ;
#36239 = ORIENTED_EDGE ( 'NONE', *, *, #36947, .T. ) ;
#36240 = CARTESIAN_POINT ( 'NONE',  ( -19.60990026154428278, 0.000000000000000000, 4.498472333781370125 ) ) ;
#36241 = LINE ( 'NONE', #1846, #21319 ) ;
#36243 = ADVANCED_FACE ( 'NONE', ( #10344 ), #14042, .F. ) ;
#36242 = ORIENTED_EDGE ( 'NONE', *, *, #50063, .T. ) ;
#36244 = EDGE_CURVE ( 'NONE', #3565, #35683, #48697, .T. ) ;
#36245 = EDGE_CURVE ( 'NONE', #27257, #12509, #27106, .T. ) ;
#36246 = ORIENTED_EDGE ( 'NONE', *, *, #36857, .F. ) ;
#36247 = LINE ( 'NONE', #39380, #25845 ) ;
#36248 = ORIENTED_EDGE ( 'NONE', *, *, #19999, .T. ) ;
#36249 = ORIENTED_EDGE ( 'NONE', *, *, #42840, .T. ) ;
#36250 = CARTESIAN_POINT ( 'NONE',  ( -21.55158313111639146, -4.079838673713161334, 5.122519686159045627 ) ) ;
#36251 = CARTESIAN_POINT ( 'NONE',  ( 4.912750499197525045, -1.131233082521085231, 2.061810099490657411 ) ) ;
#36252 = DIRECTION ( 'NONE',  ( 0.5364919789714477361, 0.6444004775717706579, 0.5449076811759711036 ) ) ;
#36253 = DIRECTION ( 'NONE',  ( 0.005002170337468016433, -0.7660444431189770143, -0.6427681459581293666 ) ) ;
#36254 = ORIENTED_EDGE ( 'NONE', *, *, #10964, .T. ) ;
#36255 = DIRECTION ( 'NONE',  ( -0.5364919789714478471, 0.6444004775717705469, -0.5449076811759709926 ) ) ;
#36256 = ORIENTED_EDGE ( 'NONE', *, *, #7096, .T. ) ;
#36257 = ADVANCED_FACE ( 'NONE', ( #49229 ), #27956, .F. ) ;
#36258 = PLANE ( 'NONE',  #13918 ) ;
#36259 = EDGE_CURVE ( 'NONE', #26566, #25938, #10649, .T. ) ;
#36260 = CARTESIAN_POINT ( 'NONE',  ( -11.59291107943755605, 0.000000000000000000, 1.284706784507182231 ) ) ;
#36261 = CARTESIAN_POINT ( 'NONE',  ( -68.12990498669439887, 0.1329617757551050938, 4.288727116335238954 ) ) ;
#36262 = CARTESIAN_POINT ( 'NONE',  ( -17.74560456716937296, 0.000000000000000000, 3.774316574337878372 ) ) ;
#36263 = B_SPLINE_CURVE_WITH_KNOTS ( 'NONE', 3,
 ( #13704, #53196, #10293, #10599, #23078, #9453, #49180, #31321, #13994, #27914, #45218, #26777, #44101, #5216, #22528, #52883 ),
 .UNSPECIFIED., .F., .F.,
 ( 4, 2, 2, 2, 2, 2, 2, 4 ),
 ( 3.469446951953613804E-18, 0.001965516910292332883, 0.003931033820584662296, 0.007862067641169319387, 0.009827584551461647500, 0.01179310146175397735, 0.01375861837204630372, 0.01572413528233863184 ),
 .UNSPECIFIED. ) ;
#36264 = ADVANCED_FACE ( 'NONE', ( #36447 ), #18581, .F. ) ;
#36265 = DIRECTION ( 'NONE',  ( 0.000000000000000000, -1.000000000000000000, 0.000000000000000000 ) ) ;
#36266 = CARTESIAN_POINT ( 'NONE',  ( -13.13049853634656472, 5.467268677019015755, 1.607828781524239803 ) ) ;
#36267 = EDGE_LOOP ( 'NONE', ( #31557, #17197, #13402, #21003 ) ) ;
#36268 = LINE ( 'NONE', #44233, #17460 ) ;
#36269 = VERTEX_POINT ( 'NONE', #53761 ) ;
#36270 = EDGE_CURVE ( 'NONE', #51541, #55849, #5514, .T. ) ;
#36271 = LINE ( 'NONE', #11544, #17468 ) ;
#36272 = CARTESIAN_POINT ( 'NONE',  ( -16.48201256934722636, 0.000000000000000000, 6.738806697895671327 ) ) ;
#36273 = LINE ( 'NONE', #28029, #38110 ) ;
#36274 = DIRECTION ( 'NONE',  ( 0.6427681459581294776, -0.7660444431189769032, 0.005002170337467562802 ) ) ;
#36275 = CARTESIAN_POINT ( 'NONE',  ( -17.46532115785441519, 0.000000000000000000, 13.67492996699914265 ) ) ;
#36276 = CARTESIAN_POINT ( 'NONE',  ( -70.11839600776268355, -1.000000000000000666, -7.555920072494595630 ) ) ;
#36277 = ORIENTED_EDGE ( 'NONE', *, *, #16292, .F. ) ;
#36278 = CARTESIAN_POINT ( 'NONE',  ( -28.34606951297313060, 14.56061417452916729, 4.728537094605865576 ) ) ;
#36279 = LINE ( 'NONE', #1635, #33984 ) ;
#36280 = DIRECTION ( 'NONE',  ( 0.000000000000000000, -1.000000000000000000, 0.000000000000000000 ) ) ;
#36281 = CARTESIAN_POINT ( 'NONE',  ( -19.70178816256107979, -1.327505506330656670, 4.491810339156243614 ) ) ;
#36282 = DIRECTION ( 'NONE',  ( 0.7660212471507180654, -0.6427876096865404731, 0.005961354470445141482 ) ) ;
#36283 = CARTESIAN_POINT ( 'NONE',  ( -8.509919637592204822, -0.1191753592594197858, 10.23596830920056711 ) ) ;
#36284 = DIRECTION ( 'NONE',  ( -0.5449076811759708816, 0.6444004775717707689, 0.5364919789714475140 ) ) ;
#36285 = DIRECTION ( 'NONE',  ( -0.5449076811759708816, 0.6444004775717707689, 0.5364919789714475140 ) ) ;
#36286 = EDGE_LOOP ( 'NONE', ( #38425, #26948, #4319, #52563 ) ) ;
#36287 = VERTEX_POINT ( 'NONE', #14342 ) ;
#36288 = ORIENTED_EDGE ( 'NONE', *, *, #12704, .F. ) ;
#36289 = ORIENTED_EDGE ( 'NONE', *, *, #12763, .F. ) ;
#36290 = ORIENTED_EDGE ( 'NONE', *, *, #47098, .F. ) ;
#36291 = FACE_OUTER_BOUND ( 'NONE', #20898, .T. ) ;
#36292 = LINE ( 'NONE', #5927, #15824 ) ;
#36293 = EDGE_CURVE ( 'NONE', #21366, #24619, #45257, .T. ) ;
#36294 = EDGE_CURVE ( 'NONE', #29459, #51867, #44685, .T. ) ;
#36295 = ORIENTED_EDGE ( 'NONE', *, *, #8153, .T. ) ;
#36296 = VERTEX_POINT ( 'NONE', #52936 ) ;
#36297 = ORIENTED_EDGE ( 'NONE', *, *, #27384, .T. ) ;
#36298 = ADVANCED_FACE ( 'NONE', ( #14880 ), #27366, .F. ) ;
#36299 = AXIS2_PLACEMENT_3D ( 'NONE', #30629, #17841, #47931 ) ;
#36300 = DIRECTION ( 'NONE',  ( 0.6427681459581294776, -0.7660444431189769032, 0.005002170337467562802 ) ) ;
#36301 = CARTESIAN_POINT ( 'NONE',  ( -11.36525859708471486, 0.000000000000000000, 6.039962320828248465 ) ) ;
#36302 = DIRECTION ( 'NONE',  ( -0.005002170337468016433, -0.7660444431189770143, 0.6427681459581293666 ) ) ;
#36303 = ORIENTED_EDGE ( 'NONE', *, *, #43739, .F. ) ;
#36304 = DIRECTION ( 'NONE',  ( -0.05705673239519651330, 0.9983709377222391712, 2.351258244848514932E-16 ) ) ;
#36305 = ORIENTED_EDGE ( 'NONE', *, *, #3288, .T. ) ;
#36306 = CARTESIAN_POINT ( 'NONE',  ( -22.40478740399063895, 0.000000000000000000, 5.384712028983816623 ) ) ;
#36307 = CARTESIAN_POINT ( 'NONE',  ( -15.36843275361795591, 0.000000000000000000, 8.763459196131494267 ) ) ;
#36308 = ADVANCED_FACE ( 'NONE', ( #22294 ), #14596, .F. ) ;
#36309 = LINE ( 'NONE', #27225, #13707 ) ;
#36310 = PLANE ( 'NONE',  #656 ) ;
#36311 = CARTESIAN_POINT ( 'NONE',  ( -13.71393590006033492, 0.6102101463440037232, 3.209738356201059073 ) ) ;
#36312 = PLANE ( 'NONE',  #54676 ) ;
#36313 = LINE ( 'NONE', #6491, #41218 ) ;
#36314 = ADVANCED_FACE ( 'NONE', ( #39626 ), #705, .F. ) ;
#36315 = EDGE_LOOP ( 'NONE', ( #8935, #32281, #11516, #43797 ) ) ;
#36316 = CARTESIAN_POINT ( 'NONE',  ( -21.47341775636118655, -0.1191753592594197858, 5.122631121243466090 ) ) ;
#36317 = ORIENTED_EDGE ( 'NONE', *, *, #48328, .T. ) ;
#36318 = EDGE_CURVE ( 'NONE', #55206, #16632, #31068, .T. ) ;
#36319 = CARTESIAN_POINT ( 'NONE',  ( -8.609916609573598834, 0.000000000000000000, 10.23519010964256637 ) ) ;
#36320 = CARTESIAN_POINT ( 'NONE',  ( -18.39746900504187010, 0.000000000000000000, 14.03700784672088808 ) ) ;
#36321 = LINE ( 'NONE', #33656, #17701 ) ;
#36322 = CARTESIAN_POINT ( 'NONE',  ( -10.00813838035478298, 0.000000000000000000, 10.77830692922518452 ) ) ;
#36323 = DIRECTION ( 'NONE',  ( -0.5364919789714478471, 0.6444004775717705469, -0.5449076811759709926 ) ) ;
#36324 = EDGE_CURVE ( 'NONE', #5802, #39181, #35924, .T. ) ;
#36325 = DIRECTION ( 'NONE',  ( -0.005961354470445682716, -0.6427876096865404731, 0.7660212471507180654 ) ) ;
#36326 = DIRECTION ( 'NONE',  ( 0.6427681459581294776, -0.7660444431189769032, 0.005002170337467562802 ) ) ;
#36327 = DIRECTION ( 'NONE',  ( 0.000000000000000000, -1.000000000000000000, 0.000000000000000000 ) ) ;
#36328 = EDGE_CURVE ( 'NONE', #5918, #42224, #31913, .T. ) ;
#36329 = FACE_OUTER_BOUND ( 'NONE', #22732, .T. ) ;
#36330 = EDGE_LOOP ( 'NONE', ( #55357, #43158, #17275, #1706 ) ) ;
#36331 = CARTESIAN_POINT ( 'NONE',  ( -17.26532721389163072, 0.000000000000000000, 13.67648636611514590 ) ) ;
#36332 = LINE ( 'NONE', #10514, #11320 ) ;
#36334 = EDGE_CURVE ( 'NONE', #3029, #44205, #16018, .T. ) ;
#36333 = DIRECTION ( 'NONE',  ( -0.6427681459581293666, -0.7660444431189770143, -0.005002170337467561935 ) ) ;
#36335 = FACE_OUTER_BOUND ( 'NONE', #23967, .T. ) ;
#36336 = ADVANCED_FACE ( 'NONE', ( #33582 ), #33330, .F. ) ;
#36337 = DIRECTION ( 'NONE',  ( -0.5364919789714478471, 0.6444004775717705469, -0.5449076811759709926 ) ) ;
#36338 = FACE_OUTER_BOUND ( 'NONE', #38600, .T. ) ;
#36339 = DIRECTION ( 'NONE',  ( 0.9999697198139515519, 0.000000000000000000, 0.007781995580013368816 ) ) ;
#36340 = EDGE_LOOP ( 'NONE', ( #14918, #14714, #9297, #39786 ) ) ;
#36341 = VECTOR ( 'NONE', #23067, 999.9999999999998863 ) ;
#36342 = ORIENTED_EDGE ( 'NONE', *, *, #19148, .T. ) ;
#36343 = DIRECTION ( 'NONE',  ( 0.5449076811759707706, 0.6444004775717708799, -0.5364919789714476250 ) ) ;
#36344 = CARTESIAN_POINT ( 'NONE',  ( -13.84758239767214860, 4.657758921906512306, 1.912196104970483868 ) ) ;
#36345 = ORIENTED_EDGE ( 'NONE', *, *, #13030, .F. ) ;
#36346 = LINE ( 'NONE', #31552, #16784 ) ;
#36347 = ORIENTED_EDGE ( 'NONE', *, *, #46434, .T. ) ;
#36348 = DIRECTION ( 'NONE',  ( -0.9999697198139514409, -0.000000000000000000, -0.007781995580013368816 ) ) ;
#36349 = ORIENTED_EDGE ( 'NONE', *, *, #19934, .T. ) ;
#36350 = ORIENTED_EDGE ( 'NONE', *, *, #41686, .T. ) ;
#36351 = ORIENTED_EDGE ( 'NONE', *, *, #12255, .T. ) ;
#36352 = DIRECTION ( 'NONE',  ( 0.9999697198139515519, 0.000000000000000000, 0.007781995580013368816 ) ) ;
#36353 = FACE_OUTER_BOUND ( 'NONE', #8207, .T. ) ;
#36354 = CARTESIAN_POINT ( 'NONE',  ( -16.81190032086591302, 0.000000000000000000, 3.212244750653343583 ) ) ;
#36355 = EDGE_CURVE ( 'NONE', #10472, #14361, #2069, .T. ) ;
#36356 = AXIS2_PLACEMENT_3D ( 'NONE', #24054, #15799, #19216 ) ;
#36357 = ORIENTED_EDGE ( 'NONE', *, *, #11087, .F. ) ;
#36358 = ORIENTED_EDGE ( 'NONE', *, *, #36647, .F. ) ;
#36359 = EDGE_CURVE ( 'NONE', #7820, #13266, #24244, .T. ) ;
#36360 = EDGE_CURVE ( 'NONE', #41032, #40408, #45513, .T. ) ;
#36361 = FACE_OUTER_BOUND ( 'NONE', #20448, .T. ) ;
#36362 = ORIENTED_EDGE ( 'NONE', *, *, #42059, .F. ) ;
#36363 = CARTESIAN_POINT ( 'NONE',  ( -23.33693525117809386, 0.000000000000000000, 5.746789908705562944 ) ) ;
#36364 = ORIENTED_EDGE ( 'NONE', *, *, #3677, .F. ) ;
#36365 = FACE_OUTER_BOUND ( 'NONE', #16107, .T. ) ;
#36366 = CARTESIAN_POINT ( 'NONE',  ( -10.22581229980790418, 0.000000000000000000, 4.740827489744188661 ) ) ;
#36367 = ORIENTED_EDGE ( 'NONE', *, *, #8804, .T. ) ;
#36368 = VECTOR ( 'NONE', #13669, 1000.000000000000114 ) ;
#36369 = CARTESIAN_POINT ( 'NONE',  ( -13.95883414117900934, 0.000000000000000000, 6.758442655851721881 ) ) ;
#36370 = ADVANCED_FACE ( 'NONE', ( #54891 ), #41812, .F. ) ;
#36371 = VECTOR ( 'NONE', #6793, 1000.000000000000227 ) ;
#36372 = LINE ( 'NONE', #1725, #49931 ) ;
#36373 = ORIENTED_EDGE ( 'NONE', *, *, #15269, .F. ) ;
#36374 = DIRECTION ( 'NONE',  ( -0.005002170337468016433, -0.7660444431189770143, 0.6427681459581293666 ) ) ;
#36375 = FACE_OUTER_BOUND ( 'NONE', #51568, .T. ) ;
#36376 = CARTESIAN_POINT ( 'NONE',  ( -15.82666044788779303, 3.686347215771511365, 2.711930348772070509 ) ) ;
#36377 = EDGE_LOOP ( 'NONE', ( #27651, #33860, #56183, #15331 ) ) ;
#36378 = DIRECTION ( 'NONE',  ( 0.5364919789714477361, 0.6444004775717706579, 0.5449076811759711036 ) ) ;
#36379 = CARTESIAN_POINT ( 'NONE',  ( -12.56049299803446750, 0.000000000000000000, 6.199986743935199662 ) ) ;
#36380 = PLANE ( 'NONE',  #42131 ) ;
#36381 = CARTESIAN_POINT ( 'NONE',  ( -14.86511550681891691, 0.000000000000000000, 3.796733206253588122 ) ) ;
#36382 = EDGE_CURVE ( 'NONE', #42498, #21366, #6632, .T. ) ;
#36383 = CARTESIAN_POINT ( 'NONE',  ( -12.52505892662501097, 0.000000000000000000, 1.646784664228929218 ) ) ;
#36384 = DIRECTION ( 'NONE',  ( -0.5449076811759708816, 0.6444004775717707689, 0.5364919789714475140 ) ) ;
#36385 = CARTESIAN_POINT ( 'NONE',  ( -68.36693371783928797, -11.54762975344078768, 6.564485215144721941 ) ) ;
#36386 = EDGE_LOOP ( 'NONE', ( #50557, #14437, #15632, #53219 ) ) ;
#36388 = EDGE_CURVE ( 'NONE', #22744, #2049, #19702, .T. ) ;
#36387 = PLANE ( 'NONE',  #22580 ) ;
#36389 = DIRECTION ( 'NONE',  ( -0.5364919789714478471, 0.6444004775717705469, -0.5449076811759709926 ) ) ;
#36390 = CARTESIAN_POINT ( 'NONE',  ( -67.85140231345076245, -4.690475086145005873E-12, -5.859509639698581296 ) ) ;
#36391 = ORIENTED_EDGE ( 'NONE', *, *, #43699, .T. ) ;
#36392 = CARTESIAN_POINT ( 'NONE',  ( -18.39746900504187010, 0.000000000000000000, 14.03700784672088808 ) ) ;
#36393 = LINE ( 'NONE', #49743, #3657 ) ;
#36394 = VECTOR ( 'NONE', #7338, 999.9999999999998863 ) ;
#36395 = VECTOR ( 'NONE', #16679, 1000.000000000000227 ) ;
#36396 = EDGE_CURVE ( 'NONE', #55993, #37342, #37869, .T. ) ;
#36397 = LINE ( 'NONE', #24191, #54867 ) ;
#36398 = PLANE ( 'NONE',  #6955 ) ;
#36399 = FACE_OUTER_BOUND ( 'NONE', #40963, .T. ) ;
#36400 = VERTEX_POINT ( 'NONE', #15693 ) ;
#36401 = ORIENTED_EDGE ( 'NONE', *, *, #32908, .T. ) ;
#36402 = FACE_OUTER_BOUND ( 'NONE', #16044, .T. ) ;
#36403 = DIRECTION ( 'NONE',  ( -0.9999697198139514409, -0.000000000000000000, -0.007781995580013368816 ) ) ;
#36404 = ADVANCED_FACE ( 'NONE', ( #7460 ), #23947, .F. ) ;
#36405 = LINE ( 'NONE', #15133, #40197 ) ;
#36406 = ORIENTED_EDGE ( 'NONE', *, *, #33852, .T. ) ;
#36407 = CARTESIAN_POINT ( 'NONE',  ( -69.51265309394176484, -9.414302016845754295, -7.502502568033363239 ) ) ;
#36408 = VERTEX_POINT ( 'NONE', #54061 ) ;
#36409 = PLANE ( 'NONE',  #27431 ) ;
#36410 = ADVANCED_FACE ( 'NONE', ( #15177 ), #24783, .F. ) ;
#36411 = AXIS2_PLACEMENT_3D ( 'NONE', #11652, #36656, #11365 ) ;
#36412 = VERTEX_POINT ( 'NONE', #11992 ) ;
#36413 = CARTESIAN_POINT ( 'NONE',  ( -10.74029228357944987, 0.000000000000000000, 11.14194120806293320 ) ) ;
#36414 = ADVANCED_FACE ( 'NONE', ( #37567 ), #45805, .F. ) ;
#36415 = LINE ( 'NONE', #10612, #1461 ) ;
#36416 = LINE ( 'NONE', #49496, #16690 ) ;
#36417 = ORIENTED_EDGE ( 'NONE', *, *, #331, .T. ) ;
#36418 = FACE_OUTER_BOUND ( 'NONE', #3221, .T. ) ;
#36419 = EDGE_CURVE ( 'NONE', #41178, #4939, #16263, .T. ) ;
#36420 = ORIENTED_EDGE ( 'NONE', *, *, #929, .F. ) ;
#36421 = EDGE_CURVE ( 'NONE', #48670, #55547, #50350, .T. ) ;
#36422 = EDGE_LOOP ( 'NONE', ( #46240, #40265, #47766, #18853 ) ) ;
#36423 = ORIENTED_EDGE ( 'NONE', *, *, #51024, .T. ) ;
#36424 = FACE_OUTER_BOUND ( 'NONE', #54682, .T. ) ;
#36425 = ORIENTED_EDGE ( 'NONE', *, *, #33000, .F. ) ;
#36426 = CARTESIAN_POINT ( 'NONE',  ( -69.66297551618575312, -8.676591480033549075, 7.503902134509970345 ) ) ;
#36427 = EDGE_LOOP ( 'NONE', ( #26065, #34410, #17497, #5982 ) ) ;
#36428 = CARTESIAN_POINT ( 'NONE',  ( -1.299719944060198529, -6.815497196261854462, 3.723228940611872595 ) ) ;
#36429 = FACE_OUTER_BOUND ( 'NONE', #41225, .T. ) ;
#36430 = EDGE_CURVE ( 'NONE', #30223, #40790, #11462, .T. ) ;
#36431 = VECTOR ( 'NONE', #24270, 999.9999999999998863 ) ;
#36432 = AXIS2_PLACEMENT_3D ( 'NONE', #23656, #27951, #13549 ) ;
#36433 = ORIENTED_EDGE ( 'NONE', *, *, #6366, .F. ) ;
#36434 = DIRECTION ( 'NONE',  ( 0.6427681459581294776, -0.7660444431189769032, 0.005002170337467562802 ) ) ;
#36435 = ORIENTED_EDGE ( 'NONE', *, *, #30342, .F. ) ;
#36436 = EDGE_CURVE ( 'NONE', #42084, #50596, #2902, .T. ) ;
#36437 = PLANE ( 'NONE',  #18327 ) ;
#36438 = CARTESIAN_POINT ( 'NONE',  ( -12.23851102634202448, -0.1191753592594197858, 11.68427982808754884 ) ) ;
#36439 = VECTOR ( 'NONE', #27666, 999.9999999999998863 ) ;
#36440 = LINE ( 'NONE', #35609, #47706 ) ;
#36441 = LINE ( 'NONE', #53753, #30244 ) ;
#36442 = DIRECTION ( 'NONE',  ( 0.7660212471507180654, -0.6427876096865404731, 0.005961354470445141482 ) ) ;
#36443 = DIRECTION ( 'NONE',  ( -0.005961354470445682716, -0.6427876096865404731, 0.7660212471507180654 ) ) ;
#36444 = ORIENTED_EDGE ( 'NONE', *, *, #33280, .F. ) ;
#36445 = ORIENTED_EDGE ( 'NONE', *, *, #32733, .F. ) ;
#36446 = CARTESIAN_POINT ( 'NONE',  ( -10.22293824630262193, 0.000000000000000000, 4.371517786486424306 ) ) ;
#36447 = FACE_OUTER_BOUND ( 'NONE', #11961, .T. ) ;
#36448 = AXIS2_PLACEMENT_3D ( 'NONE', #5036, #34851, #52165 ) ;
#36449 = AXIS2_PLACEMENT_3D ( 'NONE', #47325, #42522, #9489 ) ;
#36450 = DIRECTION ( 'NONE',  ( -0.9999697198139514409, -0.000000000000000000, -0.007781995580013368816 ) ) ;
#36451 = CARTESIAN_POINT ( 'NONE',  ( 0.000000000000000000, -1.000000000000000000, 0.000000000000000000 ) ) ;
#36452 = ORIENTED_EDGE ( 'NONE', *, *, #7197, .T. ) ;
#36453 = DIRECTION ( 'NONE',  ( -0.6427681459581293666, -0.7660444431189770143, -0.005002170337467561935 ) ) ;
#36454 = DIRECTION ( 'NONE',  ( -0.3583679495452941621, -0.9335804264972042965, 0.000000000000000000 ) ) ;
#36455 = ORIENTED_EDGE ( 'NONE', *, *, #46821, .F. ) ;
#36456 = CARTESIAN_POINT ( 'NONE',  ( -26.13415699229845757, -0.1191753592594197858, 6.933020519852192365 ) ) ;
#36457 = FACE_OUTER_BOUND ( 'NONE', #2656, .T. ) ;
#36458 = ORIENTED_EDGE ( 'NONE', *, *, #53716, .T. ) ;
#36459 = CARTESIAN_POINT ( 'NONE',  ( -67.32595136268157887, -0.9999999999999974465, 0.5932824550257459473 ) ) ;
#36460 = PLANE ( 'NONE',  #26957 ) ;
#36461 = EDGE_CURVE ( 'NONE', #5753, #20039, #25092, .T. ) ;
#36462 = FACE_OUTER_BOUND ( 'NONE', #53009, .T. ) ;
#36463 = CARTESIAN_POINT ( 'NONE',  ( -19.06540955380966551, 0.000000000000000000, 6.149363979183064544 ) ) ;
#36464 = FACE_OUTER_BOUND ( 'NONE', #15747, .T. ) ;
#36465 = ORIENTED_EDGE ( 'NONE', *, *, #34897, .T. ) ;
#36466 = ORIENTED_EDGE ( 'NONE', *, *, #4188, .T. ) ;
#36467 = DIRECTION ( 'NONE',  ( 0.000000000000000000, -0.000000000000000000, -1.000000000000000000 ) ) ;
#36468 = CARTESIAN_POINT ( 'NONE',  ( -10.24018256733431897, 0.000000000000000000, 6.587376006033009546 ) ) ;
#36469 = VECTOR ( 'NONE', #946, 1000.000000000000114 ) ;
#36470 = DIRECTION ( 'NONE',  ( 0.007781995580012663651, 0.000000000000000000, -0.9999697198139515519 ) ) ;
#36471 = EDGE_CURVE ( 'NONE', #6270, #49012, #38973, .T. ) ;
#36472 = AXIS2_PLACEMENT_3D ( 'NONE', #35048, #9172, #30505 ) ;
#36473 = AXIS2_PLACEMENT_3D ( 'NONE', #7977, #21002, #50819 ) ;
#36474 = CARTESIAN_POINT ( 'NONE',  ( -14.60753831534046476, 0.000000000000000000, 4.706727884716099375 ) ) ;
#36475 = LINE ( 'NONE', #41580, #24930 ) ;
#36477 = EDGE_CURVE ( 'NONE', #55458, #8286, #8600, .T. ) ;
#36476 = ORIENTED_EDGE ( 'NONE', *, *, #9773, .F. ) ;
#36478 = PLANE ( 'NONE',  #38324 ) ;
#36479 = EDGE_CURVE ( 'NONE', #50963, #52679, #17376, .T. ) ;
#36480 = CARTESIAN_POINT ( 'NONE',  ( -18.19747506107908563, 0.000000000000000000, 14.03856424583689311 ) ) ;
#36481 = VECTOR ( 'NONE', #17270, 1000.000000000000114 ) ;
#36482 = CARTESIAN_POINT ( 'NONE',  ( -20.63663870328428374, 20.74370693537071020, -4.329125112780540796 ) ) ;
#36483 = AXIS2_PLACEMENT_3D ( 'NONE', #6855, #50271, #20464 ) ;
#36484 = VERTEX_POINT ( 'NONE', #3495 ) ;
#36485 = CARTESIAN_POINT ( 'NONE',  ( -67.30928982028858343, -11.38498548360074025, 7.460396425438591272 ) ) ;
#36486 = ORIENTED_EDGE ( 'NONE', *, *, #45911, .F. ) ;
#36487 = CARTESIAN_POINT ( 'NONE',  ( -13.07066190154808361, 0.000000000000000000, 12.04713590736729678 ) ) ;
#36488 = LINE ( 'NONE', #19447, #3956 ) ;
#36489 = VERTEX_POINT ( 'NONE', #8304 ) ;
#36490 = CARTESIAN_POINT ( 'NONE',  ( -17.88011496776504572, 0.000000000000000000, 7.266584425144382742 ) ) ;
#36491 = ADVANCED_FACE ( 'NONE', ( #34430 ), #43258, .F. ) ;
#36492 = VECTOR ( 'NONE', #36255, 1000.000000000000000 ) ;
#36493 = ORIENTED_EDGE ( 'NONE', *, *, #33426, .T. ) ;
#36494 = ADVANCED_FACE ( 'NONE', ( #55729 ), #12582, .F. ) ;
#36495 = ORIENTED_EDGE ( 'NONE', *, *, #40950, .T. ) ;
#36496 = ORIENTED_EDGE ( 'NONE', *, *, #17978, .T. ) ;
#36497 = FACE_OUTER_BOUND ( 'NONE', #10398, .T. ) ;
#36498 = ORIENTED_EDGE ( 'NONE', *, *, #53773, .F. ) ;
#36499 = ORIENTED_EDGE ( 'NONE', *, *, #10270, .T. ) ;
#36500 = DIRECTION ( 'NONE',  ( 0.9999697198139515519, 0.000000000000000000, 0.007781995580013368816 ) ) ;
#36501 = FACE_OUTER_BOUND ( 'NONE', #34229, .T. ) ;
#36502 = ORIENTED_EDGE ( 'NONE', *, *, #28126, .F. ) ;
#36503 = EDGE_CURVE ( 'NONE', #48024, #44358, #56027, .T. ) ;
#36504 = ORIENTED_EDGE ( 'NONE', *, *, #25618, .F. ) ;
#36505 = CARTESIAN_POINT ( 'NONE',  ( -26.83479864408084126, 17.16519762507144975, 4.645878820492973738 ) ) ;
#36506 = ORIENTED_EDGE ( 'NONE', *, *, #8064, .F. ) ;
#36507 = VECTOR ( 'NONE', #31792, 1000.000000000000227 ) ;
#36508 = ORIENTED_EDGE ( 'NONE', *, *, #9494, .F. ) ;
#36509 = EDGE_CURVE ( 'NONE', #48860, #55206, #29899, .T. ) ;
#36510 = DIRECTION ( 'NONE',  ( 0.6427681459581294776, -0.7660444431189769032, 0.005002170337467562802 ) ) ;
#36511 = CARTESIAN_POINT ( 'NONE',  ( 0.1285714285714289751, 0.000000000000000000, -5.998622290806042479 ) ) ;
#36512 = CARTESIAN_POINT ( 'NONE',  ( -16.49195238425235743, 0.000000000000000000, 8.016051566963941610 ) ) ;
#36513 = LINE ( 'NONE', #14659, #52298 ) ;
#36514 = VECTOR ( 'NONE', #37057, 1000.000000000000227 ) ;
#36515 = EDGE_LOOP ( 'NONE', ( #11136, #16678, #13419, #1981 ) ) ;
#36516 = LINE ( 'NONE', #23200, #30171 ) ;
#36517 = ORIENTED_EDGE ( 'NONE', *, *, #47821, .T. ) ;
#36518 = VECTOR ( 'NONE', #24055, 1000.000000000000227 ) ;
#36519 = AXIS2_PLACEMENT_3D ( 'NONE', #12147, #41950, #29482 ) ;
#36520 = LINE ( 'NONE', #35693, #45646 ) ;
#36521 = CARTESIAN_POINT ( 'NONE',  ( -18.05255645404804454, -2.137015261443159009, 3.825365135988253673 ) ) ;
#36522 = AXIS2_PLACEMENT_3D ( 'NONE', #18543, #1207, #31030 ) ;
#36523 = VECTOR ( 'NONE', #49916, 1000.000000000000114 ) ;
#36524 = DIRECTION ( 'NONE',  ( -0.9321478471874540261, 0.000000000000000000, 0.3620778797217457656 ) ) ;
#36525 = CARTESIAN_POINT ( 'NONE',  ( -17.73140113748535285, 0.000000000000000000, 13.85752530597602039 ) ) ;
#36526 = LINE ( 'NONE', #31724, #335 ) ;
#36527 = DIRECTION ( 'NONE',  ( 0.6427681459581294776, -0.7660444431189769032, 0.005002170337467562802 ) ) ;
#36528 = EDGE_LOOP ( 'NONE', ( #7633, #26050, #30308, #17349 ) ) ;
#36529 = LINE ( 'NONE', #22915, #24703 ) ;
#36530 = VERTEX_POINT ( 'NONE', #12849 ) ;
#36531 = CARTESIAN_POINT ( 'NONE',  ( -22.57598249675604052, 4.981562823951511731, 13.82619267738939328 ) ) ;
#36532 = LINE ( 'NONE', #18953, #41419 ) ;
#36533 = PLANE ( 'NONE',  #41708 ) ;
#36534 = VECTOR ( 'NONE', #52247, 1000.000000000000227 ) ;
#36535 = ADVANCED_FACE ( 'NONE', ( #3757 ), #47488, .F. ) ;
#36536 = CARTESIAN_POINT ( 'NONE',  ( -18.86354292863559579, 0.000000000000000000, 14.21804678658176080 ) ) ;
#36537 = VECTOR ( 'NONE', #33914, 1000.000000000000114 ) ;
#36538 = CARTESIAN_POINT ( 'NONE',  ( -13.27065584551087163, 0.000000000000000000, 12.04557950825129176 ) ) ;
#36539 = ADVANCED_FACE ( 'NONE', ( #25931 ), #4355, .F. ) ;
#36540 = ORIENTED_EDGE ( 'NONE', *, *, #31276, .F. ) ;
#36541 = CARTESIAN_POINT ( 'NONE',  ( -9.959851692540329537, 0.000000000000000000, 4.573571243101220318 ) ) ;
#36542 = DIRECTION ( 'NONE',  ( -0.5364919789714478471, 0.6444004775717705469, -0.5449076811759709926 ) ) ;
#36543 = DIRECTION ( 'NONE',  ( 0.5364919789714477361, 0.6444004775717706579, 0.5449076811759711036 ) ) ;
#36544 = EDGE_CURVE ( 'NONE', #2632, #10808, #13429, .T. ) ;
#36545 = VECTOR ( 'NONE', #5316, 999.9999999999998863 ) ;
#36546 = EDGE_CURVE ( 'NONE', #23289, #17566, #26201, .T. ) ;
#36547 = EDGE_CURVE ( 'NONE', #27982, #7513, #25622, .T. ) ;
#36548 = CARTESIAN_POINT ( 'NONE',  ( -69.79279777665210815, 0.8065827901120606880, -7.497281464624094838 ) ) ;
#36549 = LINE ( 'NONE', #32575, #21239 ) ;
#36550 = CIRCLE ( 'NONE', #45617, 2.125000000000000000 ) ;
#36551 = CARTESIAN_POINT ( 'NONE',  ( -15.44908955062037492, -0.1191753592594185784, 6.277510045750531731 ) ) ;
#36552 = CARTESIAN_POINT ( 'NONE',  ( -10.87607287308537174, 0.000000000000000000, 2.889106662571353290 ) ) ;
#36553 = ADVANCED_FACE ( 'NONE', ( #55437 ), #16537, .F. ) ;
#36554 = LINE ( 'NONE', #19512, #23309 ) ;
#36555 = VECTOR ( 'NONE', #47447, 1000.000000000000227 ) ;
#36556 = LINE ( 'NONE', #6461, #24671 ) ;
#36557 = ORIENTED_EDGE ( 'NONE', *, *, #9239, .T. ) ;
#36558 = VECTOR ( 'NONE', #29178, 1000.000000000000114 ) ;
#36559 = VECTOR ( 'NONE', #49390, 1000.000000000000227 ) ;
#36560 = ORIENTED_EDGE ( 'NONE', *, *, #39578, .F. ) ;
#36561 = EDGE_CURVE ( 'NONE', #41657, #21645, #29639, .T. ) ;
#36562 = EDGE_CURVE ( 'NONE', #37474, #27104, #9888, .T. ) ;
#36563 = AXIS2_PLACEMENT_3D ( 'NONE', #20129, #37462, #33231 ) ;
#36564 = ORIENTED_EDGE ( 'NONE', *, *, #55992, .T. ) ;
#36565 = ORIENTED_EDGE ( 'NONE', *, *, #51811, .T. ) ;
#36566 = CIRCLE ( 'NONE', #28406, 2.125000000000000000 ) ;
#36567 = ORIENTED_EDGE ( 'NONE', *, *, #35136, .F. ) ;
#36568 = EDGE_CURVE ( 'NONE', #34678, #44201, #36131, .T. ) ;
#36569 = VERTEX_POINT ( 'NONE', #53432 ) ;
#36570 = DIRECTION ( 'NONE',  ( -0.8531650599175527594, 0.4028455766673922356, 0.3313982828793700652 ) ) ;
#36571 = CARTESIAN_POINT ( 'NONE',  ( -23.33849165029409889, 0.000000000000000000, 5.946783852668351855 ) ) ;
#36572 = EDGE_CURVE ( 'NONE', #31757, #10233, #53693, .T. ) ;
#36573 = ORIENTED_EDGE ( 'NONE', *, *, #39111, .F. ) ;
#36574 = ORIENTED_EDGE ( 'NONE', *, *, #40529, .F. ) ;
#36575 = VECTOR ( 'NONE', #51404, 1000.000000000000114 ) ;
#36576 = ORIENTED_EDGE ( 'NONE', *, *, #29222, .T. ) ;
#36577 = VECTOR ( 'NONE', #42230, 999.9999999999998863 ) ;
#36578 = DIRECTION ( 'NONE',  ( 0.5449076811759707706, 0.6444004775717708799, -0.5364919789714476250 ) ) ;
#36579 = FACE_OUTER_BOUND ( 'NONE', #7442, .T. ) ;
#36580 = DIRECTION ( 'NONE',  ( 0.6427681459581294776, -0.7660444431189769032, 0.005002170337467562802 ) ) ;
#36581 = ORIENTED_EDGE ( 'NONE', *, *, #7414, .T. ) ;
#36582 = CARTESIAN_POINT ( 'NONE',  ( -21.47341775636118655, -0.1191753592594197858, 5.122631121243466090 ) ) ;
#36583 = AXIS2_PLACEMENT_3D ( 'NONE', #54571, #38394, #47189 ) ;
#36584 = FACE_OUTER_BOUND ( 'NONE', #6010, .T. ) ;
#36586 = VECTOR ( 'NONE', #4082, 1000.000000000000227 ) ;
#36585 = CARTESIAN_POINT ( 'NONE',  ( -17.26532721389163072, 0.000000000000000000, 13.67648636611514590 ) ) ;
#36587 = CARTESIAN_POINT ( 'NONE',  ( -15.82444748994319283, 0.000000000000000000, 7.651914174590189965 ) ) ;
#36588 = FACE_OUTER_BOUND ( 'NONE', #43748, .T. ) ;
#36589 = LINE ( 'NONE', #37148, #51262 ) ;
#36590 = CARTESIAN_POINT ( 'NONE',  ( -15.91372644746146037, -0.1191753592594204797, 6.273894133982523158 ) ) ;
#36591 = DIRECTION ( 'NONE',  ( 0.5364919789714477361, 0.6444004775717706579, 0.5449076811759711036 ) ) ;
#36592 = VECTOR ( 'NONE', #18060, 1000.000000000000114 ) ;
#36593 = CARTESIAN_POINT ( 'NONE',  ( -10.94028622754223967, 0.000000000000000000, 11.14038480894692995 ) ) ;
#36594 = VERTEX_POINT ( 'NONE', #44917 ) ;
#36595 = DIRECTION ( 'NONE',  ( 0.5364919789714477361, 0.6444004775717706579, 0.5449076811759711036 ) ) ;
#36596 = ORIENTED_EDGE ( 'NONE', *, *, #38548, .F. ) ;
#36597 = ADVANCED_FACE ( 'NONE', ( #22762 ), #6032, .F. ) ;
#36598 = VECTOR ( 'NONE', #22756, 999.9999999999998863 ) ;
#36599 = AXIS2_PLACEMENT_3D ( 'NONE', #33731, #50211, #49923 ) ;
#36600 = DIRECTION ( 'NONE',  ( -0.5449076811759708816, 0.6444004775717707689, 0.5364919789714475140 ) ) ;
#36601 = DIRECTION ( 'NONE',  ( -0.6427681459581293666, -0.7660444431189770143, -0.005002170337467561935 ) ) ;
#36602 = PLANE ( 'NONE',  #21300 ) ;
#36603 = DIRECTION ( 'NONE',  ( -0.005002170337468016433, -0.7660444431189770143, 0.6427681459581293666 ) ) ;
#36604 = EDGE_CURVE ( 'NONE', #931, #19450, #40663, .T. ) ;
#36605 = LINE ( 'NONE', #15851, #25046 ) ;
#36606 = DIRECTION ( 'NONE',  ( 0.6427681459581294776, -0.7660444431189769032, 0.005002170337467562802 ) ) ;
#36607 = CARTESIAN_POINT ( 'NONE',  ( -12.08591628628825276, 0.000000000000000000, 4.926357786634938840 ) ) ;
#36608 = AXIS2_PLACEMENT_3D ( 'NONE', #55322, #47090, #12476 ) ;
#36609 = CARTESIAN_POINT ( 'NONE',  ( -23.33693525117809386, 0.000000000000000000, 5.746789908705562944 ) ) ;
#36610 = ADVANCED_FACE ( 'NONE', ( #14276 ), #9142, .F. ) ;
#36611 = VECTOR ( 'NONE', #6247, 999.9999999999998863 ) ;
#36612 = DIRECTION ( 'NONE',  ( 0.000000000000000000, 0.000000000000000000, 1.000000000000000000 ) ) ;
#36613 = DIRECTION ( 'NONE',  ( 0.005961354470445682716, -0.6427876096865404731, -0.7660212471507180654 ) ) ;
#36614 = DIRECTION ( 'NONE',  ( 0.7660212471507180654, -0.6427876096865404731, 0.005961354470445141482 ) ) ;
#36615 = CARTESIAN_POINT ( 'NONE',  ( -15.87975247367846166, 0.000000000000000000, 2.850166870931599927 ) ) ;
#36616 = DIRECTION ( 'NONE',  ( -0.5449076811759708816, 0.6444004775717707689, 0.5364919789714475140 ) ) ;
#36617 = EDGE_CURVE ( 'NONE', #17974, #15806, #44349, .T. ) ;
#36618 = LINE ( 'NONE', #45149, #3281 ) ;
#36619 = EDGE_CURVE ( 'NONE', #5931, #30283, #5448, .T. ) ;
#36620 = EDGE_CURVE ( 'NONE', #38231, #52239, #5192, .T. ) ;
#36621 = DIRECTION ( 'NONE',  ( 0.005961354470445682716, -0.6427876096865404731, -0.7660212471507180654 ) ) ;
#36622 = CARTESIAN_POINT ( 'NONE',  ( -13.08408713167409942, -0.1191753592594197858, 1.863930203747758085 ) ) ;
#36623 = EDGE_CURVE ( 'NONE', #48904, #23765, #9732, .T. ) ;
#36624 = PLANE ( 'NONE',  #20467 ) ;
#36625 = DIRECTION ( 'NONE',  ( -0.005002170337468016433, -0.7660444431189770143, 0.6427681459581293666 ) ) ;
#36626 = ORIENTED_EDGE ( 'NONE', *, *, #12082, .T. ) ;
#36627 = ORIENTED_EDGE ( 'NONE', *, *, #9358, .T. ) ;
#36628 = AXIS2_PLACEMENT_3D ( 'NONE', #51534, #12625, #30788 ) ;
#36629 = CARTESIAN_POINT ( 'NONE',  ( -17.74404816805336793, 0.000000000000000000, 3.574322630375089460 ) ) ;
#36630 = CARTESIAN_POINT ( 'NONE',  ( -9.808144436391993182, 0.000000000000000000, 10.77986332834118777 ) ) ;
#36631 = VECTOR ( 'NONE', #20376, 1000.000000000000227 ) ;
#36632 = ORIENTED_EDGE ( 'NONE', *, *, #7444, .F. ) ;
#36633 = CARTESIAN_POINT ( 'NONE',  ( -14.90092180327158999, 0.000000000000000000, 8.397765404641738485 ) ) ;
#36634 = VECTOR ( 'NONE', #49027, 1000.000000000000114 ) ;
#36635 = ORIENTED_EDGE ( 'NONE', *, *, #53773, .T. ) ;
#36636 = CARTESIAN_POINT ( 'NONE',  ( 5.417481111513990477, -1.073353501383011110, -2.423381879925703419 ) ) ;
#36637 = ADVANCED_FACE ( 'NONE', ( #35545 ), #26751, .F. ) ;
#36638 = ORIENTED_EDGE ( 'NONE', *, *, #929, .T. ) ;
#36639 = VERTEX_POINT ( 'NONE', #18501 ) ;
#36640 = ORIENTED_EDGE ( 'NONE', *, *, #3670, .F. ) ;
#36641 = EDGE_CURVE ( 'NONE', #12052, #50963, #52854, .T. ) ;
#36642 = DIRECTION ( 'NONE',  ( 0.000000000000000000, 0.000000000000000000, 1.000000000000000000 ) ) ;
#36643 = VECTOR ( 'NONE', #22257, 1000.000000000000227 ) ;
#36644 = CARTESIAN_POINT ( 'NONE',  ( -18.85266870113162341, 1.743523803501506375, 3.949320956653499692 ) ) ;
#36645 = LINE ( 'NONE', #19035, #38497 ) ;
#36646 = VECTOR ( 'NONE', #53978, 1000.000000000000227 ) ;
#36647 = EDGE_CURVE ( 'NONE', #21379, #47620, #31293, .T. ) ;
#36648 = B_SPLINE_CURVE_WITH_KNOTS ( 'NONE', 3,
 ( #26779, #13452, #9171, #35307 ),
 .UNSPECIFIED., .F., .F.,
 ( 4, 4 ),
 ( 0.000000000000000000, 1.000000000000000000 ),
 .UNSPECIFIED. ) ;
#36649 = VERTEX_POINT ( 'NONE', #31588 ) ;
#36650 = EDGE_LOOP ( 'NONE', ( #32633, #45378, #20730, #1605 ) ) ;
#36651 = ADVANCED_FACE ( 'NONE', ( #10267 ), #36380, .F. ) ;
#36652 = VECTOR ( 'NONE', #3581, 999.9999999999998863 ) ;
#36653 = VECTOR ( 'NONE', #41005, 999.9999999999998863 ) ;
#36654 = DIRECTION ( 'NONE',  ( 0.007781995580012663651, -3.146120232559066537E-19, -0.9999697198139514409 ) ) ;
#36655 = VERTEX_POINT ( 'NONE', #4891 ) ;
#36656 = DIRECTION ( 'NONE',  ( -0.005961354470445682716, -0.6427876096865404731, 0.7660212471507180654 ) ) ;
#36657 = ORIENTED_EDGE ( 'NONE', *, *, #38680, .F. ) ;
#36658 = PLANE ( 'NONE',  #21252 ) ;
#36659 = CARTESIAN_POINT ( 'NONE',  ( -22.40634380310664397, 0.000000000000000000, 5.584705972946605534 ) ) ;
#36660 = ORIENTED_EDGE ( 'NONE', *, *, #9383, .T. ) ;
#36661 = LINE ( 'NONE', #40067, #34989 ) ;
#36662 = DIRECTION ( 'NONE',  ( -0.005002170337468016433, -0.7660444431189770143, 0.6427681459581293666 ) ) ;
#36663 = VECTOR ( 'NONE', #13108, 1000.000000000000000 ) ;
#36664 = VERTEX_POINT ( 'NONE', #1470 ) ;
#36665 = CARTESIAN_POINT ( 'NONE',  ( -14.94760462649100496, 0.000000000000000000, 2.488088991209854051 ) ) ;
#36666 = CARTESIAN_POINT ( 'NONE',  ( -20.54204810873173415, 0.000000000000000000, 4.860550213503115558 ) ) ;
#36667 = CARTESIAN_POINT ( 'NONE',  ( -17.40266420251354873, 0.000000000000000000, 5.623645764586359341 ) ) ;
#36668 = ORIENTED_EDGE ( 'NONE', *, *, #14519, .T. ) ;
#36669 = AXIS2_PLACEMENT_3D ( 'NONE', #53312, #31720, #49022 ) ;
#36670 = CARTESIAN_POINT ( 'NONE',  ( 2.072287782118878319, 0.000000000000000000, -2.950529333540147015 ) ) ;
#36671 = PLANE ( 'NONE',  #35108 ) ;
#36672 = DIRECTION ( 'NONE',  ( 0.3313982828793700097, 0.4028455766673915694, 0.8531650599175529814 ) ) ;
#36673 = CARTESIAN_POINT ( 'NONE',  ( -15.88130887279446490, 0.000000000000000000, 3.050160814894388839 ) ) ;
#36674 = LINE ( 'NONE', #2578, #1367 ) ;
#36675 = LINE ( 'NONE', #6861, #20673 ) ;
#36676 = CARTESIAN_POINT ( 'NONE',  ( -10.54003869734961718, 0.000000000000000000, 0.8757353956076227020 ) ) ;
#36677 = VERTEX_POINT ( 'NONE', #22216 ) ;
#36678 = CARTESIAN_POINT ( 'NONE',  ( -16.99924723426068951, 0.000000000000000000, 13.49389102713827171 ) ) ;
#36679 = PLANE ( 'NONE',  #5935 ) ;
#36680 = CARTESIAN_POINT ( 'NONE',  ( -68.36638157653975156, 9.462817827437976943E-12, -6.792143739499517885 ) ) ;
#36681 = VERTEX_POINT ( 'NONE', #39550 ) ;
#36682 = VECTOR ( 'NONE', #55087, 999.9999999999998863 ) ;
#36683 = CARTESIAN_POINT ( 'NONE',  ( -16.23369548331420020, 0.2864062442990022439, 3.657081181831572714 ) ) ;
#36684 = PLANE ( 'NONE',  #27256 ) ;
#36685 = VECTOR ( 'NONE', #37569, 1000.000000000000227 ) ;
#36686 = ADVANCED_FACE ( 'NONE', ( #11090 ), #6858, .F. ) ;
#36687 = DIRECTION ( 'NONE',  ( -0.9999697198139514409, -0.000000000000000000, -0.007781995580013368816 ) ) ;
#36688 = EDGE_CURVE ( 'NONE', #35922, #52348, #33263, .T. ) ;
#36689 = EDGE_CURVE ( 'NONE', #31243, #6083, #19896, .T. ) ;
#36690 = DIRECTION ( 'NONE',  ( -0.8531650599175527594, 0.4028455766673922356, 0.3313982828793700652 ) ) ;
#36691 = CARTESIAN_POINT ( 'NONE',  ( -56.75000000000000711, 6.050000000000001599, 2.449489742783185875 ) ) ;
#36692 = VERTEX_POINT ( 'NONE', #32673 ) ;
#36693 = AXIS2_PLACEMENT_3D ( 'NONE', #52356, #47818, #39582 ) ;
#36694 = VECTOR ( 'NONE', #3932, 999.9999999999998863 ) ;
#36695 = ORIENTED_EDGE ( 'NONE', *, *, #50355, .T. ) ;
#36696 = DIRECTION ( 'NONE',  ( 0.007781995580012663651, 0.000000000000000000, -0.9999697198139515519 ) ) ;
#36697 = DIRECTION ( 'NONE',  ( -0.5449076811759708816, 0.6444004775717707689, 0.5364919789714475140 ) ) ;
#36698 = ORIENTED_EDGE ( 'NONE', *, *, #24814, .T. ) ;
#36699 = DIRECTION ( 'NONE',  ( 0.005961354470445682716, -0.6427876096865404731, -0.7660212471507180654 ) ) ;
#36700 = ORIENTED_EDGE ( 'NONE', *, *, #34523, .F. ) ;
#36701 = CARTESIAN_POINT ( 'NONE',  ( -19.33760068587298164, 21.49370688441072019, 4.239878526350478793 ) ) ;
#36702 = AXIS2_PLACEMENT_3D ( 'NONE', #5903, #31737, #10974 ) ;
#36703 = ORIENTED_EDGE ( 'NONE', *, *, #49463, .F. ) ;
#36704 = ORIENTED_EDGE ( 'NONE', *, *, #53589, .T. ) ;
#36705 = AXIS2_PLACEMENT_3D ( 'NONE', #4037, #3476, #47470 ) ;
#36706 = LINE ( 'NONE', #22799, #28364 ) ;
#36707 = FACE_OUTER_BOUND ( 'NONE', #39962, .T. ) ;
#36708 = VECTOR ( 'NONE', #10577, 1000.000000000000227 ) ;
#36709 = LINE ( 'NONE', #2335, #8506 ) ;
#36710 = ORIENTED_EDGE ( 'NONE', *, *, #32286, .T. ) ;
#36711 = CARTESIAN_POINT ( 'NONE',  ( -13.96015179556829011, 0.000000000000000000, 6.927758415146698212 ) ) ;
#36712 = VERTEX_POINT ( 'NONE', #36964 ) ;
#36713 = EDGE_CURVE ( 'NONE', #28808, #485, #11667, .T. ) ;
#36714 = ORIENTED_EDGE ( 'NONE', *, *, #26825, .T. ) ;
#36715 = ORIENTED_EDGE ( 'NONE', *, *, #52340, .T. ) ;
#36716 = VECTOR ( 'NONE', #18856, 1000.000000000000114 ) ;
#36717 = CARTESIAN_POINT ( 'NONE',  ( -12.57354561117159797, 0.000000000000000000, 7.877219500929045992 ) ) ;
#36718 = VECTOR ( 'NONE', #24181, 1000.000000000000114 ) ;
#36719 = EDGE_CURVE ( 'NONE', #30987, #26051, #15619, .T. ) ;
#36720 = ORIENTED_EDGE ( 'NONE', *, *, #12194, .F. ) ;
#36721 = VECTOR ( 'NONE', #30449, 999.9999999999998863 ) ;
#36722 = FACE_OUTER_BOUND ( 'NONE', #47832, .T. ) ;
#36723 = ADVANCED_FACE ( 'NONE', ( #10828 ), #37212, .F. ) ;
#36724 = ORIENTED_EDGE ( 'NONE', *, *, #46594, .T. ) ;
#36725 = CARTESIAN_POINT ( 'NONE',  ( -27.56484202182514665, 16.74370688441070953, -4.657437592157546824 ) ) ;
#36726 = DIRECTION ( 'NONE',  ( -0.9090593428863094072, 0.000000000000000000, 0.4166666666666669072 ) ) ;
#36727 = VECTOR ( 'NONE', #4545, 999.9999999999998863 ) ;
#36728 = VERTEX_POINT ( 'NONE', #41493 ) ;
#36729 = EDGE_CURVE ( 'NONE', #3193, #1369, #19335, .T. ) ;
#36730 = PLANE ( 'NONE',  #521 ) ;
#36731 = ORIENTED_EDGE ( 'NONE', *, *, #26730, .F. ) ;
#36732 = CIRCLE ( 'NONE', #45752, 2.749999999999997335 ) ;
#36733 = CARTESIAN_POINT ( 'NONE',  ( -19.60834386242827776, 0.000000000000000000, 4.298478389818581213 ) ) ;
#36734 = VECTOR ( 'NONE', #21728, 1000.000000000000000 ) ;
#36735 = FACE_OUTER_BOUND ( 'NONE', #5716, .T. ) ;
#36736 = PLANE ( 'NONE',  #14160 ) ;
#36737 = DIRECTION ( 'NONE',  ( 0.005961354470445682716, -0.6427876096865404731, -0.7660212471507180654 ) ) ;
#36738 = DIRECTION ( 'NONE',  ( -0.7660212471507179544, -0.6427876096865405842, -0.005961354470445141482 ) ) ;
#36739 = DIRECTION ( 'NONE',  ( -0.9999697198139514409, -0.000000000000000000, -0.007781995580013368816 ) ) ;
#36740 = FILL_AREA_STYLE_COLOUR ( '', #9292 ) ;
#36741 = ORIENTED_EDGE ( 'NONE', *, *, #33957, .F. ) ;
#36742 = VERTEX_POINT ( 'NONE', #7388 ) ;
#36743 = DIRECTION ( 'NONE',  ( 0.6427681459581294776, -0.7660444431189769032, 0.005002170337467562802 ) ) ;
#36744 = CARTESIAN_POINT ( 'NONE',  ( -22.52493451062505869, 5.467268677019012202, 14.60348995783060211 ) ) ;
#36745 = LINE ( 'NONE', #22071, #14921 ) ;
#36746 = DIRECTION ( 'NONE',  ( 0.6427681459581294776, -0.7660444431189769032, 0.005002170337467562802 ) ) ;
#36747 = VECTOR ( 'NONE', #40813, 1000.000000000000227 ) ;
#36748 = LINE ( 'NONE', #1550, #429 ) ;
#36749 = ORIENTED_EDGE ( 'NONE', *, *, #36904, .T. ) ;
#36750 = VECTOR ( 'NONE', #31972, 999.9999999999998863 ) ;
#36751 = LINE ( 'NONE', #14347, #54838 ) ;
#36752 = DIRECTION ( 'NONE',  ( 0.9999697198139515519, 0.000000000000000000, 0.007781995580013368816 ) ) ;
#36753 = EDGE_LOOP ( 'NONE', ( #13417, #10532, #10076, #24369 ) ) ;
#36754 = FACE_OUTER_BOUND ( 'NONE', #4383, .T. ) ;
#36755 = EDGE_CURVE ( 'NONE', #6150, #8005, #28720, .T. ) ;
#36756 = FACE_OUTER_BOUND ( 'NONE', #34235, .T. ) ;
#36757 = VECTOR ( 'NONE', #53914, 1000.000000000000227 ) ;
#36758 = VERTEX_POINT ( 'NONE', #41204 ) ;
#36759 = ADVANCED_FACE ( 'NONE', ( #28137 ), #19634, .F. ) ;
#36760 = LINE ( 'NONE', #24798, #37052 ) ;
#36761 = CARTESIAN_POINT ( 'NONE',  ( -50.99228148001754590, 2.341865487272625668, 5.000000000000000000 ) ) ;
#36762 = VECTOR ( 'NONE', #53622, 1000.000000000000227 ) ;
#36763 = DIRECTION ( 'NONE',  ( -0.005961354470445682716, -0.6427876096865404731, 0.7660212471507180654 ) ) ;
#36764 = EDGE_CURVE ( 'NONE', #5849, #17764, #45729, .T. ) ;
#36765 = DIRECTION ( 'NONE',  ( 0.9999697198139515519, 0.000000000000000000, 0.007781995580013368816 ) ) ;
#36766 = CARTESIAN_POINT ( 'NONE',  ( -13.58223596932098154, 4.819660872929010687, 10.06700741326545234 ) ) ;
#36767 = ORIENTED_EDGE ( 'NONE', *, *, #47587, .T. ) ;
#36768 = VECTOR ( 'NONE', #42935, 1000.000000000000114 ) ;
#36769 = CIRCLE ( 'NONE', #42226, 2.750000000000001776 ) ;
#36770 = VERTEX_POINT ( 'NONE', #45196 ) ;
#36771 = VECTOR ( 'NONE', #2014, 1000.000000000000227 ) ;
#36772 = CARTESIAN_POINT ( 'NONE',  ( -18.49718515159138477, -1.003701604285657911, 4.034232660979946594 ) ) ;
#36773 = CARTESIAN_POINT ( 'NONE',  ( 2.072287782118878319, 0.000000000000000000, -2.950529333540147015 ) ) ;
#36774 = FACE_OUTER_BOUND ( 'NONE', #29440, .T. ) ;
#36775 = AXIS2_PLACEMENT_3D ( 'NONE', #45607, #41072, #19496 ) ;
#36777 = DIRECTION ( 'NONE',  ( -0.005002170337468016433, -0.7660444431189770143, 0.6427681459581293666 ) ) ;
#36776 = VECTOR ( 'NONE', #46856, 1000.000000000000114 ) ;
#36778 = FACE_OUTER_BOUND ( 'NONE', #35856, .T. ) ;
#36779 = ORIENTED_EDGE ( 'NONE', *, *, #48482, .F. ) ;
#36780 = DIRECTION ( 'NONE',  ( 0.7660212471507180654, -0.6427876096865404731, 0.005961354470445141482 ) ) ;
#36781 = EDGE_CURVE ( 'NONE', #33095, #22624, #32961, .T. ) ;
#36782 = VECTOR ( 'NONE', #51979, 1000.000000000000227 ) ;
#36783 = DIRECTION ( 'NONE',  ( -0.6427681459581293666, -0.7660444431189770143, -0.005002170337467561935 ) ) ;
#36784 = VECTOR ( 'NONE', #6937, 1000.000000000000114 ) ;
#36785 = CARTESIAN_POINT ( 'NONE',  ( -16.49925689037891985, 0.000000000000000000, 8.954664917442258343 ) ) ;
#36786 = ORIENTED_EDGE ( 'NONE', *, *, #38472, .T. ) ;
#36787 = CARTESIAN_POINT ( 'NONE',  ( -11.15221203998479460, 0.000000000000000000, 4.364285962950406272 ) ) ;
#36788 = ORIENTED_EDGE ( 'NONE', *, *, #3852, .F. ) ;
#36789 = DIRECTION ( 'NONE',  ( 0.6427681459581294776, -0.7660444431189769032, 0.005002170337467562802 ) ) ;
#36790 = DIRECTION ( 'NONE',  ( 0.000000000000000000, -0.000000000000000000, -1.000000000000000000 ) ) ;
#36791 = ORIENTED_EDGE ( 'NONE', *, *, #35450, .F. ) ;
#36792 = DIRECTION ( 'NONE',  ( -0.5364919789714478471, 0.6444004775717705469, -0.5449076811759709926 ) ) ;
#36793 = ORIENTED_EDGE ( 'NONE', *, *, #27797, .T. ) ;
#36794 = CIRCLE ( 'NONE', #25936, 0.2499999999999997780 ) ;
#36795 = VERTEX_POINT ( 'NONE', #2575 ) ;
#36796 = ORIENTED_EDGE ( 'NONE', *, *, #24478, .T. ) ;
#36797 = CARTESIAN_POINT ( 'NONE',  ( -14.07714710935361779, 2.714935509636509536, 2.063353073686676531 ) ) ;
#36798 = ORIENTED_EDGE ( 'NONE', *, *, #19807, .T. ) ;
#36799 = AXIS2_PLACEMENT_3D ( 'NONE', #25147, #20856, #38175 ) ;
#36800 = ORIENTED_EDGE ( 'NONE', *, *, #14782, .F. ) ;
#36801 = CARTESIAN_POINT ( 'NONE',  ( -20.51915365390780011, -2.298917212465658721, 4.778309734519891272 ) ) ;
#36802 = VECTOR ( 'NONE', #41823, 1000.000000000000227 ) ;
#36803 = ORIENTED_EDGE ( 'NONE', *, *, #1808, .T. ) ;
#36804 = EDGE_LOOP ( 'NONE', ( #46540, #46382, #28248, #27798 ) ) ;
#36805 = CARTESIAN_POINT ( 'NONE',  ( -58.00000000000000711, -8.999999999999998224, 7.102951435054649637E-15 ) ) ;
#36806 = EDGE_CURVE ( 'NONE', #54647, #13476, #2831, .T. ) ;
#36807 = EDGE_LOOP ( 'NONE', ( #1834, #50348, #31651, #6144 ) ) ;
#36808 = VECTOR ( 'NONE', #33264, 1000.000000000000227 ) ;
#36809 = VERTEX_POINT ( 'NONE', #6297 ) ;
#36810 = ORIENTED_EDGE ( 'NONE', *, *, #41490, .F. ) ;
#36811 = VECTOR ( 'NONE', #42460, 1000.000000000000227 ) ;
#36812 = VECTOR ( 'NONE', #41592, 1000.000000000000227 ) ;
#36813 = DIRECTION ( 'NONE',  ( 0.007781995580012663651, 0.000000000000000000, -0.9999697198139515519 ) ) ;
#36814 = DIRECTION ( 'NONE',  ( 0.007781995580012662783, 0.000000000000000000, -0.9999697198139514409 ) ) ;
#36815 = DIRECTION ( 'NONE',  ( 0.3535533905932752297, -0.6123724356957952475, -0.7071067811865462405 ) ) ;
#36816 = CARTESIAN_POINT ( 'NONE',  ( -19.60834386242827776, 0.000000000000000000, 4.298478389818581213 ) ) ;
#36817 = ORIENTED_EDGE ( 'NONE', *, *, #17574, .T. ) ;
#36818 = LINE ( 'NONE', #54134, #3853 ) ;
#36819 = ORIENTED_EDGE ( 'NONE', *, *, #11928, .F. ) ;
#36820 = VECTOR ( 'NONE', #20255, 1000.000000000000227 ) ;
#36821 = EDGE_CURVE ( 'NONE', #11634, #25655, #11385, .T. ) ;
#36822 = ORIENTED_EDGE ( 'NONE', *, *, #52496, .F. ) ;
#36823 = VECTOR ( 'NONE', #53070, 1000.000000000000227 ) ;
#36824 = AXIS2_PLACEMENT_3D ( 'NONE', #12477, #17010, #25801 ) ;
#36825 = PLANE ( 'NONE',  #54724 ) ;
#36826 = EDGE_CURVE ( 'NONE', #40568, #27421, #54814, .T. ) ;
#36827 = ADVANCED_FACE ( 'NONE', ( #50273 ), #7135, .F. ) ;
#36828 = AXIS2_PLACEMENT_3D ( 'NONE', #41323, #49572, #53804 ) ;
#36829 = DIRECTION ( 'NONE',  ( 0.005961354470445682716, -0.6427876096865404731, -0.7660212471507180654 ) ) ;
#36830 = AXIS2_PLACEMENT_3D ( 'NONE', #27184, #44491, #40244 ) ;
#36831 = CARTESIAN_POINT ( 'NONE',  ( -16.81345671998191449, 0.000000000000000000, 3.412238694616132495 ) ) ;
#36832 = LINE ( 'NONE', #19193, #39349 ) ;
#36833 = CARTESIAN_POINT ( 'NONE',  ( -20.52784467904771759, 0.000000000000000000, 14.94375894514125491 ) ) ;
#36834 = ORIENTED_EDGE ( 'NONE', *, *, #53268, .T. ) ;
#36835 = LINE ( 'NONE', #46159, #47412 ) ;
#36836 = EDGE_CURVE ( 'NONE', #2309, #17653, #40916, .T. ) ;
#36837 = VERTEX_POINT ( 'NONE', #29838 ) ;
#36838 = CARTESIAN_POINT ( 'NONE',  ( -14.94916102560700821, 0.000000000000000000, 2.688082935172642962 ) ) ;
#36839 = CARTESIAN_POINT ( 'NONE',  ( -24.26908309836554878, 0.000000000000000000, 6.108867788427308376 ) ) ;
#36840 = ADVANCED_FACE ( 'NONE', ( #3690 ), #46568, .F. ) ;
#36841 = FACE_OUTER_BOUND ( 'NONE', #21265, .T. ) ;
#36842 = CARTESIAN_POINT ( 'NONE',  ( -12.47550013608699260, 3.524445264749008988, 7.511444159126568820 ) ) ;
#36843 = EDGE_CURVE ( 'NONE', #54306, #1702, #46876, .T. ) ;
#36844 = LINE ( 'NONE', #23493, #14170 ) ;
#36845 = AXIS2_PLACEMENT_3D ( 'NONE', #42690, #7493, #29363 ) ;
#36846 = EDGE_LOOP ( 'NONE', ( #32033, #47439, #238, #42456 ) ) ;
#36847 = DIRECTION ( 'NONE',  ( 0.000000000000000000, 0.000000000000000000, -1.000000000000000000 ) ) ;
#36848 = DIRECTION ( 'NONE',  ( -0.005961354470445682716, -0.6427876096865404731, 0.7660212471507180654 ) ) ;
#36849 = FACE_OUTER_BOUND ( 'NONE', #15112, .T. ) ;
#36850 = VECTOR ( 'NONE', #22574, 1000.000000000000227 ) ;
#36851 = EDGE_CURVE ( 'NONE', #45499, #17332, #47135, .T. ) ;
#36852 = CARTESIAN_POINT ( 'NONE',  ( -10.32946152485258295, -0.1191753592594181482, 5.209355965425340962 ) ) ;
#36853 = AXIS2_PLACEMENT_3D ( 'NONE', #44295, #22703, #48243 ) ;
#36854 = DIRECTION ( 'NONE',  ( -0.9321478471874540261, 0.000000000000000000, 0.3620778797217457656 ) ) ;
#36855 = LINE ( 'NONE', #15262, #46394 ) ;
#36856 = CARTESIAN_POINT ( 'NONE',  ( -1.086233639165236964, -1.000000000000000000, -2.796443541562362078 ) ) ;
#36857 = EDGE_CURVE ( 'NONE', #37024, #41757, #29563, .T. ) ;
#36858 = VECTOR ( 'NONE', #4821, 1000.000000000000227 ) ;
#36859 = VECTOR ( 'NONE', #56021, 1000.000000000000227 ) ;
#36860 = CARTESIAN_POINT ( 'NONE',  ( -16.35723548322975418, 2.067327705546507133, 6.627863836689923183 ) ) ;
#36861 = DIRECTION ( 'NONE',  ( -0.5449076811759708816, 0.6444004775717707689, 0.5364919789714475140 ) ) ;
#36862 = VECTOR ( 'NONE', #7089, 999.9999999999998863 ) ;
#36863 = ORIENTED_EDGE ( 'NONE', *, *, #45821, .T. ) ;
#36864 = VECTOR ( 'NONE', #51545, 1000.000000000000227 ) ;
#36865 = AXIS2_PLACEMENT_3D ( 'NONE', #17718, #35058, #928 ) ;
#36866 = ORIENTED_EDGE ( 'NONE', *, *, #9267, .T. ) ;
#36867 = AXIS2_PLACEMENT_3D ( 'NONE', #5275, #974, #34258 ) ;
#36868 = ORIENTED_EDGE ( 'NONE', *, *, #15639, .T. ) ;
#36869 = ORIENTED_EDGE ( 'NONE', *, *, #38088, .T. ) ;
#36870 = VERTEX_POINT ( 'NONE', #25293 ) ;
#36871 = LINE ( 'NONE', #15274, #43232 ) ;
#36872 = FACE_OUTER_BOUND ( 'NONE', #35386, .T. ) ;
#36873 = VERTEX_POINT ( 'NONE', #55960 ) ;
#36874 = DIRECTION ( 'NONE',  ( 0.9999697198139515519, 0.000000000000000000, 0.007781995580013368816 ) ) ;
#36875 = ADVANCED_FACE ( 'NONE', ( #12519 ), #8237, .F. ) ;
#36876 = ORIENTED_EDGE ( 'NONE', *, *, #48716, .F. ) ;
#36877 = VERTEX_POINT ( 'NONE', #50827 ) ;
#36878 = VECTOR ( 'NONE', #21302, 999.9999999999998863 ) ;
#36879 = CARTESIAN_POINT ( 'NONE',  ( -66.93067463247570004, -9.369820663055195453, 6.899827505725927068 ) ) ;
#36880 = CARTESIAN_POINT ( 'NONE',  ( -22.40634380310664397, 0.000000000000000000, 5.584705972946605534 ) ) ;
#36881 = CARTESIAN_POINT ( 'NONE',  ( -15.56710904319146671, 0.000000000000000000, 8.592587037720512910 ) ) ;
#36882 = ORIENTED_EDGE ( 'NONE', *, *, #34753, .T. ) ;
#36883 = VECTOR ( 'NONE', #650, 1000.000000000000114 ) ;
#36884 = CARTESIAN_POINT ( 'NONE',  ( 5.454592090961234874, -6.230699628392517120, -2.061810099490657411 ) ) ;
#36885 = EDGE_CURVE ( 'NONE', #2328, #18331, #34370, .T. ) ;
#36886 = CARTESIAN_POINT ( 'NONE',  ( -25.20200914511100265, -0.1191753592594197858, 6.570942640130446932 ) ) ;
#36887 = VECTOR ( 'NONE', #29137, 1000.000000000000227 ) ;
#36888 = CARTESIAN_POINT ( 'NONE',  ( -11.87243407472968926, 0.000000000000000000, 11.50246268866867361 ) ) ;
#36889 = ADVANCED_FACE ( 'NONE', ( #34629 ), #12779, .F. ) ;
#36890 = CARTESIAN_POINT ( 'NONE',  ( 1.086233639165236964, 0.000000000000000000, 2.796443541562362078 ) ) ;
#36891 = CARTESIAN_POINT ( 'NONE',  ( -12.15271748404464880, 0.000000000000000000, 1.601849296007406664 ) ) ;
#36892 = VECTOR ( 'NONE', #26330, 1000.000000000000227 ) ;
#36893 = DIRECTION ( 'NONE',  ( 0.9999697198139515519, 0.000000000000000000, 0.007781995580013368816 ) ) ;
#36894 = CARTESIAN_POINT ( 'NONE',  ( -17.41128636302939725, 0.000000000000000000, 6.731574874359651517 ) ) ;
#36895 = CARTESIAN_POINT ( 'NONE',  ( 2.072287782118878319, 0.000000000000000000, -2.950529333540147015 ) ) ;
#36896 = DIRECTION ( 'NONE',  ( 0.7660212471507180654, -0.6427876096865404731, 0.005961354470445141482 ) ) ;
#36897 = EDGE_LOOP ( 'NONE', ( #36067, #28716, #9698, #601 ) ) ;
#36898 = CARTESIAN_POINT ( 'NONE',  ( -27.13182931993292257, 16.99370688441070953, -4.657437592157546824 ) ) ;
#36899 = VERTEX_POINT ( 'NONE', #11923 ) ;
#36900 = AXIS2_PLACEMENT_3D ( 'NONE', #4744, #22068, #29474 ) ;
#36901 = DIRECTION ( 'NONE',  ( -0.9999697198139514409, -0.000000000000000000, -0.007781995580013368816 ) ) ;
#36902 = CARTESIAN_POINT ( 'NONE',  ( -11.67244013076689946, 0.000000000000000000, 11.50401908778467863 ) ) ;
#36903 = PLANE ( 'NONE',  #51257 ) ;
#36904 = EDGE_CURVE ( 'NONE', #54774, #1287, #34101, .T. ) ;
#36905 = PLANE ( 'NONE',  #33200 ) ;
#36906 = CARTESIAN_POINT ( 'NONE',  ( -20.54479086174542957, 3.200641362704010007, 4.560108989559846115 ) ) ;
#36907 = FACE_OUTER_BOUND ( 'NONE', #6172, .T. ) ;
#36908 = VECTOR ( 'NONE', #25523, 999.9999999999998863 ) ;
#36909 = ADVANCED_FACE ( 'NONE', ( #25014 ), #3980, .F. ) ;
#36910 = AXIS2_PLACEMENT_3D ( 'NONE', #22160, #589, #52273 ) ;
#36911 = LINE ( 'NONE', #19008, #1990 ) ;
#36912 = CARTESIAN_POINT ( 'NONE',  ( -12.80458192191714595, 0.000000000000000000, 11.86454056839041726 ) ) ;
#36913 = CARTESIAN_POINT ( 'NONE',  ( 2.072287782118878319, 0.000000000000000000, -2.950529333540147015 ) ) ;
#36914 = DIRECTION ( 'NONE',  ( 0.005961354470445682716, -0.6427876096865404731, -0.7660212471507180654 ) ) ;
#36915 = FACE_OUTER_BOUND ( 'NONE', #30720, .T. ) ;
#36916 = CARTESIAN_POINT ( 'NONE',  ( -9.136524801126023831, 0.000000000000000000, 3.471982353925851861 ) ) ;
#36917 = EDGE_CURVE ( 'NONE', #22139, #38141, #29252, .T. ) ;
#36918 = LINE ( 'NONE', #19016, #51789 ) ;
#36919 = FACE_OUTER_BOUND ( 'NONE', #13914, .T. ) ;
#36920 = CARTESIAN_POINT ( 'NONE',  ( 2.072287782118878319, 0.000000000000000000, -2.950529333540147015 ) ) ;
#36921 = LINE ( 'NONE', #10522, #27470 ) ;
#36922 = AXIS2_PLACEMENT_3D ( 'NONE', #9974, #13946, #23036 ) ;
#36923 = ORIENTED_EDGE ( 'NONE', *, *, #41430, .F. ) ;
#36924 = DIRECTION ( 'NONE',  ( 0.6427681459581294776, -0.7660444431189769032, 0.005002170337467562802 ) ) ;
#36925 = VERTEX_POINT ( 'NONE', #56217 ) ;
#36926 = CARTESIAN_POINT ( 'NONE',  ( -8.830583954895368848, 0.000000000000000000, 4.582359465753242489 ) ) ;
#36927 = CARTESIAN_POINT ( 'NONE',  ( -19.32961685222932147, 0.000000000000000000, 14.39908572644263351 ) ) ;
#36928 = EDGE_LOOP ( 'NONE', ( #52984, #42765, #26357, #45583 ) ) ;
#36929 = CARTESIAN_POINT ( 'NONE',  ( -20.54204810873173415, 0.000000000000000000, 4.860550213503115558 ) ) ;
#36930 = VECTOR ( 'NONE', #47885, 1000.000000000000114 ) ;
#36931 = EDGE_LOOP ( 'NONE', ( #28262, #10887, #35591, #4034 ) ) ;
#36932 = CARTESIAN_POINT ( 'NONE',  ( -13.92048961155144937, -3.270328918600660995, 7.456289541356968975 ) ) ;
#36933 = VECTOR ( 'NONE', #21739, 1000.000000000000114 ) ;
#36934 = VERTEX_POINT ( 'NONE', #38637 ) ;
#36935 = ORIENTED_EDGE ( 'NONE', *, *, #36145, .F. ) ;
#36936 = ORIENTED_EDGE ( 'NONE', *, *, #12533, .F. ) ;
#36937 = DIRECTION ( 'NONE',  ( 0.9999697198139515519, 0.000000000000000000, 0.007781995580013368816 ) ) ;
#36938 = DIRECTION ( 'NONE',  ( -0.5364919789714478471, 0.6444004775717705469, -0.5449076811759709926 ) ) ;
#36939 = CARTESIAN_POINT ( 'NONE',  ( -18.67697421479882181, -0.1191753592594197858, 4.036397482078229793 ) ) ;
#36940 = EDGE_CURVE ( 'NONE', #35444, #8247, #43445, .T. ) ;
#36941 = AXIS2_PLACEMENT_3D ( 'NONE', #5262, #41280, #6635 ) ;
#36942 = ORIENTED_EDGE ( 'NONE', *, *, #41198, .F. ) ;
#36944 = ORIENTED_EDGE ( 'NONE', *, *, #28803, .F. ) ;
#36943 = EDGE_CURVE ( 'NONE', #39017, #9012, #21851, .T. ) ;
#36945 = DIRECTION ( 'NONE',  ( 0.005002170337468016433, -0.7660444431189770143, -0.6427681459581293666 ) ) ;
#36947 = EDGE_CURVE ( 'NONE', #27291, #15255, #17054, .T. ) ;
#36946 = ORIENTED_EDGE ( 'NONE', *, *, #12276, .T. ) ;
#36948 = DIRECTION ( 'NONE',  ( 0.6427681459581294776, -0.7660444431189769032, 0.005002170337467562802 ) ) ;
#36949 = EDGE_LOOP ( 'NONE', ( #3396, #8099, #20587, #28543 ) ) ;
#36950 = CARTESIAN_POINT ( 'NONE',  ( 5.284044854955649129, -1.088655197871726710, 2.393421119419573806 ) ) ;
#36951 = CARTESIAN_POINT ( 'NONE',  ( -18.76354595665420177, -0.1191753592594177458, 14.21882498613976331 ) ) ;
#36952 = EDGE_CURVE ( 'NONE', #16268, #43785, #51114, .T. ) ;
#36953 = EDGE_CURVE ( 'NONE', #19164, #30303, #33666, .T. ) ;
#36954 = EDGE_CURVE ( 'NONE', #30608, #48670, #8831, .T. ) ;
#36955 = VERTEX_POINT ( 'NONE', #49091 ) ;
#36956 = DIRECTION ( 'NONE',  ( 0.5449076811759707706, 0.6444004775717708799, -0.5364919789714476250 ) ) ;
#36957 = CARTESIAN_POINT ( 'NONE',  ( -17.31051119149000428, -0.1191753592594168992, 6.632356101936254689 ) ) ;
#36958 = ORIENTED_EDGE ( 'NONE', *, *, #36191, .T. ) ;
#36959 = CARTESIAN_POINT ( 'NONE',  ( -14.46888367232926420, 0.000000000000000000, 12.59025272694991315 ) ) ;
#36960 = FACE_OUTER_BOUND ( 'NONE', #43388, .T. ) ;
#36961 = ORIENTED_EDGE ( 'NONE', *, *, #47027, .T. ) ;
#36962 = FACE_OUTER_BOUND ( 'NONE', #15246, .T. ) ;
#36963 = DIRECTION ( 'NONE',  ( 0.007781995580012663651, 0.000000000000000000, -0.9999697198139515519 ) ) ;
#36964 = CARTESIAN_POINT ( 'NONE',  ( -9.712109199288757821, 0.000000000000000000, 1.990174743821643055 ) ) ;
#36965 = EDGE_CURVE ( 'NONE', #29764, #42740, #44293, .T. ) ;
#36966 = FACE_OUTER_BOUND ( 'NONE', #39918, .T. ) ;
#36967 = FACE_OUTER_BOUND ( 'NONE', #27496, .T. ) ;
#36968 = CARTESIAN_POINT ( 'NONE',  ( -17.87304920636520222, 0.000000000000000000, 6.358649259333880366 ) ) ;
#36969 = ADVANCED_FACE ( 'NONE', ( #52785 ), #1098, .F. ) ;
#36970 = VECTOR ( 'NONE', #14905, 1000.000000000000227 ) ;
#36971 = CARTESIAN_POINT ( 'NONE',  ( -66.51077781314475601, -11.33477655279809326, 1.402349447197485777 ) ) ;
#36972 = ORIENTED_EDGE ( 'NONE', *, *, #53482, .F. ) ;
#36973 = CARTESIAN_POINT ( 'NONE',  ( -16.21461322262780058, -2.137015261443158565, 6.487444273011554685 ) ) ;
#36974 = EDGE_CURVE ( 'NONE', #42260, #17024, #17656, .T. ) ;
#36975 = CARTESIAN_POINT ( 'NONE',  ( -66.44888886210301848, -1.718375678206839771E-11, -0.7138195548296715209 ) ) ;
#36976 = EDGE_LOOP ( 'NONE', ( #30142, #50505, #50316, #3412 ) ) ;
#36977 = DIRECTION ( 'NONE',  ( 0.000000000000000000, -0.000000000000000000, -1.000000000000000000 ) ) ;
#36978 = DIRECTION ( 'NONE',  ( -0.5364919789714478471, 0.6444004775717705469, -0.5449076811759709926 ) ) ;
#36979 = EDGE_CURVE ( 'NONE', #51394, #42909, #47983, .T. ) ;
#36980 = AXIS2_PLACEMENT_3D ( 'NONE', #42661, #12852, #29643 ) ;
#36981 = CARTESIAN_POINT ( 'NONE',  ( -24.26986129792355129, -0.1191753592594197858, 6.208864760408702388 ) ) ;
#36982 = CARTESIAN_POINT ( 'NONE',  ( -10.44305056480239102, 0.000000000000000000, 6.955129310174771540 ) ) ;
#36983 = EDGE_CURVE ( 'NONE', #9162, #42368, #27236, .T. ) ;
#36984 = CARTESIAN_POINT ( 'NONE',  ( 0.000000000000000000, -1.000000000000000000, 0.000000000000000000 ) ) ;
#36985 = EDGE_LOOP ( 'NONE', ( #14222, #18219, #33567 ) ) ;
#36986 = VERTEX_POINT ( 'NONE', #30683 ) ;
#36987 = LINE ( 'NONE', #15379, #51297 ) ;
#36988 = LINE ( 'NONE', #37823, #11161 ) ;
#36989 = EDGE_LOOP ( 'NONE', ( #9257, #17221, #13049, #31357 ) ) ;
#36990 = CARTESIAN_POINT ( 'NONE',  ( -17.80242246511569348, -0.1191753592594190225, 10.13343903392645373 ) ) ;
#36991 = EDGE_LOOP ( 'NONE', ( #16244, #36417, #25895, #49348, #8557 ) ) ;
#36992 = CARTESIAN_POINT ( 'NONE',  ( -11.87243407472968926, 0.000000000000000000, 11.50246268866867361 ) ) ;
#36993 = EDGE_LOOP ( 'NONE', ( #46523, #44085, #30812, #36504 ) ) ;
#36994 = VERTEX_POINT ( 'NONE', #53092 ) ;
#36995 = DIRECTION ( 'NONE',  ( 0.007781995580012663651, -3.146120232559066537E-19, -0.9999697198139514409 ) ) ;
#36996 = DIRECTION ( 'NONE',  ( 0.007781995580012662783, 0.000000000000000000, -0.9999697198139514409 ) ) ;
#36997 = DIRECTION ( 'NONE',  ( 0.9999697198139515519, 0.000000000000000000, 0.007781995580013368816 ) ) ;
#36998 = ORIENTED_EDGE ( 'NONE', *, *, #25020, .F. ) ;
#36999 = FACE_OUTER_BOUND ( 'NONE', #36804, .T. ) ;
#37000 = ORIENTED_EDGE ( 'NONE', *, *, #49463, .T. ) ;
#37001 = ORIENTED_EDGE ( 'NONE', *, *, #38978, .F. ) ;
#37002 = ORIENTED_EDGE ( 'NONE', *, *, #4325, .T. ) ;
#37003 = CARTESIAN_POINT ( 'NONE',  ( -46.52156441860518754, 5.799038105676674881, 5.000000000000000000 ) ) ;
#37004 = EDGE_LOOP ( 'NONE', ( #40641, #22303, #29718, #25284 ) ) ;
#37005 = LINE ( 'NONE', #55154, #33908 ) ;
#37006 = ORIENTED_EDGE ( 'NONE', *, *, #18527, .T. ) ;
#37007 = CARTESIAN_POINT ( 'NONE',  ( -19.63273726619797088, -2.181752617796719029, 7.099516195845842148 ) ) ;
#37008 = CARTESIAN_POINT ( 'NONE',  ( -24.62525945952572215, 18.15220053346459750, 4.407440554554201917 ) ) ;
#37009 = EDGE_CURVE ( 'NONE', #11612, #48717, #33104, .T. ) ;
#37010 = EDGE_CURVE ( 'NONE', #34036, #22830, #44548, .T. ) ;
#37011 = VECTOR ( 'NONE', #29721, 1000.000000000000227 ) ;
#37012 = VERTEX_POINT ( 'NONE', #26388 ) ;
#37013 = CARTESIAN_POINT ( 'NONE',  ( -18.48776216474505674, 0.000000000000000000, 10.04718611902029934 ) ) ;
#37014 = ORIENTED_EDGE ( 'NONE', *, *, #28741, .F. ) ;
#37015 = EDGE_CURVE ( 'NONE', #6991, #44267, #35770, .T. ) ;
#37016 = LINE ( 'NONE', #50339, #19218 ) ;
#37017 = DIRECTION ( 'NONE',  ( -0.7660212471507179544, -0.6427876096865405842, -0.005961354470445141482 ) ) ;
#37018 = CARTESIAN_POINT ( 'NONE',  ( -16.81267852042391198, -0.1191753592594197858, 3.312241722634738039 ) ) ;
#37019 = FACE_OUTER_BOUND ( 'NONE', #33940, .T. ) ;
#37020 = CARTESIAN_POINT ( 'NONE',  ( -14.20280369269832832, 0.000000000000000000, 12.40765738797303719 ) ) ;
#37021 = DIRECTION ( 'NONE',  ( 0.000000000000000000, -0.000000000000000000, -1.000000000000000000 ) ) ;
#37022 = CARTESIAN_POINT ( 'NONE',  ( -9.908141408373387193, -0.1191753592594197858, 10.77908512878318703 ) ) ;
#37023 = ORIENTED_EDGE ( 'NONE', *, *, #12836, .F. ) ;
#37024 = VERTEX_POINT ( 'NONE', #9935 ) ;
#37025 = DIRECTION ( 'NONE',  ( 0.005961354470445682716, -0.6427876096865404731, -0.7660212471507180654 ) ) ;
#37026 = CARTESIAN_POINT ( 'NONE',  ( 2.072287782118878319, 0.000000000000000000, -2.950529333540147015 ) ) ;
#37027 = DIRECTION ( 'NONE',  ( 0.007781995580012663651, -3.146120232559066537E-19, -0.9999697198139514409 ) ) ;
#37028 = DIRECTION ( 'NONE',  ( -0.005961354470445682716, -0.6427876096865404731, 0.7660212471507180654 ) ) ;
#37029 = CARTESIAN_POINT ( 'NONE',  ( -1.602641424070903486, 5.553834702102301790, 3.840893930704793569 ) ) ;
#37030 = ORIENTED_EDGE ( 'NONE', *, *, #9128, .T. ) ;
#37031 = LINE ( 'NONE', #29052, #34063 ) ;
#37032 = FACE_OUTER_BOUND ( 'NONE', #45255, .T. ) ;
#37033 = ORIENTED_EDGE ( 'NONE', *, *, #3975, .T. ) ;
#37034 = DIRECTION ( 'NONE',  ( -0.005961354470445682716, -0.6427876096865404731, 0.7660212471507180654 ) ) ;
#37035 = CARTESIAN_POINT ( 'NONE',  ( -15.86710544311044302, 0.000000000000000000, 13.13336954653252953 ) ) ;
#37036 = ORIENTED_EDGE ( 'NONE', *, *, #48033, .F. ) ;
#37037 = FACE_OUTER_BOUND ( 'NONE', #17575, .T. ) ;
#37038 = DIRECTION ( 'NONE',  ( 0.007781995580012663651, -3.146120232559066537E-19, -0.9999697198139514409 ) ) ;
#37039 = EDGE_CURVE ( 'NONE', #43487, #27671, #46342, .T. ) ;
#37040 = LINE ( 'NONE', #28502, #42233 ) ;
#37041 = EDGE_CURVE ( 'NONE', #47084, #32426, #31786, .T. ) ;
#37042 = CARTESIAN_POINT ( 'NONE',  ( -20.54204810873173415, 0.000000000000000000, 4.860550213503115558 ) ) ;
#37043 = CARTESIAN_POINT ( 'NONE',  ( -70.06496498987883115, 0.1329914806336913169, 7.577667541101601678 ) ) ;
#37044 = ORIENTED_EDGE ( 'NONE', *, *, #45554, .T. ) ;
#37045 = EDGE_CURVE ( 'NONE', #54483, #13455, #1395, .T. ) ;
#37046 = VERTEX_POINT ( 'NONE', #48547 ) ;
#37047 = DIRECTION ( 'NONE',  ( 0.9999697198139515519, 0.000000000000000000, 0.007781995580013368816 ) ) ;
#37048 = DIRECTION ( 'NONE',  ( 0.5364919789714477361, 0.6444004775717706579, 0.5449076811759711036 ) ) ;
#37049 = LINE ( 'NONE', #38144, #6140 ) ;
#37050 = EDGE_CURVE ( 'NONE', #52840, #23668, #30932, .T. ) ;
#37051 = CARTESIAN_POINT ( 'NONE',  ( -16.29195844028956230, 0.000000000000000000, 8.017607966079944859 ) ) ;
#37052 = VECTOR ( 'NONE', #19972, 1000.000000000000227 ) ;
#37053 = CARTESIAN_POINT ( 'NONE',  ( -28.93137873341882127, 0.000000000000000000, 8.119251130998824451 ) ) ;
#37054 = EDGE_CURVE ( 'NONE', #20652, #50912, #34940, .T. ) ;
#37055 = CARTESIAN_POINT ( 'NONE',  ( -15.88130887279446490, 0.000000000000000000, 3.050160814894388839 ) ) ;
#37056 = ORIENTED_EDGE ( 'NONE', *, *, #38227, .F. ) ;
#37057 = DIRECTION ( 'NONE',  ( -0.9999697198139514409, -0.000000000000000000, -0.007781995580013368816 ) ) ;
#37058 = CARTESIAN_POINT ( 'NONE',  ( -14.94760462649100496, 0.000000000000000000, 2.488088991209854051 ) ) ;
#37059 = LINE ( 'NONE', #33614, #16046 ) ;
#37060 = ORIENTED_EDGE ( 'NONE', *, *, #51370, .F. ) ;
#37061 = CARTESIAN_POINT ( 'NONE',  ( -11.09304826722767956, 24.43504809471621542, -3.000000000000000000 ) ) ;
#37062 = DIRECTION ( 'NONE',  ( 0.000000000000000000, -1.000000000000000000, 0.000000000000000000 ) ) ;
#37063 = CARTESIAN_POINT ( 'NONE',  ( -9.808144436391993182, 0.000000000000000000, 10.77986332834118777 ) ) ;
#37064 = ORIENTED_EDGE ( 'NONE', *, *, #3203, .T. ) ;
#37065 = DIRECTION ( 'NONE',  ( 0.5364919789714477361, 0.6444004775717706579, 0.5449076811759711036 ) ) ;
#37066 = ORIENTED_EDGE ( 'NONE', *, *, #38407, .T. ) ;
#37067 = VERTEX_POINT ( 'NONE', #13366 ) ;
#37068 = EDGE_LOOP ( 'NONE', ( #9062, #12192, #26959, #33511 ) ) ;
#37069 = EDGE_LOOP ( 'NONE', ( #28106, #12902, #5422, #39080 ) ) ;
#37070 = VERTEX_POINT ( 'NONE', #48240 ) ;
#37071 = CARTESIAN_POINT ( 'NONE',  ( -24.24107053542677548, 18.66268724680757884, 4.531816173043640816 ) ) ;
#37072 = ORIENTED_EDGE ( 'NONE', *, *, #51923, .T. ) ;
#37073 = ADVANCED_FACE ( 'NONE', ( #43702 ), #22142, .F. ) ;
#37074 = ORIENTED_EDGE ( 'NONE', *, *, #55716, .T. ) ;
#37075 = CARTESIAN_POINT ( 'NONE',  ( -27.13182803479460858, 16.99370762638562127, 4.657392947539034544 ) ) ;
#37076 = ORIENTED_EDGE ( 'NONE', *, *, #9900, .T. ) ;
#37077 = EDGE_LOOP ( 'NONE', ( #4484, #31760, #23724, #48306 ) ) ;
#37078 = EDGE_CURVE ( 'NONE', #10313, #29764, #35227, .T. ) ;
#37079 = EDGE_CURVE ( 'NONE', #49166, #53648, #39756, .T. ) ;
#37080 = ORIENTED_EDGE ( 'NONE', *, *, #33655, .T. ) ;
#37081 = DIRECTION ( 'NONE',  ( 0.9999697198139515519, 0.000000000000000000, 0.007781995580013368816 ) ) ;
#37082 = CARTESIAN_POINT ( 'NONE',  ( -23.33849165029409889, 0.000000000000000000, 5.946783852668351855 ) ) ;
#37083 = DIRECTION ( 'NONE',  ( -0.7886751345948130876, 0.2113248654051844977, 0.5773502691896263972 ) ) ;
#37084 = DIRECTION ( 'NONE',  ( -0.9999697198139514409, -0.000000000000000000, -0.007781995580013368816 ) ) ;
#37085 = ORIENTED_EDGE ( 'NONE', *, *, #20903, .F. ) ;
#37086 = DIRECTION ( 'NONE',  ( -0.5449076811759708816, 0.6444004775717707689, 0.5364919789714475140 ) ) ;
#37087 = ORIENTED_EDGE ( 'NONE', *, *, #30959, .F. ) ;
#37088 = AXIS2_PLACEMENT_3D ( 'NONE', #12864, #35298, #17976 ) ;
#37089 = ORIENTED_EDGE ( 'NONE', *, *, #11894, .T. ) ;
#37090 = CARTESIAN_POINT ( 'NONE',  ( -11.87243407472968926, 0.000000000000000000, 11.50246268866867361 ) ) ;
#37091 = CARTESIAN_POINT ( 'NONE',  ( -17.38961158937641471, 0.000000000000000000, 3.946413007592513456 ) ) ;
#37092 = UNCERTAINTY_MEASURE_WITH_UNIT (LENGTH_MEASURE( 1.000000000000000082E-05 ), #3551, 'distance_accuracy_value', 'NONE');
#37093 = EDGE_CURVE ( 'NONE', #37968, #43469, #22701, .T. ) ;
#37094 = CARTESIAN_POINT ( 'NONE',  ( 2.602374448188125350E-16, -1.000000000000000000, -2.125000000000000000 ) ) ;
#37095 = DIRECTION ( 'NONE',  ( 0.007781995580012663651, -3.146120232559066537E-19, -0.9999697198139514409 ) ) ;
#37096 = CARTESIAN_POINT ( 'NONE',  ( -15.32244789753343461, 0.000000000000000000, 2.854503944007263261 ) ) ;
#37097 = LINE ( 'NONE', #54394, #13205 ) ;
#37098 = ORIENTED_EDGE ( 'NONE', *, *, #27903, .F. ) ;
#37099 = DIRECTION ( 'NONE',  ( 0.000000000000000000, -1.000000000000000000, 0.000000000000000000 ) ) ;
#37100 = ORIENTED_EDGE ( 'NONE', *, *, #26105, .F. ) ;
#37101 = PLANE ( 'NONE',  #14762 ) ;
#37102 = DIRECTION ( 'NONE',  ( 0.007781995580012662783, 0.000000000000000000, -0.9999697198139514409 ) ) ;
#37103 = CARTESIAN_POINT ( 'NONE',  ( -14.94838282604900748, -0.1191753592594197858, 2.588085963191248506 ) ) ;
#37104 = PLANE ( 'NONE',  #53982 ) ;
#37105 = LINE ( 'NONE', #14679, #50433 ) ;
#37106 = EDGE_LOOP ( 'NONE', ( #36305, #35748, #26668, #35137 ) ) ;
#37107 = FACE_OUTER_BOUND ( 'NONE', #6683, .T. ) ;
#37108 = PLANE ( 'NONE',  #43952 ) ;
#37109 = CARTESIAN_POINT ( 'NONE',  ( -16.69548912546022734, -0.5179957512181551094, 4.017145964781438039 ) ) ;
#37110 = DIRECTION ( 'NONE',  ( 0.000000000000000000, -0.000000000000000000, -1.000000000000000000 ) ) ;
#37111 = EDGE_CURVE ( 'NONE', #40689, #21263, #45384, .T. ) ;
#37112 = DIRECTION ( 'NONE',  ( -0.6427681459581293666, -0.7660444431189770143, -0.005002170337467561935 ) ) ;
#37113 = LINE ( 'NONE', #41905, #44497 ) ;
#37114 = LINE ( 'NONE', #36283, #36518 ) ;
#37115 = DIRECTION ( 'NONE',  ( 0.007781995580012662783, 0.000000000000000000, -0.9999697198139514409 ) ) ;
#37116 = DIRECTION ( 'NONE',  ( 0.9999697198139515519, 0.000000000000000000, 0.007781995580013368816 ) ) ;
#37117 = EDGE_LOOP ( 'NONE', ( #28837, #4847, #2251, #27963 ) ) ;
#37118 = ADVANCED_FACE ( 'NONE', ( #1677 ), #36602, .F. ) ;
#37119 = EDGE_LOOP ( 'NONE', ( #7346, #2974, #35519, #51073 ) ) ;
#37120 = ADVANCED_FACE ( 'NONE', ( #3297 ), #28079, .F. ) ;
#37121 = EDGE_CURVE ( 'NONE', #46316, #2289, #29717, .T. ) ;
#37122 = VERTEX_POINT ( 'NONE', #51276 ) ;
#37123 = ORIENTED_EDGE ( 'NONE', *, *, #32826, .T. ) ;
#37124 = ORIENTED_EDGE ( 'NONE', *, *, #10, .T. ) ;
#37125 = VERTEX_POINT ( 'NONE', #19003 ) ;
#37126 = PLANE ( 'NONE',  #35995 ) ;
#37127 = DIRECTION ( 'NONE',  ( -0.5364919789714478471, 0.6444004775717705469, -0.5449076811759709926 ) ) ;
#37128 = ADVANCED_FACE ( 'NONE', ( #40603 ), #19565, .F. ) ;
#37129 = DIRECTION ( 'NONE',  ( -0.9999697198139514409, -0.000000000000000000, -0.007781995580013368816 ) ) ;
#37131 = ADVANCED_FACE ( 'NONE', ( #55243 ), #12392, .F. ) ;
#37130 = VERTEX_POINT ( 'NONE', #11023 ) ;
#37132 = LINE ( 'NONE', #32860, #19513 ) ;
#37133 = ORIENTED_EDGE ( 'NONE', *, *, #2855, .T. ) ;
#37134 = VERTEX_POINT ( 'NONE', #7542 ) ;
#37135 = EDGE_CURVE ( 'NONE', #52707, #27279, #1935, .T. ) ;
#37136 = CARTESIAN_POINT ( 'NONE',  ( -66.63077082645354210, -8.730603027686937523, 1.362417606690507377 ) ) ;
#37137 = DIRECTION ( 'NONE',  ( -0.9999697198139514409, -0.000000000000000000, -0.007781995580013368816 ) ) ;
#37138 = LINE ( 'NONE', #40837, #30504 ) ;
#37139 = ORIENTED_EDGE ( 'NONE', *, *, #37093, .F. ) ;
#37140 = CARTESIAN_POINT ( 'NONE',  ( -21.47419595591918906, 0.000000000000000000, 5.222628093224860102 ) ) ;
#37141 = ORIENTED_EDGE ( 'NONE', *, *, #23561, .T. ) ;
#37142 = EDGE_CURVE ( 'NONE', #21011, #34747, #36321, .T. ) ;
#37143 = DIRECTION ( 'NONE',  ( -0.5449076811759708816, 0.6444004775717707689, 0.5364919789714475140 ) ) ;
#37144 = DIRECTION ( 'NONE',  ( 0.5449076811759707706, 0.6444004775717708799, -0.5364919789714476250 ) ) ;
#37145 = EDGE_CURVE ( 'NONE', #931, #10342, #41138, .T. ) ;
#37146 = CARTESIAN_POINT ( 'NONE',  ( -18.79634312187524614, 5.467268677019011314, 13.15517843894362038 ) ) ;
#37147 = CARTESIAN_POINT ( 'NONE',  ( -16.27627051837387029, 0.000000000000000000, 6.001743690496146755 ) ) ;
#37148 = CARTESIAN_POINT ( 'NONE',  ( -15.88053067323646417, -0.1191753592594197858, 2.950163842912994383 ) ) ;
#37149 = DIRECTION ( 'NONE',  ( -0.9999697198139514409, -0.000000000000000000, -0.007781995580013368816 ) ) ;
#37150 = DIRECTION ( 'NONE',  ( 0.6427681459581294776, -0.7660444431189769032, 0.005002170337467562802 ) ) ;
#37151 = CARTESIAN_POINT ( 'NONE',  ( -10.77685410066197846, -0.1191753592594185784, 2.989881834110746262 ) ) ;
#37152 = ORIENTED_EDGE ( 'NONE', *, *, #2456, .T. ) ;
#37153 = DIRECTION ( 'NONE',  ( 0.9659258262890682012, -0.2588190451025213501, 0.000000000000000000 ) ) ;
#37154 = ORIENTED_EDGE ( 'NONE', *, *, #17735, .T. ) ;
#37155 = CARTESIAN_POINT ( 'NONE',  ( -27.13182931993292257, 16.99370688441070953, 4.657440554554202805 ) ) ;
#37156 = CARTESIAN_POINT ( 'NONE',  ( -21.20448354515064437, 2.876837460659008361, 4.826687070827041737 ) ) ;
#37157 = CARTESIAN_POINT ( 'NONE',  ( -15.55914933374884512, -2.460819163488158878, 6.764257206824528801 ) ) ;
#37158 = CARTESIAN_POINT ( 'NONE',  ( -10.84028925556084388, -0.1191753592594197858, 11.14116300850493246 ) ) ;
#37159 = CARTESIAN_POINT ( 'NONE',  ( -14.86068505419763142, 0.000000000000000000, 3.227429559033034856 ) ) ;
#37160 = DIRECTION ( 'NONE',  ( -0.005002170337468016433, -0.7660444431189770143, 0.6427681459581293666 ) ) ;
#37161 = DIRECTION ( 'NONE',  ( 1.000000000000000000, 0.000000000000000000, 0.000000000000000000 ) ) ;
#37162 = ORIENTED_EDGE ( 'NONE', *, *, #6055, .T. ) ;
#37163 = DIRECTION ( 'NONE',  ( -0.7660212471507179544, -0.6427876096865405842, -0.005961354470445141482 ) ) ;
#37164 = DIRECTION ( 'NONE',  ( 0.000000000000000000, -1.000000000000000000, 0.000000000000000000 ) ) ;
#37165 = CARTESIAN_POINT ( 'NONE',  ( -19.60834386242827776, 0.000000000000000000, 4.298478389818581213 ) ) ;
#37166 = DIRECTION ( 'NONE',  ( -0.005961354470445682716, -0.6427876096865404731, 0.7660212471507180654 ) ) ;
#37167 = FACE_OUTER_BOUND ( 'NONE', #15951, .T. ) ;
#37168 = CARTESIAN_POINT ( 'NONE',  ( -20.54126990917373519, -0.1191753592594197858, 4.760553241521720658 ) ) ;
#37169 = EDGE_CURVE ( 'NONE', #4596, #26120, #24867, .T. ) ;
#37170 = DIRECTION ( 'NONE',  ( -0.9999697198139514409, -0.000000000000000000, -0.007781995580013368816 ) ) ;
#37171 = LINE ( 'NONE', #16156, #48700 ) ;
#37172 = PLANE ( 'NONE',  #17491 ) ;
#37173 = ORIENTED_EDGE ( 'NONE', *, *, #46483, .F. ) ;
#37174 = CARTESIAN_POINT ( 'NONE',  ( -8.609916609573598834, 0.000000000000000000, 10.23519010964256637 ) ) ;
#37175 = ORIENTED_EDGE ( 'NONE', *, *, #37894, .T. ) ;
#37176 = DIRECTION ( 'NONE',  ( 0.9999697198139515519, 0.000000000000000000, 0.007781995580013368816 ) ) ;
#37177 = PLANE ( 'NONE',  #50968 ) ;
#37178 = ADVANCED_FACE ( 'NONE', ( #10501 ), #15304, .F. ) ;
#37179 = ORIENTED_EDGE ( 'NONE', *, *, #50789, .F. ) ;
#37180 = ORIENTED_EDGE ( 'NONE', *, *, #36647, .T. ) ;
#37181 = PLANE ( 'NONE',  #51090 ) ;
#37182 = EDGE_CURVE ( 'NONE', #8945, #7825, #31509, .T. ) ;
#37183 = VECTOR ( 'NONE', #3301, 1000.000000000000114 ) ;
#37184 = EDGE_LOOP ( 'NONE', ( #50238, #36200, #28310, #37656 ) ) ;
#37185 = VERTEX_POINT ( 'NONE', #19266 ) ;
#37186 = ORIENTED_EDGE ( 'NONE', *, *, #797, .F. ) ;
#37187 = CARTESIAN_POINT ( 'NONE',  ( -19.32961685222932147, 0.000000000000000000, 14.39908572644263351 ) ) ;
#37188 = DIRECTION ( 'NONE',  ( -0.7660212471507179544, -0.6427876096865405842, -0.005961354470445141482 ) ) ;
#37189 = CARTESIAN_POINT ( 'NONE',  ( -18.66354898467281132, 0.000000000000000000, 14.21960318569776582 ) ) ;
#37190 = EDGE_CURVE ( 'NONE', #13455, #22275, #20874, .T. ) ;
#37191 = EDGE_LOOP ( 'NONE', ( #17928, #17171, #13536, #7255 ) ) ;
#37192 = ORIENTED_EDGE ( 'NONE', *, *, #29814, .T. ) ;
#37193 = EDGE_CURVE ( 'NONE', #36955, #34381, #6238, .T. ) ;
#37194 = CARTESIAN_POINT ( 'NONE',  ( -67.13303327250461905, 2.471980953266950741E-14, 6.321089406856109427 ) ) ;
#37195 = DIRECTION ( 'NONE',  ( -0.005961354470445682716, -0.6427876096865404731, 0.7660212471507180654 ) ) ;
#37196 = ORIENTED_EDGE ( 'NONE', *, *, #39955, .F. ) ;
#37197 = DIRECTION ( 'NONE',  ( 0.9999697198139515519, 0.000000000000000000, 0.007781995580013368816 ) ) ;
#37198 = EDGE_LOOP ( 'NONE', ( #55917, #39234, #23112, #47006 ) ) ;
#37199 = DIRECTION ( 'NONE',  ( -0.6427681459581293666, -0.7660444431189770143, -0.005002170337467561935 ) ) ;
#37200 = CARTESIAN_POINT ( 'NONE',  ( -28.92982233430281980, 0.000000000000000000, 7.919257187036034651 ) ) ;
#37201 = EDGE_CURVE ( 'NONE', #23095, #29543, #10770, .T. ) ;
#37202 = ORIENTED_EDGE ( 'NONE', *, *, #43715, .T. ) ;
#37203 = ADVANCED_FACE ( 'NONE', ( #2223 ), #36903, .F. ) ;
#37204 = DIRECTION ( 'NONE',  ( 0.005961354470445682716, -0.6427876096865404731, -0.7660212471507180654 ) ) ;
#37205 = ORIENTED_EDGE ( 'NONE', *, *, #47305, .F. ) ;
#37206 = LINE ( 'NONE', #10822, #31277 ) ;
#37207 =( NAMED_UNIT ( * ) PLANE_ANGLE_UNIT ( ) SI_UNIT ( $, .RADIAN. ) );
#37208 = CARTESIAN_POINT ( 'NONE',  ( -10.14636587563368764, 0.2096447517685606221, 0.8722069013983897445 ) ) ;
#37209 = ORIENTED_EDGE ( 'NONE', *, *, #56074, .F. ) ;
#37210 = CARTESIAN_POINT ( 'NONE',  ( -13.57617169572962190, -0.1191753592594188005, 4.445425176533747802 ) ) ;
#37211 = DIRECTION ( 'NONE',  ( 0.007781995580012663651, 0.000000000000000000, -0.9999697198139515519 ) ) ;
#37212 = PLANE ( 'NONE',  #24019 ) ;
#37213 = DIRECTION ( 'NONE',  ( 0.000000000000000000, -1.000000000000000000, 0.000000000000000000 ) ) ;
#37214 = CARTESIAN_POINT ( 'NONE',  ( -20.39737380963304858, -0.1191753592594195638, 5.131005144047771971 ) ) ;
#37215 = CARTESIAN_POINT ( 'NONE',  ( -10.90796677398788006, 0.6102101463440047224, 0.8994875641494844976 ) ) ;
#37216 = VECTOR ( 'NONE', #45460, 1000.000000000000114 ) ;
#37217 = DIRECTION ( 'NONE',  ( 0.000000000000000000, -1.000000000000000000, 0.000000000000000000 ) ) ;
#37218 = ORIENTED_EDGE ( 'NONE', *, *, #28711, .T. ) ;
#37219 = PLANE ( 'NONE',  #24082 ) ;
#37220 = CARTESIAN_POINT ( 'NONE',  ( -65.61040098691356093, 2.602085213965210642E-15, 0.7610157271807490575 ) ) ;
#37221 = EDGE_LOOP ( 'NONE', ( #11739, #38892, #2748, #16813 ) ) ;
#37222 = CARTESIAN_POINT ( 'NONE',  ( -14.01206388602242292, 3.686347215771508257, 8.374006385476546299 ) ) ;
#37223 = DIRECTION ( 'NONE',  ( -0.5449076811759708816, 0.6444004775717707689, 0.5364919789714475140 ) ) ;
#37224 = LINE ( 'NONE', #41219, #8640 ) ;
#37225 = EDGE_CURVE ( 'NONE', #12737, #30623, #43578, .T. ) ;
#37226 = DIRECTION ( 'NONE',  ( 0.007781995580012663651, -3.146120232559066537E-19, -0.9999697198139514409 ) ) ;
#37227 = CARTESIAN_POINT ( 'NONE',  ( -56.73047118268372202, 6.245764598936942136, 2.439786402985463898 ) ) ;
#37228 = VERTEX_POINT ( 'NONE', #21736 ) ;
#37229 = EDGE_CURVE ( 'NONE', #37046, #10112, #13499, .T. ) ;
#37230 = ORIENTED_EDGE ( 'NONE', *, *, #6851, .T. ) ;
#37231 = ADVANCED_FACE ( 'NONE', ( #48116 ), #34503, .T. ) ;
#37232 = CARTESIAN_POINT ( 'NONE',  ( -21.03231001138954070, 4.333955019861511992, 4.713319344289897295 ) ) ;
#37233 = EDGE_CURVE ( 'NONE', #15067, #52765, #4143, .T. ) ;
#37234 = EDGE_CURVE ( 'NONE', #41830, #37629, #4426, .T. ) ;
#37235 = EDGE_CURVE ( 'NONE', #38019, #12500, #39046, .T. ) ;
#37236 = LINE ( 'NONE', #42618, #19350 ) ;
#37237 = CARTESIAN_POINT ( 'NONE',  ( -14.48966086313376600, -0.1191753592594185784, 2.409902774531527569 ) ) ;
#37238 = AXIS2_PLACEMENT_3D ( 'NONE', #54245, #15598, #36945 ) ;
#37239 = VERTEX_POINT ( 'NONE', #12926 ) ;
#37240 = CARTESIAN_POINT ( 'NONE',  ( -11.87243407472968926, 0.000000000000000000, 11.50246268866867361 ) ) ;
#37241 = ORIENTED_EDGE ( 'NONE', *, *, #37329, .T. ) ;
#37242 = DIRECTION ( 'NONE',  ( 0.005961354470445682716, -0.6427876096865404731, -0.7660212471507180654 ) ) ;
#37243 = ORIENTED_EDGE ( 'NONE', *, *, #24319, .F. ) ;
#37244 = ORIENTED_EDGE ( 'NONE', *, *, #7547, .F. ) ;
#37245 = CARTESIAN_POINT ( 'NONE',  ( -16.33317936670417225, 0.000000000000000000, 13.31440848639340224 ) ) ;
#37246 = PLANE ( 'NONE',  #42287 ) ;
#37247 = CARTESIAN_POINT ( 'NONE',  ( -19.60834386242827776, 0.000000000000000000, 4.298478389818581213 ) ) ;
#37248 = ORIENTED_EDGE ( 'NONE', *, *, #44450, .T. ) ;
#37250 = CARTESIAN_POINT ( 'NONE',  ( -16.11636885593316393, -5.375054281893166142, 2.969973721925023291 ) ) ;
#37249 = VECTOR ( 'NONE', #27881, 1000.000000000000000 ) ;
#37251 = EDGE_CURVE ( 'NONE', #15218, #54860, #54853, .T. ) ;
#37252 = VERTEX_POINT ( 'NONE', #4683 ) ;
#37253 = VECTOR ( 'NONE', #1051, 999.9999999999998863 ) ;
#37255 = VERTEX_POINT ( 'NONE', #17187 ) ;
#37254 = ADVANCED_FACE ( 'NONE', ( #26017 ), #38486, .F. ) ;
#37256 = ORIENTED_EDGE ( 'NONE', *, *, #39615, .T. ) ;
#37257 = PLANE ( 'NONE',  #14124 ) ;
#37258 = EDGE_CURVE ( 'NONE', #52840, #28798, #25425, .T. ) ;
#37259 = ORIENTED_EDGE ( 'NONE', *, *, #37646, .F. ) ;
#37260 = CARTESIAN_POINT ( 'NONE',  ( -12.26136140309277778, 0.000000000000000000, 1.770329817494030955 ) ) ;
#37261 = ORIENTED_EDGE ( 'NONE', *, *, #46582, .F. ) ;
#37262 = PLANE ( 'NONE',  #48506 ) ;
#37263 = PLANE ( 'NONE',  #25002 ) ;
#37264 = EDGE_CURVE ( 'NONE', #13853, #39622, #48543, .T. ) ;
#37265 = ORIENTED_EDGE ( 'NONE', *, *, #20942, .T. ) ;
#37266 = FACE_OUTER_BOUND ( 'NONE', #39785, .T. ) ;
#37267 = ORIENTED_EDGE ( 'NONE', *, *, #50732, .T. ) ;
#37268 = CARTESIAN_POINT ( 'NONE',  ( -15.82531159426634915, 4.172053068839010059, 9.875459425361245991 ) ) ;
#37269 = PLANE ( 'NONE',  #36583 ) ;
#37270 = DIRECTION ( 'NONE',  ( 0.7660212471507180654, -0.6427876096865404731, 0.005961354470445141482 ) ) ;
#37271 = CARTESIAN_POINT ( 'NONE',  ( -15.47205284714705442, -0.1191753592594190225, 9.228244334622088374 ) ) ;
#37272 = CARTESIAN_POINT ( 'NONE',  ( -18.42457910756102990, 0.000000000000000000, 3.938358651053141202 ) ) ;
#37273 = LINE ( 'NONE', #46639, #50030 ) ;
#37274 = ORIENTED_EDGE ( 'NONE', *, *, #28455, .T. ) ;
#37275 = VECTOR ( 'NONE', #8194, 1000.000000000000227 ) ;
#37276 = ORIENTED_EDGE ( 'NONE', *, *, #25121, .T. ) ;
#37277 = VECTOR ( 'NONE', #28908, 1000.000000000000114 ) ;
#37278 = CARTESIAN_POINT ( 'NONE',  ( -56.72378334990722237, 4.325356880459150233, 2.436518382942996830 ) ) ;
#37279 = DIRECTION ( 'NONE',  ( 0.007781995580012663651, 0.000000000000000000, -0.9999697198139515519 ) ) ;
#37280 = CARTESIAN_POINT ( 'NONE',  ( -20.91587874690506155, 3.038739411681507185, 9.992847796181067110 ) ) ;
#37281 = CARTESIAN_POINT ( 'NONE',  ( -9.505154610604371612, 0.000000000000000000, 5.854432023937497398 ) ) ;
#37282 = CARTESIAN_POINT ( 'NONE',  ( 2.072287782118878319, 0.000000000000000000, -2.950529333540147015 ) ) ;
#37283 = VERTEX_POINT ( 'NONE', #712 ) ;
#37284 = DIRECTION ( 'NONE',  ( 0.9999697198139515519, 0.000000000000000000, 0.007781995580013368816 ) ) ;
#37285 = DIRECTION ( 'NONE',  ( 0.000000000000000000, -1.000000000000000000, 0.000000000000000000 ) ) ;
#37286 = ORIENTED_EDGE ( 'NONE', *, *, #26353, .F. ) ;
#37287 = DIRECTION ( 'NONE',  ( 0.6427681459581294776, -0.7660444431189769032, 0.005002170337467562802 ) ) ;
#37288 = DIRECTION ( 'NONE',  ( -0.005002170337468016433, -0.7660444431189770143, 0.6427681459581293666 ) ) ;
#37289 = ORIENTED_EDGE ( 'NONE', *, *, #2448, .F. ) ;
#37290 = CARTESIAN_POINT ( 'NONE',  ( -67.11631774061213207, 2.000000000000002220, 0.4315550088921883409 ) ) ;
#37291 = CARTESIAN_POINT ( 'NONE',  ( -17.33062956602698179, -0.1191753592594162470, 9.217524024740605171 ) ) ;
#37292 = DIRECTION ( 'NONE',  ( 0.005961354470445682716, -0.6427876096865404731, -0.7660212471507180654 ) ) ;
#37293 = DIRECTION ( 'NONE',  ( 0.000000000000000000, -1.000000000000000000, 0.000000000000000000 ) ) ;
#37294 = VECTOR ( 'NONE', #11905, 999.9999999999998863 ) ;
#37295 = CARTESIAN_POINT ( 'NONE',  ( -13.27065584551087163, 0.000000000000000000, 12.04557950825129176 ) ) ;
#37296 = VERTEX_POINT ( 'NONE', #39332 ) ;
#37297 = ORIENTED_EDGE ( 'NONE', *, *, #46164, .F. ) ;
#37298 = PLANE ( 'NONE',  #53866 ) ;
#37299 = FACE_OUTER_BOUND ( 'NONE', #35817, .T. ) ;
#37300 = DIRECTION ( 'NONE',  ( -0.6427681459581293666, -0.7660444431189770143, -0.005002170337467561935 ) ) ;
#37301 = EDGE_CURVE ( 'NONE', #23151, #29528, #18033, .T. ) ;
#37302 = ADVANCED_FACE ( 'NONE', ( #42733 ), #34253, .F. ) ;
#37303 = PLANE ( 'NONE',  #22080 ) ;
#37304 = LINE ( 'NONE', #46675, #9275 ) ;
#37305 = CARTESIAN_POINT ( 'NONE',  ( -25.20278734466900517, 0.000000000000000000, 6.670939612111840944 ) ) ;
#37307 = EDGE_CURVE ( 'NONE', #37711, #31703, #47864, .T. ) ;
#37306 = EDGE_LOOP ( 'NONE', ( #32187, #33545, #51452, #10750 ) ) ;
#37308 = DIRECTION ( 'NONE',  ( 0.000000000000000000, -1.000000000000000000, 0.000000000000000000 ) ) ;
#37309 = DIRECTION ( 'NONE',  ( -0.6246952433987894571, 0.7422098413412802076, 0.2426528472758539834 ) ) ;
#37310 = DIRECTION ( 'NONE',  ( 0.005002170337468016433, -0.7660444431189770143, -0.6427681459581293666 ) ) ;
#37311 = EDGE_LOOP ( 'NONE', ( #37461, #31523, #21618, #27137 ) ) ;
#37312 = CARTESIAN_POINT ( 'NONE',  ( -23.33849165029409889, 0.000000000000000000, 5.946783852668351855 ) ) ;
#37313 = PLANE ( 'NONE',  #51286 ) ;
#37314 = EDGE_CURVE ( 'NONE', #883, #11534, #26269, .T. ) ;
#37315 = CARTESIAN_POINT ( 'NONE',  ( -11.34070976992645363, 0.000000000000000000, 2.885490750803344273 ) ) ;
#37316 = ORIENTED_EDGE ( 'NONE', *, *, #52884, .T. ) ;
#37317 = VECTOR ( 'NONE', #38577, 1000.000000000000227 ) ;
#37318 = VECTOR ( 'NONE', #47784, 999.9999999999998863 ) ;
#37319 = DIRECTION ( 'NONE',  ( 0.005961354470445682716, -0.6427876096865404731, -0.7660212471507180654 ) ) ;
#37320 = ORIENTED_EDGE ( 'NONE', *, *, #31514, .F. ) ;
#37321 = ORIENTED_EDGE ( 'NONE', *, *, #50261, .F. ) ;
#37322 = ORIENTED_EDGE ( 'NONE', *, *, #16958, .F. ) ;
#37323 = VERTEX_POINT ( 'NONE', #3832 ) ;
#37324 = VECTOR ( 'NONE', #2634, 1000.000000000000227 ) ;
#37325 = ADVANCED_FACE ( 'NONE', ( #21162 ), #17763, .F. ) ;
#37326 = ORIENTED_EDGE ( 'NONE', *, *, #5368, .F. ) ;
#37327 = CARTESIAN_POINT ( 'NONE',  ( -12.49980730458054978, 0.2864062442990030766, 1.528143525138426773 ) ) ;
#37328 = VERTEX_POINT ( 'NONE', #29971 ) ;
#37329 = EDGE_CURVE ( 'NONE', #23582, #31229, #49542, .T. ) ;
#37330 = EDGE_LOOP ( 'NONE', ( #54670, #7107, #40643, #30066, #5430 ) ) ;
#37331 = LINE ( 'NONE', #6163, #7721 ) ;
#37332 = ORIENTED_EDGE ( 'NONE', *, *, #27857, .T. ) ;
#37333 = ORIENTED_EDGE ( 'NONE', *, *, #40626, .F. ) ;
#37334 = ADVANCED_FACE ( 'NONE', ( #36756 ), #19132, .F. ) ;
#37335 = AXIS2_PLACEMENT_3D ( 'NONE', #6622, #24233, #33858 ) ;
#37336 = CARTESIAN_POINT ( 'NONE',  ( -27.99767448711536133, 0.000000000000000000, 7.557179307314289218 ) ) ;
#37337 = LINE ( 'NONE', #41346, #47563 ) ;
#37338 = CARTESIAN_POINT ( 'NONE',  ( -17.18893626679898645, 5.305366725996512933, 3.189429341044820454 ) ) ;
#37339 = LINE ( 'NONE', #50113, #15049 ) ;
#37340 = ORIENTED_EDGE ( 'NONE', *, *, #52194, .T. ) ;
#37341 = LINE ( 'NONE', #41872, #52814 ) ;
#37342 = VERTEX_POINT ( 'NONE', #5269 ) ;
#37343 = VERTEX_POINT ( 'NONE', #45268 ) ;
#37344 = CARTESIAN_POINT ( 'NONE',  ( -16.99924723426068951, 0.000000000000000000, 13.49389102713827171 ) ) ;
#37345 = DIRECTION ( 'NONE',  ( 1.000000000000000000, 0.000000000000000000, 0.000000000000000000 ) ) ;
#37346 = FACE_OUTER_BOUND ( 'NONE', #51643, .T. ) ;
#37347 = DIRECTION ( 'NONE',  ( -0.005002170337468016433, -0.7660444431189770143, 0.6427681459581293666 ) ) ;
#37348 = LINE ( 'NONE', #50131, #18619 ) ;
#37349 = PLANE ( 'NONE',  #37686 ) ;
#37350 = ORIENTED_EDGE ( 'NONE', *, *, #4761, .F. ) ;
#37351 = CARTESIAN_POINT ( 'NONE',  ( -18.13613576012749817, 0.000000000000000000, 6.156595802719084354 ) ) ;
#37352 = ORIENTED_EDGE ( 'NONE', *, *, #20205, .F. ) ;
#37353 = AXIS2_PLACEMENT_3D ( 'NONE', #11492, #3241, #20266 ) ;
#37354 = VECTOR ( 'NONE', #4474, 1000.000000000000227 ) ;
#37355 = LINE ( 'NONE', #19200, #20165 ) ;
#37356 = DIRECTION ( 'NONE',  ( 0.000000000000000000, -1.000000000000000000, 0.000000000000000000 ) ) ;
#37357 = PLANE ( 'NONE',  #54434 ) ;
#37358 = PLANE ( 'NONE',  #31338 ) ;
#37359 = DIRECTION ( 'NONE',  ( 0.5364919789714477361, 0.6444004775717706579, 0.5449076811759711036 ) ) ;
#37360 = ORIENTED_EDGE ( 'NONE', *, *, #32016, .T. ) ;
#37361 = VECTOR ( 'NONE', #25012, 1000.000000000000227 ) ;
#37362 = EDGE_LOOP ( 'NONE', ( #27187, #29611, #27388, #38225 ) ) ;
#37363 = LINE ( 'NONE', #54683, #21241 ) ;
#37364 = DIRECTION ( 'NONE',  ( 0.000000000000000000, -1.000000000000000000, 0.000000000000000000 ) ) ;
#37365 = LINE ( 'NONE', #28875, #15207 ) ;
#37366 = EDGE_CURVE ( 'NONE', #40739, #14885, #27965, .T. ) ;
#37367 = DIRECTION ( 'NONE',  ( 0.000000000000000000, 0.000000000000000000, 1.000000000000000000 ) ) ;
#37368 = VECTOR ( 'NONE', #17824, 1000.000000000000227 ) ;
#37369 = CARTESIAN_POINT ( 'NONE',  ( 2.072287782118878319, 0.000000000000000000, -2.950529333540147015 ) ) ;
#37370 = EDGE_CURVE ( 'NONE', #44242, #33042, #49240, .T. ) ;
#37371 = LINE ( 'NONE', #10450, #11856 ) ;
#37372 = EDGE_CURVE ( 'NONE', #49975, #9690, #17926, .T. ) ;
#37373 = FACE_OUTER_BOUND ( 'NONE', #2762, .T. ) ;
#37374 = CARTESIAN_POINT ( 'NONE',  ( -69.35974691127840686, -9.648372592778560630, -8.803577518029834792 ) ) ;
#37375 = LINE ( 'NONE', #54695, #39192 ) ;
#37376 = ORIENTED_EDGE ( 'NONE', *, *, #19542, .F. ) ;
#37377 = VECTOR ( 'NONE', #27971, 999.9999999999998863 ) ;
#37378 = VERTEX_POINT ( 'NONE', #6119 ) ;
#37379 = ORIENTED_EDGE ( 'NONE', *, *, #26913, .T. ) ;
#37380 = ORIENTED_EDGE ( 'NONE', *, *, #40793, .F. ) ;
#37381 = ORIENTED_EDGE ( 'NONE', *, *, #9979, .T. ) ;
#37382 = VECTOR ( 'NONE', #13171, 1000.000000000000227 ) ;
#37383 = DIRECTION ( 'NONE',  ( 0.000000000000000000, -1.000000000000000000, 0.000000000000000000 ) ) ;
#37384 = DIRECTION ( 'NONE',  ( 0.000000000000000000, 0.000000000000000000, -1.000000000000000000 ) ) ;
#37385 = LINE ( 'NONE', #15815, #31286 ) ;
#37386 = VECTOR ( 'NONE', #22659, 1000.000000000000227 ) ;
#37387 = VECTOR ( 'NONE', #23340, 1000.000000000000000 ) ;
#37388 = ORIENTED_EDGE ( 'NONE', *, *, #26977, .T. ) ;
#37389 = ORIENTED_EDGE ( 'NONE', *, *, #3283, .F. ) ;
#37390 = ORIENTED_EDGE ( 'NONE', *, *, #52011, .T. ) ;
#37391 = CARTESIAN_POINT ( 'NONE',  ( -64.63669322539915640, -11.11986739470662933, 1.314563741827290189 ) ) ;
#37392 = VERTEX_POINT ( 'NONE', #44697 ) ;
#37393 = EDGE_CURVE ( 'NONE', #44507, #10018, #48401, .T. ) ;
#37394 = AXIS2_PLACEMENT_3D ( 'NONE', #45920, #50990, #29436 ) ;
#37395 = AXIS2_PLACEMENT_3D ( 'NONE', #36838, #18952, #15496 ) ;
#37396 = CARTESIAN_POINT ( 'NONE',  ( -66.56540940824446295, -9.327934164263727013, 6.231849021620877060 ) ) ;
#37397 = EDGE_CURVE ( 'NONE', #23847, #34987, #14891, .T. ) ;
#37398 = LINE ( 'NONE', #53887, #17396 ) ;
#37399 = FACE_OUTER_BOUND ( 'NONE', #1431, .T. ) ;
#37400 = EDGE_CURVE ( 'NONE', #9714, #3202, #23420, .T. ) ;
#37401 = ORIENTED_EDGE ( 'NONE', *, *, #4522, .F. ) ;
#37402 = LINE ( 'NONE', #41664, #52770 ) ;
#37403 = ORIENTED_EDGE ( 'NONE', *, *, #8154, .F. ) ;
#37404 = DIRECTION ( 'NONE',  ( 0.9999697198139515519, 0.000000000000000000, 0.007781995580013368816 ) ) ;
#37405 = EDGE_CURVE ( 'NONE', #12044, #20122, #32219, .T. ) ;
#37406 = VECTOR ( 'NONE', #17440, 999.9999999999998863 ) ;
#37407 = DIRECTION ( 'NONE',  ( -0.005961354470445682716, -0.6427876096865404731, 0.7660212471507180654 ) ) ;
#37408 = DIRECTION ( 'NONE',  ( 0.000000000000000000, -1.000000000000000000, 0.000000000000000000 ) ) ;
#37409 = CARTESIAN_POINT ( 'NONE',  ( -21.10420191512951149, 1.095915999411505526, 4.844554998909636367 ) ) ;
#37410 = DIRECTION ( 'NONE',  ( 0.007781995580012662783, 0.000000000000000000, -0.9999697198139514409 ) ) ;
#37411 = FACE_OUTER_BOUND ( 'NONE', #27009, .T. ) ;
#37412 = DIRECTION ( 'NONE',  ( 0.6427681459581294776, -0.7660444431189769032, 0.005002170337467562802 ) ) ;
#37413 = FACE_OUTER_BOUND ( 'NONE', #34853, .T. ) ;
#37414 = LINE ( 'NONE', #54199, #20199 ) ;
#37415 = ORIENTED_EDGE ( 'NONE', *, *, #24734, .F. ) ;
#37416 = CARTESIAN_POINT ( 'NONE',  ( -18.66354898467281132, 0.000000000000000000, 14.21960318569776582 ) ) ;
#37417 = ORIENTED_EDGE ( 'NONE', *, *, #36036, .T. ) ;
#37418 = VECTOR ( 'NONE', #52160, 1000.000000000000227 ) ;
#37419 = CARTESIAN_POINT ( 'NONE',  ( -10.47421230394850866, 0.000000000000000000, 10.95934586908605723 ) ) ;
#37420 = CARTESIAN_POINT ( 'NONE',  ( -11.77243710274829525, -0.1191753592594197858, 11.50324088822667612 ) ) ;
#37421 = LINE ( 'NONE', #3371, #44096 ) ;
#37422 = VECTOR ( 'NONE', #40322, 1000.000000000000114 ) ;
#37423 = DIRECTION ( 'NONE',  ( -0.5364919789714478471, 0.6444004775717705469, -0.5449076811759709926 ) ) ;
#37424 = CARTESIAN_POINT ( 'NONE',  ( -12.13851405436063047, 0.000000000000000000, 11.68505802764555135 ) ) ;
#37425 = ADVANCED_FACE ( 'NONE', ( #9811 ), #40468, .F. ) ;
#37426 = CARTESIAN_POINT ( 'NONE',  ( -19.22961988024793101, -0.1191753592594177458, 14.39986392600063603 ) ) ;
#37427 = VERTEX_POINT ( 'NONE', #10063 ) ;
#37428 = PLANE ( 'NONE',  #17446 ) ;
#37429 = AXIS2_PLACEMENT_3D ( 'NONE', #55137, #55991, #38086 ) ;
#37430 = FACE_OUTER_BOUND ( 'NONE', #13152, .T. ) ;
#37431 = PLANE ( 'NONE',  #25839 ) ;
#37432 = EDGE_CURVE ( 'NONE', #607, #27671, #28782, .T. ) ;
#37433 = DIRECTION ( 'NONE',  ( 0.9999697198139515519, 0.000000000000000000, 0.007781995580013368816 ) ) ;
#37434 = DIRECTION ( 'NONE',  ( 0.5364919789714477361, 0.6444004775717706579, 0.5449076811759711036 ) ) ;
#37435 = AXIS2_PLACEMENT_3D ( 'NONE', #18314, #15646, #35653 ) ;
#37436 = VECTOR ( 'NONE', #28643, 1000.000000000000227 ) ;
#37437 = EDGE_CURVE ( 'NONE', #48957, #25894, #44419, .T. ) ;
#37438 = DIRECTION ( 'NONE',  ( -0.6427681459581293666, -0.7660444431189770143, -0.005002170337467561935 ) ) ;
#37439 = PLANE ( 'NONE',  #2136 ) ;
#37440 = FACE_OUTER_BOUND ( 'NONE', #29617, .T. ) ;
#37441 = EDGE_CURVE ( 'NONE', #25831, #19083, #52946, .T. ) ;
#37443 = EDGE_CURVE ( 'NONE', #51780, #30062, #5524, .T. ) ;
#37442 = PLANE ( 'NONE',  #15615 ) ;
#37444 = ORIENTED_EDGE ( 'NONE', *, *, #49046, .T. ) ;
#37445 = VECTOR ( 'NONE', #30836, 1000.000000000000227 ) ;
#37446 = LINE ( 'NONE', #24132, #46649 ) ;
#37447 = VECTOR ( 'NONE', #11399, 1000.000000000000227 ) ;
#37448 = LINE ( 'NONE', #24964, #50454 ) ;
#37449 = ORIENTED_EDGE ( 'NONE', *, *, #55248, .F. ) ;
#37450 = CARTESIAN_POINT ( 'NONE',  ( -18.68223532000061482, -0.1166911823299036782, 4.038441074006483333 ) ) ;
#37451 = CARTESIAN_POINT ( 'NONE',  ( -29.86274838104827367, -0.1191753592594197858, 8.381332038739175871 ) ) ;
#37452 = ORIENTED_EDGE ( 'NONE', *, *, #45910, .T. ) ;
#37453 = PRODUCT_DEFINITION ( 'UNKNOWN', '', #49842, #50125 ) ;
#37454 = AXIS2_PLACEMENT_3D ( 'NONE', #1090, #18426, #44833 ) ;
#37455 = ORIENTED_EDGE ( 'NONE', *, *, #17648, .F. ) ;
#37456 = DIRECTION ( 'NONE',  ( -0.005961354470445682716, -0.6427876096865404731, 0.7660212471507180654 ) ) ;
#37457 = VECTOR ( 'NONE', #13799, 1000.000000000000000 ) ;
#37458 = ADVANCED_FACE ( 'NONE', ( #1806 ), #22843, .F. ) ;
#37459 = ORIENTED_EDGE ( 'NONE', *, *, #5717, .F. ) ;
#37460 = ORIENTED_EDGE ( 'NONE', *, *, #10154, .F. ) ;
#37461 = ORIENTED_EDGE ( 'NONE', *, *, #55256, .F. ) ;
#37462 = DIRECTION ( 'NONE',  ( -0.005961354470445682716, -0.6427876096865404731, 0.7660212471507180654 ) ) ;
#37463 = CARTESIAN_POINT ( 'NONE',  ( -13.53673582514181106, 0.000000000000000000, 12.22817484722816772 ) ) ;
#37464 = LINE ( 'NONE', #25267, #29423 ) ;
#37465 = AXIS2_PLACEMENT_3D ( 'NONE', #19112, #40446, #44674 ) ;
#37466 = ORIENTED_EDGE ( 'NONE', *, *, #52111, .F. ) ;
#37467 = ORIENTED_EDGE ( 'NONE', *, *, #56007, .F. ) ;
#37468 = AXIS2_PLACEMENT_3D ( 'NONE', #666, #39275, #44103 ) ;
#37469 = DIRECTION ( 'NONE',  ( 0.000000000000000000, -0.000000000000000000, -1.000000000000000000 ) ) ;
#37470 = DIRECTION ( 'NONE',  ( 0.007781995580012663651, 0.000000000000000000, -0.9999697198139515519 ) ) ;
#37471 = ORIENTED_EDGE ( 'NONE', *, *, #5596, .T. ) ;
#37472 = CIRCLE ( 'NONE', #30241, 2.125000000000000000 ) ;
#37473 = DIRECTION ( 'NONE',  ( 0.6427681459581294776, -0.7660444431189769032, 0.005002170337467562802 ) ) ;
#37474 = VERTEX_POINT ( 'NONE', #36202 ) ;
#37475 = DIRECTION ( 'NONE',  ( -0.5364919789714478471, 0.6444004775717705469, -0.5449076811759709926 ) ) ;
#37476 = CARTESIAN_POINT ( 'NONE',  ( -18.58927644294745107, 0.000000000000000000, 4.675741077920016586 ) ) ;
#37477 = VECTOR ( 'NONE', #23654, 1000.000000000000114 ) ;
#37478 = AXIS2_PLACEMENT_3D ( 'NONE', #52399, #30813, #9220 ) ;
#37479 = ORIENTED_EDGE ( 'NONE', *, *, #22957, .T. ) ;
#37480 = DIRECTION ( 'NONE',  ( -0.7660212471507179544, -0.6427876096865405842, -0.005961354470445141482 ) ) ;
#37481 = EDGE_CURVE ( 'NONE', #9006, #32205, #53258, .T. ) ;
#37482 = AXIS2_PLACEMENT_3D ( 'NONE', #11055, #24145, #15591 ) ;
#37483 = DIRECTION ( 'NONE',  ( -0.005002170337468016433, -0.7660444431189770143, 0.6427681459581293666 ) ) ;
#37484 = AXIS2_PLACEMENT_3D ( 'NONE', #1049, #23754, #11257 ) ;
#37485 = EDGE_LOOP ( 'NONE', ( #35781, #37479, #27932, #20848 ) ) ;
#37486 = CARTESIAN_POINT ( 'NONE',  ( -9.495214795699244092, 0.000000000000000000, 4.577187154869228891 ) ) ;
#37487 = DIRECTION ( 'NONE',  ( 0.2426528472758542054, 0.7422098413412800966, 0.6246952433987894571 ) ) ;
#37488 = DIRECTION ( 'NONE',  ( -0.8531650599175529814, -0.4028455766673920135, 0.3313982828793697877 ) ) ;
#37489 = ORIENTED_EDGE ( 'NONE', *, *, #6975, .F. ) ;
#37490 = ADVANCED_FACE ( 'NONE', ( #36457 ), #53771, .F. ) ;
#37491 = LINE ( 'NONE', #55655, #31044 ) ;
#37492 = PLANE ( 'NONE',  #29625 ) ;
#37493 = CARTESIAN_POINT ( 'NONE',  ( -12.16996096287794060, 0.4483081953215045656, 1.394854484504827852 ) ) ;
#37494 = CARTESIAN_POINT ( 'NONE',  ( -13.07066190154808361, 0.000000000000000000, 12.04713590736729678 ) ) ;
#37495 = ADVANCED_FACE ( 'NONE', ( #55182 ), #28214, .F. ) ;
#37496 = CARTESIAN_POINT ( 'NONE',  ( -17.47832216281435436, -2.189961127332303636, 12.64592903418461667 ) ) ;
#37498 = ADVANCED_FACE ( 'NONE', ( #7775 ), #11473, .F. ) ;
#37497 = DIRECTION ( 'NONE',  ( 0.007781995580012663651, 0.000000000000000000, -0.9999697198139515519 ) ) ;
#37499 = CARTESIAN_POINT ( 'NONE',  ( -69.19091591890759219, -11.64211925634823608, -7.659292557883813579 ) ) ;
#37500 = AXIS2_PLACEMENT_3D ( 'NONE', #51244, #12360, #4941 ) ;
#37501 = ORIENTED_EDGE ( 'NONE', *, *, #44079, .F. ) ;
#37502 = CARTESIAN_POINT ( 'NONE',  ( -18.29747203306047609, -0.1191753592594177458, 14.03778604627889059 ) ) ;
#37503 = CARTESIAN_POINT ( 'NONE',  ( -18.86354292863559579, 0.000000000000000000, 14.21804678658176080 ) ) ;
#37504 = DIRECTION ( 'NONE',  ( 0.000000000000000000, -0.000000000000000000, -1.000000000000000000 ) ) ;
#37505 = ORIENTED_EDGE ( 'NONE', *, *, #12597, .T. ) ;
#37506 = CARTESIAN_POINT ( 'NONE',  ( -9.542064456761055524, 0.000000000000000000, 10.59726798936431180 ) ) ;
#37507 = EDGE_CURVE ( 'NONE', #24035, #19370, #42114, .T. ) ;
#37508 = DIRECTION ( 'NONE',  ( -0.5364919789714478471, 0.6444004775717705469, -0.5449076811759709926 ) ) ;
#37509 = VECTOR ( 'NONE', #16385, 1000.000000000000227 ) ;
#37510 = EDGE_CURVE ( 'NONE', #30294, #16295, #24254, .T. ) ;
#37511 = LINE ( 'NONE', #33535, #14070 ) ;
#37512 = VECTOR ( 'NONE', #21829, 999.9999999999998863 ) ;
#37513 = DIRECTION ( 'NONE',  ( -0.005002170337468016433, -0.7660444431189770143, 0.6427681459581293666 ) ) ;
#37514 = EDGE_CURVE ( 'NONE', #23008, #29351, #20553, .T. ) ;
#37515 = CARTESIAN_POINT ( 'NONE',  ( -56.19049806081029175, 6.779003593249485426, 2.073111974254101320 ) ) ;
#37516 = ORIENTED_EDGE ( 'NONE', *, *, #48619, .T. ) ;
#37517 = ORIENTED_EDGE ( 'NONE', *, *, #41880, .T. ) ;
#37518 = CARTESIAN_POINT ( 'NONE',  ( 2.072287782118878319, 0.000000000000000000, -2.950529333540147015 ) ) ;
#37519 = AXIS2_PLACEMENT_3D ( 'NONE', #41528, #6595, #44956 ) ;
#37520 = VECTOR ( 'NONE', #38627, 999.9999999999998863 ) ;
#37521 = CARTESIAN_POINT ( 'NONE',  ( -27.99923088623136636, 0.000000000000000000, 7.757173251277078130 ) ) ;
#37522 = EDGE_CURVE ( 'NONE', #30961, #32780, #28797, .T. ) ;
#37523 = ORIENTED_EDGE ( 'NONE', *, *, #2846, .T. ) ;
#37524 = DIRECTION ( 'NONE',  ( 0.007781995580012663651, -3.146120232559066537E-19, -0.9999697198139514409 ) ) ;
#37525 = VERTEX_POINT ( 'NONE', #16015 ) ;
#37526 = CARTESIAN_POINT ( 'NONE',  ( -16.33317936670417225, 0.000000000000000000, 13.31440848639340224 ) ) ;
#37527 = ADVANCED_FACE ( 'NONE', ( #16272 ), #2913, .F. ) ;
#37528 = VECTOR ( 'NONE', #53293, 1000.000000000000227 ) ;
#37529 = VERTEX_POINT ( 'NONE', #33591 ) ;
#37530 = VECTOR ( 'NONE', #21172, 1000.000000000000227 ) ;
#37531 = ORIENTED_EDGE ( 'NONE', *, *, #43167, .F. ) ;
#37532 = LINE ( 'NONE', #54851, #48299 ) ;
#37533 = DIRECTION ( 'NONE',  ( 0.6427681459581294776, -0.7660444431189769032, 0.005002170337467562802 ) ) ;
#37534 = LINE ( 'NONE', #42913, #24838 ) ;
#37535 = ORIENTED_EDGE ( 'NONE', *, *, #38186, .F. ) ;
#37536 = CARTESIAN_POINT ( 'NONE',  ( -15.60102546347950536, 0.000000000000000000, 12.95077420755565356 ) ) ;
#37537 = ORIENTED_EDGE ( 'NONE', *, *, #51742, .F. ) ;
#37538 = ORIENTED_EDGE ( 'NONE', *, *, #11740, .F. ) ;
#37539 = ORIENTED_EDGE ( 'NONE', *, *, #33426, .F. ) ;
#37540 = CARTESIAN_POINT ( 'NONE',  ( -12.60458797795435615, 0.000000000000000000, 11.86609696750642229 ) ) ;
#37541 = AXIS2_PLACEMENT_3D ( 'NONE', #19932, #32466, #28174 ) ;
#37542 = DIRECTION ( 'NONE',  ( -0.3313982828793700652, 0.4028455766673916250, -0.8531650599175529814 ) ) ;
#37543 = ORIENTED_EDGE ( 'NONE', *, *, #7293, .T. ) ;
#37544 = CARTESIAN_POINT ( 'NONE',  ( -19.60990026154428278, 0.000000000000000000, 4.498472333781370125 ) ) ;
#37545 = ORIENTED_EDGE ( 'NONE', *, *, #44136, .F. ) ;
#37546 = VECTOR ( 'NONE', #19768, 1000.000000000000227 ) ;
#37547 = DIRECTION ( 'NONE',  ( 0.007781995580012662783, 0.000000000000000000, -0.9999697198139514409 ) ) ;
#37548 = LINE ( 'NONE', #10629, #43135 ) ;
#37549 = ORIENTED_EDGE ( 'NONE', *, *, #19110, .T. ) ;
#37550 = DIRECTION ( 'NONE',  ( 0.000000000000000000, -0.000000000000000000, -1.000000000000000000 ) ) ;
#37551 = EDGE_CURVE ( 'NONE', #27150, #41291, #29342, .T. ) ;
#37552 = AXIS2_PLACEMENT_3D ( 'NONE', #35686, #18650, #45060 ) ;
#37553 = EDGE_LOOP ( 'NONE', ( #20111, #25628, #16829, #26508 ) ) ;
#37554 = DIRECTION ( 'NONE',  ( 0.000000000000000000, -1.000000000000000000, 0.000000000000000000 ) ) ;
#37555 = DIRECTION ( 'NONE',  ( -0.6427681459581293666, -0.7660444431189770143, -0.005002170337467561935 ) ) ;
#37556 = DIRECTION ( 'NONE',  ( -0.005961354470445682716, -0.6427876096865404731, 0.7660212471507180654 ) ) ;
#37557 =( LENGTH_UNIT ( ) NAMED_UNIT ( * ) SI_UNIT ( .MILLI., .METRE. ) );
#37558 = DIRECTION ( 'NONE',  ( -0.2588190451025176864, -0.9659258262890692004, 0.000000000000000000 ) ) ;
#37559 = AXIS2_PLACEMENT_3D ( 'NONE', #16368, #29452, #25207 ) ;
#37560 = DIRECTION ( 'NONE',  ( -0.005002170337468016433, -0.7660444431189770143, 0.6427681459581293666 ) ) ;
#37561 = ORIENTED_EDGE ( 'NONE', *, *, #45231, .F. ) ;
#37562 = ADVANCED_FACE ( 'NONE', ( #45816 ), #42414, .F. ) ;
#37563 = EDGE_CURVE ( 'NONE', #8639, #51306, #7472, .T. ) ;
#37564 = VECTOR ( 'NONE', #24496, 1000.000000000000227 ) ;
#37565 = ORIENTED_EDGE ( 'NONE', *, *, #54137, .F. ) ;
#37566 = CARTESIAN_POINT ( 'NONE',  ( -18.67619601524082285, 0.000000000000000000, 3.936400510096834893 ) ) ;
#37567 = FACE_OUTER_BOUND ( 'NONE', #36089, .T. ) ;
#37568 = CARTESIAN_POINT ( 'NONE',  ( -16.76677389676250485, 0.000000000000000000, 9.321915108048015597 ) ) ;
#37569 = DIRECTION ( 'NONE',  ( -0.9999697198139514409, -0.000000000000000000, -0.007781995580013368816 ) ) ;
#37571 = EDGE_CURVE ( 'NONE', #1588, #24466, #11172, .T. ) ;
#37570 = CARTESIAN_POINT ( 'NONE',  ( -14.76962374716334381, 2.391131607591507446, 6.542598890781153642 ) ) ;
#37572 = VECTOR ( 'NONE', #41904, 999.9999999999998863 ) ;
#37573 = VECTOR ( 'NONE', #7635, 1000.000000000000114 ) ;
#37574 = DIRECTION ( 'NONE',  ( 0.007781995580012662783, 0.000000000000000000, -0.9999697198139514409 ) ) ;
#37575 = ORIENTED_EDGE ( 'NONE', *, *, #49354, .F. ) ;
#37576 = CARTESIAN_POINT ( 'NONE',  ( -9.306717065757585061, 0.000000000000000000, 6.055982367016289558 ) ) ;
#37577 = LINE ( 'NONE', #50901, #7822 ) ;
#37578 = ORIENTED_EDGE ( 'NONE', *, *, #22396, .T. ) ;
#37579 = FACE_OUTER_BOUND ( 'NONE', #51850, .T. ) ;
#37580 = DIRECTION ( 'NONE',  ( -0.5449076811759708816, 0.6444004775717707689, 0.5364919789714475140 ) ) ;
#37581 = ORIENTED_EDGE ( 'NONE', *, *, #15012, .T. ) ;
#37582 = FACE_OUTER_BOUND ( 'NONE', #19586, .T. ) ;
#37583 = PLANE ( 'NONE',  #47796 ) ;
#37584 = EDGE_CURVE ( 'NONE', #52222, #9654, #38132, .T. ) ;
#37585 = CARTESIAN_POINT ( 'NONE',  ( -21.47419595591918906, 0.000000000000000000, 5.222628093224860102 ) ) ;
#37586 = LINE ( 'NONE', #16022, #3291 ) ;
#37587 = EDGE_CURVE ( 'NONE', #12202, #40957, #46655, .T. ) ;
#37588 = DIRECTION ( 'NONE',  ( 0.007781995580012663651, 0.000000000000000000, -0.9999697198139515519 ) ) ;
#37589 = VECTOR ( 'NONE', #49436, 1000.000000000000227 ) ;
#37590 = ORIENTED_EDGE ( 'NONE', *, *, #50534, .F. ) ;
#37591 = ORIENTED_EDGE ( 'NONE', *, *, #4202, .T. ) ;
#37592 = AXIS2_PLACEMENT_3D ( 'NONE', #23037, #39532, #27283 ) ;
#37593 = EDGE_CURVE ( 'NONE', #47675, #6779, #50645, .T. ) ;
#37594 = CARTESIAN_POINT ( 'NONE',  ( -67.02251838831884356, -0.6010030055608566180, -0.3300946888591886896 ) ) ;
#37595 = CARTESIAN_POINT ( 'NONE',  ( -20.53709881633460199, 3.686347215771508257, 10.90855154352876255 ) ) ;
#37596 = CARTESIAN_POINT ( 'NONE',  ( -20.54204810873173415, 0.000000000000000000, 4.860550213503115558 ) ) ;
#37597 = VECTOR ( 'NONE', #36672, 1000.000000000000000 ) ;
#37598 = PLANE ( 'NONE',  #27870 ) ;
#37599 = EDGE_CURVE ( 'NONE', #17866, #15410, #19713, .T. ) ;
#37600 = CARTESIAN_POINT ( 'NONE',  ( -18.35205637073270069, 0.000000000000000000, 8.201581863854691790 ) ) ;
#37601 = CARTESIAN_POINT ( 'NONE',  ( -18.79789254742608406, 0.000000000000000000, 5.782113788577308178 ) ) ;
#37602 = ORIENTED_EDGE ( 'NONE', *, *, #2922, .F. ) ;
#37603 = CARTESIAN_POINT ( 'NONE',  ( -13.50413705924304963, 0.000000000000000000, 8.039303436688003401 ) ) ;
#37604 = CARTESIAN_POINT ( 'NONE',  ( -16.81190032086591302, 0.000000000000000000, 3.212244750653343583 ) ) ;
#37605 = DIRECTION ( 'NONE',  ( 0.000000000000000000, -0.000000000000000000, -1.000000000000000000 ) ) ;
#37607 = VERTEX_POINT ( 'NONE', #32749 ) ;
#37606 = VECTOR ( 'NONE', #6178, 1000.000000000000227 ) ;
#37608 = VECTOR ( 'NONE', #26584, 1000.000000000000227 ) ;
#37609 = CARTESIAN_POINT ( 'NONE',  ( -68.96274401086908767, -10.65449282557018584, 7.493821216008848651 ) ) ;
#37610 = CARTESIAN_POINT ( 'NONE',  ( -16.99924723426068951, 0.000000000000000000, 13.49389102713827171 ) ) ;
#37611 = CARTESIAN_POINT ( 'NONE',  ( -33.59133976979808978, -0.1191753592594197858, 9.829643557626155825 ) ) ;
#37612 = VECTOR ( 'NONE', #17964, 1000.000000000000000 ) ;
#37613 = ORIENTED_EDGE ( 'NONE', *, *, #2880, .T. ) ;
#37614 = FACE_OUTER_BOUND ( 'NONE', #29469, .T. ) ;
#37615 = ORIENTED_EDGE ( 'NONE', *, *, #54801, .T. ) ;
#37616 = AXIS2_PLACEMENT_3D ( 'NONE', #3242, #12338, #4084 ) ;
#37617 = ORIENTED_EDGE ( 'NONE', *, *, #22904, .F. ) ;
#37618 = VECTOR ( 'NONE', #22573, 1000.000000000000227 ) ;
#37619 = EDGE_LOOP ( 'NONE', ( #34879, #14525, #41572, #44466 ) ) ;
#37620 = ORIENTED_EDGE ( 'NONE', *, *, #18337, .F. ) ;
#37621 = FACE_OUTER_BOUND ( 'NONE', #23743, .T. ) ;
#37623 = EDGE_CURVE ( 'NONE', #51697, #55458, #50059, .T. ) ;
#37622 = ORIENTED_EDGE ( 'NONE', *, *, #40133, .F. ) ;
#37624 = ORIENTED_EDGE ( 'NONE', *, *, #16123, .T. ) ;
#37625 = CARTESIAN_POINT ( 'NONE',  ( -15.92694207790892946, 5.467268677019013978, 2.694062420689476767 ) ) ;
#37626 = ORIENTED_EDGE ( 'NONE', *, *, #51522, .F. ) ;
#37627 = ADVANCED_FACE ( 'NONE', ( #29056 ), #46357, .F. ) ;
#37628 = EDGE_CURVE ( 'NONE', #17269, #17866, #8613, .T. ) ;
#37629 = VERTEX_POINT ( 'NONE', #12593 ) ;
#37630 = VECTOR ( 'NONE', #5972, 999.9999999999998863 ) ;
#37631 = DIRECTION ( 'NONE',  ( 0.7660212471507180654, -0.6427876096865404731, 0.005961354470445141482 ) ) ;
#37632 = CARTESIAN_POINT ( 'NONE',  ( -11.36876430285300543, 2.229229656569007290, 4.955880904987684410 ) ) ;
#37633 = EDGE_CURVE ( 'NONE', #38023, #55289, #12313, .T. ) ;
#37634 = DIRECTION ( 'NONE',  ( 0.5449076811759707706, 0.6444004775717708799, -0.5364919789714476250 ) ) ;
#37635 = LINE ( 'NONE', #28847, #33211 ) ;
#37636 = PRESENTATION_STYLE_ASSIGNMENT (( #42463 ) ) ;
#37637 = VECTOR ( 'NONE', #14053, 1000.000000000000227 ) ;
#37638 = ORIENTED_EDGE ( 'NONE', *, *, #45571, .F. ) ;
#37639 = ADVANCED_FACE ( 'NONE', ( #3768 ), #17130, .F. ) ;
#37640 = ADVANCED_FACE ( 'NONE', ( #8316 ), #34717, .F. ) ;
#37641 = EDGE_CURVE ( 'NONE', #33817, #18318, #33882, .T. ) ;
#37642 = ORIENTED_EDGE ( 'NONE', *, *, #30136, .F. ) ;
#37643 = CARTESIAN_POINT ( 'NONE',  ( -16.03306359442184004, 0.000000000000000000, 8.758286885247480669 ) ) ;
#37644 = DIRECTION ( 'NONE',  ( 0.005961354470445682716, -0.6427876096865404731, -0.7660212471507180654 ) ) ;
#37645 = VECTOR ( 'NONE', #44536, 999.9999999999998863 ) ;
#37646 = EDGE_CURVE ( 'NONE', #3673, #16343, #55743, .T. ) ;
#37647 = CARTESIAN_POINT ( 'NONE',  ( -42.47825799898742360, 8.133442155459132294, -4.990245731342549007 ) ) ;
#37648 = AXIS2_PLACEMENT_3D ( 'NONE', #1222, #5496, #30790 ) ;
#37649 = AXIS2_PLACEMENT_3D ( 'NONE', #40732, #40462, #41282 ) ;
#37650 = DIRECTION ( 'NONE',  ( 0.000000000000000000, 1.000000000000000000, 0.000000000000000000 ) ) ;
#37651 = AXIS2_PLACEMENT_3D ( 'NONE', #12909, #30239, #19908 ) ;
#37652 = DIRECTION ( 'NONE',  ( 0.007781995580012663651, 0.000000000000000000, -0.9999697198139515519 ) ) ;
#37653 = DIRECTION ( 'NONE',  ( 0.7660212471507180654, -0.6427876096865404731, 0.005961354470445141482 ) ) ;
#37654 = ORIENTED_EDGE ( 'NONE', *, *, #45221, .F. ) ;
#37655 = DIRECTION ( 'NONE',  ( 0.7660212471507180654, -0.6427876096865404731, 0.005961354470445141482 ) ) ;
#37656 = ORIENTED_EDGE ( 'NONE', *, *, #42270, .F. ) ;
#37657 = VECTOR ( 'NONE', #20393, 999.9999999999998863 ) ;
#37658 = LINE ( 'NONE', #44845, #6212 ) ;
#37659 = CARTESIAN_POINT ( 'NONE',  ( 2.072287782118878319, 0.000000000000000000, -2.950529333540147015 ) ) ;
#37660 = DIRECTION ( 'NONE',  ( -0.6427681459581293666, -0.7660444431189770143, -0.005002170337467561935 ) ) ;
#37661 = LINE ( 'NONE', #28866, #2712 ) ;
#37662 = EDGE_CURVE ( 'NONE', #2943, #35066, #46954, .T. ) ;
#37663 = FACE_OUTER_BOUND ( 'NONE', #22345, .T. ) ;
#37664 = LINE ( 'NONE', #42739, #44969 ) ;
#37665 = VECTOR ( 'NONE', #27853, 999.9999999999998863 ) ;
#37666 = EDGE_CURVE ( 'NONE', #18658, #29145, #21674, .T. ) ;
#37667 = EDGE_LOOP ( 'NONE', ( #42506, #48262, #54902, #21568 ) ) ;
#37668 = VECTOR ( 'NONE', #11674, 1000.000000000000227 ) ;
#37669 =( BOUNDED_CURVE ( )  B_SPLINE_CURVE ( 3, ( #41363, #2452, #45893, #19773 ),
 .UNSPECIFIED., .F., .F. ) 
 B_SPLINE_CURVE_WITH_KNOTS ( ( 4, 4 ),
 ( -8.881784197001252323E-16, 0.3848561846235226125 ),
 .UNSPECIFIED. ) 
 CURVE ( )  GEOMETRIC_REPRESENTATION_ITEM ( )  RATIONAL_B_SPLINE_CURVE ( ( 1.000000000000000000, 0.9876951826469675400, 0.9876951826469675400, 1.000000000000000000 ) ) 
 REPRESENTATION_ITEM ( '' )  );
#37670 = ORIENTED_EDGE ( 'NONE', *, *, #522, .T. ) ;
#37671 = EDGE_CURVE ( 'NONE', #8156, #20135, #38418, .T. ) ;
#37672 = DIRECTION ( 'NONE',  ( 0.5364919789714477361, 0.6444004775717706579, 0.5449076811759711036 ) ) ;
#37673 = CARTESIAN_POINT ( 'NONE',  ( -21.20308440300454933, -1.975113310420657520, 8.159427204713791681 ) ) ;
#37674 = DIRECTION ( 'NONE',  ( 0.005002170337468016433, -0.7660444431189770143, -0.6427681459581293666 ) ) ;
#37675 = ADVANCED_FACE ( 'NONE', ( #29911 ), #47210, .F. ) ;
#37676 = CARTESIAN_POINT ( 'NONE',  ( -14.94838282604900748, -0.1191753592594197858, 2.588085963191248506 ) ) ;
#37677 = PLANE ( 'NONE',  #9448 ) ;
#37678 = LINE ( 'NONE', #45096, #19121 ) ;
#37679 = DIRECTION ( 'NONE',  ( 0.9999697198139515519, 0.000000000000000000, 0.007781995580013368816 ) ) ;
#37680 = EDGE_CURVE ( 'NONE', #39457, #24901, #38727, .T. ) ;
#37681 = AXIS2_PLACEMENT_3D ( 'NONE', #6726, #2469, #7024 ) ;
#37682 = CARTESIAN_POINT ( 'NONE',  ( -18.67775241435682432, 0.000000000000000000, 4.136394454059623804 ) ) ;
#37683 = VECTOR ( 'NONE', #52630, 1000.000000000000227 ) ;
#37684 = LINE ( 'NONE', #55006, #54621 ) ;
#37685 = ORIENTED_EDGE ( 'NONE', *, *, #52269, .F. ) ;
#37686 = AXIS2_PLACEMENT_3D ( 'NONE', #28279, #49611, #36527 ) ;
#37687 = ORIENTED_EDGE ( 'NONE', *, *, #30145, .T. ) ;
#37688 = VECTOR ( 'NONE', #27171, 999.9999999999998863 ) ;
#37689 = ORIENTED_EDGE ( 'NONE', *, *, #42777, .F. ) ;
#37690 = ORIENTED_EDGE ( 'NONE', *, *, #25851, .T. ) ;
#37691 = VECTOR ( 'NONE', #30460, 1000.000000000000114 ) ;
#37692 = VECTOR ( 'NONE', #43451, 1000.000000000000227 ) ;
#37693 = EDGE_LOOP ( 'NONE', ( #1108, #35677, #14634, #38289 ) ) ;
#37694 = ORIENTED_EDGE ( 'NONE', *, *, #39261, .T. ) ;
#37695 = DIRECTION ( 'NONE',  ( 0.007781995580012663651, 0.000000000000000000, -0.9999697198139515519 ) ) ;
#37696 = DIRECTION ( 'NONE',  ( -0.9090593428863091852, 0.000000000000000000, -0.4166666666666674623 ) ) ;
#37697 = CARTESIAN_POINT ( 'NONE',  ( -24.27063949748155380, 0.000000000000000000, 6.308861732390097288 ) ) ;
#37698 = VECTOR ( 'NONE', #6948, 999.9999999999998863 ) ;
#37699 = VECTOR ( 'NONE', #51592, 1000.000000000000227 ) ;
#37700 = EDGE_LOOP ( 'NONE', ( #11220, #35985, #29001, #35991 ) ) ;
#37701 = LINE ( 'NONE', #28055, #2276 ) ;
#37702 = VECTOR ( 'NONE', #3644, 1000.000000000000227 ) ;
#37703 = EDGE_LOOP ( 'NONE', ( #47052, #33153, #38734, #32923 ) ) ;
#37704 = CARTESIAN_POINT ( 'NONE',  ( -65.54552266609172761, -11.22408668727510239, -5.120420914815952962 ) ) ;
#37705 = VERTEX_POINT ( 'NONE', #47925 ) ;
#37706 = VECTOR ( 'NONE', #43062, 999.9999999999998863 ) ;
#37707 = AXIS2_PLACEMENT_3D ( 'NONE', #42199, #25431, #29726 ) ;
#37708 = CARTESIAN_POINT ( 'NONE',  ( -68.22482764337692629, -9.518226629270689187, 7.369622379056326444 ) ) ;
#37709 = DIRECTION ( 'NONE',  ( -0.005002170337468016433, -0.7660444431189770143, 0.6427681459581293666 ) ) ;
#37710 = CARTESIAN_POINT ( 'NONE',  ( -9.286598691220605772, 0.000000000000000000, 3.470814444211937300 ) ) ;
#37711 = VERTEX_POINT ( 'NONE', #17532 ) ;
#37712 = PLANE ( 'NONE',  #16496 ) ;
#37713 = ORIENTED_EDGE ( 'NONE', *, *, #30885, .F. ) ;
#37714 = EDGE_CURVE ( 'NONE', #50596, #47675, #12145, .T. ) ;
#37715 = ADVANCED_FACE ( 'NONE', ( #39108 ), #16990, .F. ) ;
#37716 = DIRECTION ( 'NONE',  ( 0.007781995580012663651, -3.146120232559066537E-19, -0.9999697198139514409 ) ) ;
#37717 = LINE ( 'NONE', #42528, #41118 ) ;
#37718 = EDGE_CURVE ( 'NONE', #21088, #31624, #7916, .T. ) ;
#37719 = VECTOR ( 'NONE', #45217, 999.9999999999998863 ) ;
#37720 = DIRECTION ( 'NONE',  ( 0.6427681459581294776, -0.7660444431189769032, 0.005002170337467562802 ) ) ;
#37721 = FACE_OUTER_BOUND ( 'NONE', #44277, .T. ) ;
#37722 = FACE_OUTER_BOUND ( 'NONE', #5461, .T. ) ;
#37723 = DIRECTION ( 'NONE',  ( -0.7660212471507179544, -0.6427876096865405842, -0.005961354470445141482 ) ) ;
#37724 = CARTESIAN_POINT ( 'NONE',  ( -26.13337879274045505, 0.000000000000000000, 6.833023547870798353 ) ) ;
#37725 = CARTESIAN_POINT ( 'NONE',  ( -19.71854418059240643, 0.000000000000000000, 4.666952855267993527 ) ) ;
#37726 = ORIENTED_EDGE ( 'NONE', *, *, #12521, .T. ) ;
#37727 = CARTESIAN_POINT ( 'NONE',  ( -14.15307997813123286, 0.000000000000000000, 6.018266850220190811 ) ) ;
#37728 = EDGE_LOOP ( 'NONE', ( #12362, #37812, #22492, #27923 ) ) ;
#37729 = VECTOR ( 'NONE', #28794, 1000.000000000000000 ) ;
#37730 = PLANE ( 'NONE',  #33803 ) ;
#37731 = LINE ( 'NONE', #24942, #19655 ) ;
#37732 = LINE ( 'NONE', #54745, #35037 ) ;
#37733 = AXIS2_PLACEMENT_3D ( 'NONE', #38335, #3981, #55659 ) ;
#37734 = CARTESIAN_POINT ( 'NONE',  ( -8.638865104681501705, 0.000000000000000000, 4.753177479762371149 ) ) ;
#37735 = DIRECTION ( 'NONE',  ( -0.8531650599175529814, -0.4028455766673920135, 0.3313982828793697877 ) ) ;
#37736 = VECTOR ( 'NONE', #23543, 1000.000000000000227 ) ;
#37738 = VECTOR ( 'NONE', #40976, 1000.000000000000227 ) ;
#37737 = CARTESIAN_POINT ( 'NONE',  ( -14.41772293100952673, 0.000000000000000000, 6.016207337568184599 ) ) ;
#37739 = SHAPE_REPRESENTATION_RELATIONSHIP ( 'NONE' , 'NONE' ,  #3156, #26591 ) ;
#37740 = EDGE_LOOP ( 'NONE', ( #49741, #17805, #20849, #8410 ) ) ;
#37741 = CARTESIAN_POINT ( 'NONE',  ( -12.23851102634202448, -0.1191753592594197858, 11.68427982808754884 ) ) ;
#37742 = LINE ( 'NONE', #50215, #6697 ) ;
#37743 = DIRECTION ( 'NONE',  ( -0.9999697198139514409, -0.000000000000000000, -0.007781995580013368816 ) ) ;
#37744 = CARTESIAN_POINT ( 'NONE',  ( -15.80386756661275882, 1.419719901456505395, 5.350082209620479645 ) ) ;
#37746 = CARTESIAN_POINT ( 'NONE',  ( -19.89215662524663841, -2.622721114510659035, 8.713053072339743466 ) ) ;
#37745 = VECTOR ( 'NONE', #35999, 1000.000000000000227 ) ;
#37747 = VECTOR ( 'NONE', #49901, 1000.000000000000227 ) ;
#37748 = PLANE ( 'NONE',  #16438 ) ;
#37749 = CARTESIAN_POINT ( 'NONE',  ( -26.13493519185646008, 0.000000000000000000, 7.033017491833586377 ) ) ;
#37750 = ADVANCED_FACE ( 'NONE', ( #34309 ), #12715, .F. ) ;
#37751 = CARTESIAN_POINT ( 'NONE',  ( -19.45503627000849889, -1.000000000000000000, 7.556996783084074742 ) ) ;
#37752 = CARTESIAN_POINT ( 'NONE',  ( -11.14514627858494755, 0.000000000000000000, 3.456350797139899900 ) ) ;
#37753 = ORIENTED_EDGE ( 'NONE', *, *, #38437, .T. ) ;
#37754 = AXIS2_PLACEMENT_3D ( 'NONE', #5425, #1136, #39515 ) ;
#37756 = DIRECTION ( 'NONE',  ( 0.6427681459581294776, -0.7660444431189769032, 0.005002170337467562802 ) ) ;
#37755 = VECTOR ( 'NONE', #35637, 1000.000000000000114 ) ;
#37757 = CARTESIAN_POINT ( 'NONE',  ( -14.46888367232926420, 0.000000000000000000, 12.59025272694991315 ) ) ;
#37758 = EDGE_LOOP ( 'NONE', ( #44750, #4854, #24992, #21833, #7646 ) ) ;
#37759 = ADVANCED_FACE ( 'NONE', ( #55887 ), #10131, .F. ) ;
#37760 = ORIENTED_EDGE ( 'NONE', *, *, #46659, .T. ) ;
#37761 = DIRECTION ( 'NONE',  ( -0.005961354470445682716, -0.6427876096865404731, 0.7660212471507180654 ) ) ;
#37762 = EDGE_CURVE ( 'NONE', #21477, #2866, #30321, .T. ) ;
#37763 = VERTEX_POINT ( 'NONE', #13293 ) ;
#37764 = EDGE_CURVE ( 'NONE', #33896, #50554, #55299, .T. ) ;
#37765 = EDGE_LOOP ( 'NONE', ( #40123, #10391, #52603, #10597, #31543 ) ) ;
#37766 = DIRECTION ( 'NONE',  ( 0.5449076811759707706, 0.6444004775717708799, -0.5364919789714476250 ) ) ;
#37767 = AXIS2_PLACEMENT_3D ( 'NONE', #36480, #35965, #36783 ) ;
#37768 = ORIENTED_EDGE ( 'NONE', *, *, #56043, .F. ) ;
#37769 = ORIENTED_EDGE ( 'NONE', *, *, #52201, .F. ) ;
#37770 = VERTEX_POINT ( 'NONE', #51034 ) ;
#37771 = FACE_OUTER_BOUND ( 'NONE', #36427, .T. ) ;
#37772 = DIRECTION ( 'NONE',  ( 0.9999697198139515519, 0.000000000000000000, 0.007781995580013368816 ) ) ;
#37773 = VECTOR ( 'NONE', #13374, 1000.000000000000227 ) ;
#37774 = CARTESIAN_POINT ( 'NONE',  ( -12.15116108492864377, 0.000000000000000000, 1.401855352044617975 ) ) ;
#37775 = AXIS2_PLACEMENT_3D ( 'NONE', #51512, #12605, #1497 ) ;
#37776 = ORIENTED_EDGE ( 'NONE', *, *, #3863, .F. ) ;
#37777 = VERTEX_POINT ( 'NONE', #25230 ) ;
#37778 = AXIS2_PLACEMENT_3D ( 'NONE', #14138, #27760, #48782 ) ;
#37779 = PLANE ( 'NONE',  #35745 ) ;
#37780 = PLANE ( 'NONE',  #54452 ) ;
#37781 = VERTEX_POINT ( 'NONE', #34023 ) ;
#37782 = FACE_OUTER_BOUND ( 'NONE', #27208, .T. ) ;
#37783 = EDGE_LOOP ( 'NONE', ( #15377, #28957, #11825, #24339 ) ) ;
#37784 = LINE ( 'NONE', #12203, #52057 ) ;
#37785 = CARTESIAN_POINT ( 'NONE',  ( -26.11787696043622375, 17.53257130528676910, 4.617134652480109125 ) ) ;
#37787 = ORIENTED_EDGE ( 'NONE', *, *, #9856, .T. ) ;
#37786 = EDGE_CURVE ( 'NONE', #223, #31183, #51344, .T. ) ;
#37788 = VECTOR ( 'NONE', #34241, 1000.000000000000000 ) ;
#37789 = DIRECTION ( 'NONE',  ( -0.005002170337468016433, -0.7660444431189770143, 0.6427681459581293666 ) ) ;
#37790 = EDGE_CURVE ( 'NONE', #14283, #49510, #21227, .T. ) ;
#37791 = EDGE_CURVE ( 'NONE', #16476, #46316, #39694, .T. ) ;
#37792 = VECTOR ( 'NONE', #34539, 1000.000000000000000 ) ;
#37793 = PLANE ( 'NONE',  #22748 ) ;
#37794 = VECTOR ( 'NONE', #45212, 999.9999999999998863 ) ;
#37795 = VERTEX_POINT ( 'NONE', #44772 ) ;
#37796 = PLANE ( 'NONE',  #14061 ) ;
#37797 = CARTESIAN_POINT ( 'NONE',  ( -16.30058060080541082, 0.000000000000000000, 9.125537075853236146 ) ) ;
#37798 = ORIENTED_EDGE ( 'NONE', *, *, #30277, .T. ) ;
#37799 = DIRECTION ( 'NONE',  ( 0.005002170337468016433, -0.7660444431189770143, -0.6427681459581293666 ) ) ;
#37800 = DIRECTION ( 'NONE',  ( 0.000000000000000000, -1.000000000000000000, 0.000000000000000000 ) ) ;
#37801 = CARTESIAN_POINT ( 'NONE',  ( -12.24986416390947497, 2.714935509636507316, 6.095256065150636893 ) ) ;
#37802 = FACE_OUTER_BOUND ( 'NONE', #8343, .T. ) ;
#37803 = DIRECTION ( 'NONE',  ( 0.007781995580012663651, -3.146120232559066537E-19, -0.9999697198139514409 ) ) ;
#37804 = DIRECTION ( 'NONE',  ( -0.5449076811759708816, 0.6444004775717707689, 0.5364919789714475140 ) ) ;
#37805 = VECTOR ( 'NONE', #31525, 999.9999999999998863 ) ;
#37806 = EDGE_CURVE ( 'NONE', #36112, #883, #35702, .T. ) ;
#37807 = PLANE ( 'NONE',  #13214 ) ;
#37808 = VERTEX_POINT ( 'NONE', #36010 ) ;
#37809 = PLANE ( 'NONE',  #832 ) ;
#37810 = CARTESIAN_POINT ( 'NONE',  ( -1.086233639165236964, 0.000000000000000000, -2.796443541562362078 ) ) ;
#37811 = CARTESIAN_POINT ( 'NONE',  ( -68.37651787278942095, 7.120427645301669091E-12, 6.778377825370101029 ) ) ;
#37812 = ORIENTED_EDGE ( 'NONE', *, *, #28827, .F. ) ;
#37813 = LINE ( 'NONE', #28730, #11135 ) ;
#37814 = CARTESIAN_POINT ( 'NONE',  ( -9.762731802082821986, 0.000000000000000000, 4.944437345474987033 ) ) ;
#37815 = AXIS2_PLACEMENT_3D ( 'NONE', #4446, #43600, #44187 ) ;
#37816 = CARTESIAN_POINT ( 'NONE',  ( -12.33850799832341849, 0.000000000000000000, 11.68350162852954632 ) ) ;
#37817 = CARTESIAN_POINT ( 'NONE',  ( -27.99767448711536133, 0.000000000000000000, 7.557179307314289218 ) ) ;
#37818 = PLANE ( 'NONE',  #12961 ) ;
#37819 = ORIENTED_EDGE ( 'NONE', *, *, #33961, .F. ) ;
#37820 = AXIS2_PLACEMENT_3D ( 'NONE', #44423, #31927, #53777 ) ;
#37821 = VERTEX_POINT ( 'NONE', #53019 ) ;
#37822 = CARTESIAN_POINT ( 'NONE',  ( -10.84028925556084388, -0.1191753592594197858, 11.14116300850493246 ) ) ;
#37823 = CARTESIAN_POINT ( 'NONE',  ( -19.64439698464071427, -1.813211359398158029, 4.454021096977195171 ) ) ;
#37824 = AXIS2_PLACEMENT_3D ( 'NONE', #7189, #37558, #21072 ) ;
#37825 = ORIENTED_EDGE ( 'NONE', *, *, #34815, .T. ) ;
#37826 = DIRECTION ( 'NONE',  ( -0.005961354470445682716, -0.6427876096865404731, 0.7660212471507180654 ) ) ;
#37827 = EDGE_CURVE ( 'NONE', #32241, #8639, #9286, .T. ) ;
#37828 = VERTEX_POINT ( 'NONE', #27174 ) ;
#37829 = LINE ( 'NONE', #29595, #29288 ) ;
#37830 = AXIS2_PLACEMENT_3D ( 'NONE', #20760, #45465, #38074 ) ;
#37831 = ORIENTED_EDGE ( 'NONE', *, *, #39299, .T. ) ;
#37832 = ORIENTED_EDGE ( 'NONE', *, *, #18874, .F. ) ;
#37833 = ORIENTED_EDGE ( 'NONE', *, *, #46363, .T. ) ;
#37834 = CARTESIAN_POINT ( 'NONE',  ( -9.110551994824897193, -1.000000000000000000, 3.538847790438064411 ) ) ;
#37835 = CARTESIAN_POINT ( 'NONE',  ( -12.54899678401333496, 0.000000000000000000, 4.722747930904141356 ) ) ;
#37836 = CARTESIAN_POINT ( 'NONE',  ( -10.80508224072880452, -0.1117717739994080611, 7.415434460100314595 ) ) ;
#37837 = EDGE_CURVE ( 'NONE', #44124, #29311, #5587, .T. ) ;
#37838 = DIRECTION ( 'NONE',  ( 0.5364919789714477361, 0.6444004775717706579, 0.5449076811759711036 ) ) ;
#37839 = ORIENTED_EDGE ( 'NONE', *, *, #9176, .T. ) ;
#37840 = ADVANCED_FACE ( 'NONE', ( #9872 ), #53319, .F. ) ;
#37841 = EDGE_CURVE ( 'NONE', #22744, #51840, #22639, .T. ) ;
#37842 = ORIENTED_EDGE ( 'NONE', *, *, #34492, .F. ) ;
#37843 = ORIENTED_EDGE ( 'NONE', *, *, #48391, .T. ) ;
#37844 = LINE ( 'NONE', #37540, #48564 ) ;
#37845 = LINE ( 'NONE', #16818, #5887 ) ;
#37846 = ORIENTED_EDGE ( 'NONE', *, *, #42442, .T. ) ;
#37847 = PLANE ( 'NONE',  #49310 ) ;
#37848 = EDGE_CURVE ( 'NONE', #33592, #53425, #10428, .T. ) ;
#37849 = ORIENTED_EDGE ( 'NONE', *, *, #16469, .T. ) ;
#37850 = FACE_OUTER_BOUND ( 'NONE', #26705, .T. ) ;
#37851 = CARTESIAN_POINT ( 'NONE',  ( -19.12962290826653700, 0.000000000000000000, 14.40064212555863854 ) ) ;
#37852 = ORIENTED_EDGE ( 'NONE', *, *, #14215, .F. ) ;
#37853 = ADVANCED_FACE ( 'NONE', ( #14133 ), #49028, .F. ) ;
#37854 = LINE ( 'NONE', #33317, #22298 ) ;
#37855 = ORIENTED_EDGE ( 'NONE', *, *, #16398, .F. ) ;
#37856 = EDGE_CURVE ( 'NONE', #20361, #38484, #1619, .T. ) ;
#37857 = VECTOR ( 'NONE', #19981, 999.9999999999998863 ) ;
#37858 = FACE_OUTER_BOUND ( 'NONE', #6821, .T. ) ;
#37859 = DIRECTION ( 'NONE',  ( 0.9999697198139515519, 0.000000000000000000, 0.007781995580013368816 ) ) ;
#37860 = CARTESIAN_POINT ( 'NONE',  ( 2.072287782118878319, 0.000000000000000000, -2.950529333540147015 ) ) ;
#37861 =( NAMED_UNIT ( * ) PLANE_ANGLE_UNIT ( ) SI_UNIT ( $, .RADIAN. ) );
#37862 = DIRECTION ( 'NONE',  ( 0.005961354470445682716, -0.6427876096865404731, -0.7660212471507180654 ) ) ;
#37863 = FACE_OUTER_BOUND ( 'NONE', #32806, .T. ) ;
#37864 = EDGE_LOOP ( 'NONE', ( #47330, #53670, #24660, #6865 ) ) ;
#37865 = EDGE_CURVE ( 'NONE', #18631, #873, #773, .T. ) ;
#37866 = VERTEX_POINT ( 'NONE', #27447 ) ;
#37867 = AXIS2_PLACEMENT_3D ( 'NONE', #22570, #44412, #48699 ) ;
#37868 = CARTESIAN_POINT ( 'NONE',  ( -12.61734217886482057, -3.432230869623162928, 1.672819171754234890 ) ) ;
#37869 = LINE ( 'NONE', #46088, #13959 ) ;
#37870 = CARTESIAN_POINT ( 'NONE',  ( -69.48902198128583052, 0.1329003158168008403, 6.824617610603328721 ) ) ;
#37871 = LINE ( 'NONE', #20235, #36685 ) ;
#37872 = LINE ( 'NONE', #11730, #15249 ) ;
#37873 = EDGE_CURVE ( 'NONE', #21088, #49698, #14668, .T. ) ;
#37874 = CARTESIAN_POINT ( 'NONE',  ( -14.66887761629205222, 0.000000000000000000, 12.58869632783390990 ) ) ;
#37875 = ORIENTED_EDGE ( 'NONE', *, *, #47487, .T. ) ;
#37876 = CARTESIAN_POINT ( 'NONE',  ( -15.06775173312542826, 5.467268677019012202, 11.70686692005663865 ) ) ;
#37877 = CARTESIAN_POINT ( 'NONE',  ( -16.53317331066696383, 0.000000000000000000, 13.31285208727739899 ) ) ;
#37878 = ORIENTED_EDGE ( 'NONE', *, *, #19434, .F. ) ;
#37879 = DIRECTION ( 'NONE',  ( 0.005961354470445682716, -0.6427876096865404731, -0.7660212471507180654 ) ) ;
#37880 = ORIENTED_EDGE ( 'NONE', *, *, #526, .T. ) ;
#37881 = CYLINDRICAL_SURFACE ( 'NONE', #30732, 3.000000000000001332 ) ;
#37882 = DIRECTION ( 'NONE',  ( 0.007781995580012663651, -3.146120232559066537E-19, -0.9999697198139514409 ) ) ;
#37883 = FACE_OUTER_BOUND ( 'NONE', #42078, .T. ) ;
#37884 = DIRECTION ( 'NONE',  ( 0.005002170337468016433, -0.7660444431189770143, -0.6427681459581293666 ) ) ;
#37885 = CARTESIAN_POINT ( 'NONE',  ( -67.35931108517087296, 1.999999999999983569, -7.222001337324623904 ) ) ;
#37886 = ORIENTED_EDGE ( 'NONE', *, *, #5637, .T. ) ;
#37887 = ORIENTED_EDGE ( 'NONE', *, *, #38441, .T. ) ;
#37888 = CARTESIAN_POINT ( 'NONE',  ( -67.46543143576477064, -0.6008375282045697041, 3.326521589947856405 ) ) ;
#37889 = DIRECTION ( 'NONE',  ( -0.5449076811759708816, 0.6444004775717707689, 0.5364919789714475140 ) ) ;
#37890 = CARTESIAN_POINT ( 'NONE',  ( -25.20123094555300369, 0.000000000000000000, 6.470945668149052032 ) ) ;
#37891 = DIRECTION ( 'NONE',  ( -0.005002170337468016433, -0.7660444431189770143, 0.6427681459581293666 ) ) ;
#37892 = CARTESIAN_POINT ( 'NONE',  ( -18.19747506107908563, 0.000000000000000000, 14.03856424583689311 ) ) ;
#37893 = FACE_OUTER_BOUND ( 'NONE', #48669, .T. ) ;
#37894 = EDGE_CURVE ( 'NONE', #48923, #37770, #23213, .T. ) ;
#37895 = VERTEX_POINT ( 'NONE', #4751 ) ;
#37896 = LINE ( 'NONE', #50666, #23815 ) ;
#37897 = CARTESIAN_POINT ( 'NONE',  ( -20.49657252799461560, -2.784623065533158304, 9.213537418967975512 ) ) ;
#37898 = LINE ( 'NONE', #29679, #42350 ) ;
#37899 = VERTEX_POINT ( 'NONE', #18092 ) ;
#37900 = FACE_OUTER_BOUND ( 'NONE', #43218, .T. ) ;
#37901 = PLANE ( 'NONE',  #34773 ) ;
#37902 = ORIENTED_EDGE ( 'NONE', *, *, #49650, .T. ) ;
#37903 = VECTOR ( 'NONE', #24709, 1000.000000000000227 ) ;
#37904 = LINE ( 'NONE', #54632, #36812 ) ;
#37905 = ORIENTED_EDGE ( 'NONE', *, *, #33344, .T. ) ;
#37906 = EDGE_CURVE ( 'NONE', #40238, #9638, #22073, .T. ) ;
#37907 = ORIENTED_EDGE ( 'NONE', *, *, #54240, .F. ) ;
#37908 = ORIENTED_EDGE ( 'NONE', *, *, #13920, .T. ) ;
#37909 = ORIENTED_EDGE ( 'NONE', *, *, #30902, .F. ) ;
#37910 = CARTESIAN_POINT ( 'NONE',  ( -15.40103151951671734, 0.000000000000000000, 12.95233060667165681 ) ) ;
#37911 = ORIENTED_EDGE ( 'NONE', *, *, #46611, .T. ) ;
#37912 = LINE ( 'NONE', #33627, #38535 ) ;
#37913 = VERTEX_POINT ( 'NONE', #5330 ) ;
#37914 = DIRECTION ( 'NONE',  ( -0.005002170337468016433, -0.7660444431189770143, 0.6427681459581293666 ) ) ;
#37915 = EDGE_CURVE ( 'NONE', #8596, #42084, #52461, .T. ) ;
#37916 = ORIENTED_EDGE ( 'NONE', *, *, #39402, .F. ) ;
#37917 = ORIENTED_EDGE ( 'NONE', *, *, #27376, .F. ) ;
#37918 = ADVANCED_FACE ( 'NONE', ( #26607 ), #30870, .F. ) ;
#37919 = LINE ( 'NONE', #19757, #40278 ) ;
#37920 = DIRECTION ( 'NONE',  ( -0.5449076811759708816, 0.6444004775717707689, 0.5364919789714475140 ) ) ;
#37921 = CARTESIAN_POINT ( 'NONE',  ( -21.34570666360650293, 1.905425754524007198, 8.299846768392162843 ) ) ;
#37922 = CARTESIAN_POINT ( 'NONE',  ( -12.53618291560292519, 0.000000000000000000, 3.076193358578107162 ) ) ;
#37923 = CARTESIAN_POINT ( 'NONE',  ( -11.67244013076689946, 0.000000000000000000, 11.50401908778467863 ) ) ;
#37924 = ORIENTED_EDGE ( 'NONE', *, *, #40433, .F. ) ;
#37925 = EDGE_CURVE ( 'NONE', #19938, #27147, #9594, .T. ) ;
#37926 = ORIENTED_EDGE ( 'NONE', *, *, #15073, .T. ) ;
#37927 = DIRECTION ( 'NONE',  ( 0.6427681459581294776, -0.7660444431189769032, 0.005002170337467562802 ) ) ;
#37928 = LINE ( 'NONE', #24858, #17616 ) ;
#37929 = CARTESIAN_POINT ( 'NONE',  ( -13.21075357131192618, 0.000000000000000000, 4.348265916762363403 ) ) ;
#37930 = ADVANCED_FACE ( 'NONE', ( #18364 ), #37349, .F. ) ;
#37931 = PLANE ( 'NONE',  #15822 ) ;
#37932 = FACE_OUTER_BOUND ( 'NONE', #28116, .T. ) ;
#37933 = CARTESIAN_POINT ( 'NONE',  ( -11.82546504130451304, 0.000000000000000000, 5.467042761839684850 ) ) ;
#37934 = ORIENTED_EDGE ( 'NONE', *, *, #19818, .F. ) ;
#37935 = DIRECTION ( 'NONE',  ( -0.6427681459581293666, -0.7660444431189770143, -0.005002170337467561935 ) ) ;
#37936 = CARTESIAN_POINT ( 'NONE',  ( -13.53673582514181106, 0.000000000000000000, 12.22817484722816772 ) ) ;
#37937 = VERTEX_POINT ( 'NONE', #41364 ) ;
#37938 = AXIS2_PLACEMENT_3D ( 'NONE', #49680, #15037, #3299 ) ;
#37939 = DIRECTION ( 'NONE',  ( -0.7660212471507179544, -0.6427876096865405842, -0.005961354470445141482 ) ) ;
#37940 = PLANE ( 'NONE',  #10596 ) ;
#37941 = CARTESIAN_POINT ( 'NONE',  ( -29.86197018149027116, 0.000000000000000000, 8.281335066757780083 ) ) ;
#37942 = FACE_OUTER_BOUND ( 'NONE', #26302, .T. ) ;
#37943 = DIRECTION ( 'NONE',  ( -0.5364919789714478471, 0.6444004775717705469, -0.5449076811759709926 ) ) ;
#37944 = ORIENTED_EDGE ( 'NONE', *, *, #38681, .T. ) ;
#37945 = VERTEX_POINT ( 'NONE', #32560 ) ;
#37946 = CARTESIAN_POINT ( 'NONE',  ( -16.53317331066696383, 0.000000000000000000, 13.31285208727739899 ) ) ;
#37947 = LINE ( 'NONE', #16940, #47654 ) ;
#37948 = CARTESIAN_POINT ( 'NONE',  ( -16.30213699992141585, 0.000000000000000000, 9.325531019816025946 ) ) ;
#37949 = EDGE_CURVE ( 'NONE', #18997, #6417, #53842, .T. ) ;
#37950 = CARTESIAN_POINT ( 'NONE',  ( -14.51406764992763776, -0.1191753592594188005, 5.546122462771021056 ) ) ;
#37951 = CARTESIAN_POINT ( 'NONE',  ( 2.072287782118878319, 0.000000000000000000, -2.950529333540147015 ) ) ;
#37952 = ADVANCED_FACE ( 'NONE', ( #1872 ), #46157, .F. ) ;
#37953 = CARTESIAN_POINT ( 'NONE',  ( -11.62259704383644277, 0.000000000000000000, 5.099289457697922856 ) ) ;
#37954 = CARTESIAN_POINT ( 'NONE',  ( -15.45705336148688147, -3.432230869623159819, 8.318851767706947342 ) ) ;
#37955 = DIRECTION ( 'NONE',  ( 0.000000000000000000, -1.000000000000000000, 0.000000000000000000 ) ) ;
#37956 = DIRECTION ( 'NONE',  ( -0.005961354470445682716, -0.6427876096865404731, 0.7660212471507180654 ) ) ;
#37957 = EDGE_CURVE ( 'NONE', #16451, #28682, #19488, .T. ) ;
#37958 = EDGE_CURVE ( 'NONE', #25675, #39658, #6438, .T. ) ;
#37959 = DIRECTION ( 'NONE',  ( 0.005961354470445682716, -0.6427876096865404731, -0.7660212471507180654 ) ) ;
#37960 = VERTEX_POINT ( 'NONE', #23740 ) ;
#37961 = DIRECTION ( 'NONE',  ( 0.000000000000000000, -0.000000000000000000, -1.000000000000000000 ) ) ;
#37962 = EDGE_CURVE ( 'NONE', #3565, #29285, #19774, .T. ) ;
#37963 = ADVANCED_FACE ( 'NONE', ( #41621 ), #15492, .F. ) ;
#37964 = EDGE_CURVE ( 'NONE', #39202, #10560, #28023, .T. ) ;
#37965 = VERTEX_POINT ( 'NONE', #50703 ) ;
#37966 = ORIENTED_EDGE ( 'NONE', *, *, #30573, .T. ) ;
#37967 = ORIENTED_EDGE ( 'NONE', *, *, #23738, .F. ) ;
#37968 = VERTEX_POINT ( 'NONE', #40800 ) ;
#37969 = EDGE_LOOP ( 'NONE', ( #25466, #49623, #43941, #51567 ) ) ;
#37970 = ORIENTED_EDGE ( 'NONE', *, *, #18874, .T. ) ;
#37971 = LINE ( 'NONE', #55277, #45926 ) ;
#37972 = DIRECTION ( 'NONE',  ( -0.6246952433987894571, 0.7422098413412802076, 0.2426528472758539834 ) ) ;
#37973 = LINE ( 'NONE', #20910, #23065 ) ;
#37974 = AXIS2_PLACEMENT_3D ( 'NONE', #13694, #43789, #39828 ) ;
#37975 = VERTEX_POINT ( 'NONE', #33119 ) ;
#37976 = CARTESIAN_POINT ( 'NONE',  ( 2.072287782118878319, 0.000000000000000000, -2.950529333540147015 ) ) ;
#37977 = EDGE_CURVE ( 'NONE', #9624, #51983, #2985, .T. ) ;
#37978 = ORIENTED_EDGE ( 'NONE', *, *, #39887, .F. ) ;
#37979 = DIRECTION ( 'NONE',  ( 0.005002170337468016433, -0.7660444431189770143, -0.6427681459581293666 ) ) ;
#37980 = ORIENTED_EDGE ( 'NONE', *, *, #47125, .F. ) ;
#37981 = EDGE_CURVE ( 'NONE', #17653, #18910, #45598, .T. ) ;
#37982 = CARTESIAN_POINT ( 'NONE',  ( -65.90632570267226242, -9.252354265052927573, 0.3563396981035996669 ) ) ;
#37983 = ADVANCED_FACE ( 'NONE', ( #24032 ), #45894, .F. ) ;
#37984 = CARTESIAN_POINT ( 'NONE',  ( -24.26908309836554878, 0.000000000000000000, 6.108867788427308376 ) ) ;
#37985 = CARTESIAN_POINT ( 'NONE',  ( -69.40690260994486493, -9.931727281594525891, -7.501514206501486370 ) ) ;
#37986 = VERTEX_POINT ( 'NONE', #20313 ) ;
#37987 = LINE ( 'NONE', #30022, #5640 ) ;
#37988 = ORIENTED_EDGE ( 'NONE', *, *, #37397, .F. ) ;
#37989 = EDGE_CURVE ( 'NONE', #38023, #22884, #7009, .T. ) ;
#37990 = LINE ( 'NONE', #30312, #36395 ) ;
#37991 = DIRECTION ( 'NONE',  ( 0.9999697198139515519, 0.000000000000000000, 0.007781995580013368816 ) ) ;
#37992 = CARTESIAN_POINT ( 'NONE',  ( -11.35663643656886634, 0.000000000000000000, 4.932033211054954513 ) ) ;
#37993 = FACE_OUTER_BOUND ( 'NONE', #15554, .T. ) ;
#37994 = DIRECTION ( 'NONE',  ( 0.000000000000000000, -0.000000000000000000, -1.000000000000000000 ) ) ;
#37996 =( BOUNDED_CURVE ( )  B_SPLINE_CURVE ( 3, ( #8197, #20704, #29795, #42821 ),
 .UNSPECIFIED., .F., .F. ) 
 B_SPLINE_CURVE_WITH_KNOTS ( ( 4, 4 ),
 ( 3.141592653589797113, 4.281995669727205467 ),
 .UNSPECIFIED. ) 
 CURVE ( )  GEOMETRIC_REPRESENTATION_ITEM ( )  RATIONAL_B_SPLINE_CURVE ( ( 1.000000000000000000, 0.8945281452387652266, 0.8945281452387652266, 1.000000000000000000 ) ) 
 REPRESENTATION_ITEM ( '' )  );
#37995 = DIRECTION ( 'NONE',  ( 0.5364919789714477361, 0.6444004775717706579, 0.5449076811759711036 ) ) ;
#37997 = LINE ( 'NONE', #21225, #44782 ) ;
#37998 = CARTESIAN_POINT ( 'NONE',  ( -69.67957132394272435, -8.678494591075715192, -7.555920072494596518 ) ) ;
#37999 = EDGE_CURVE ( 'NONE', #7373, #49510, #37097, .T. ) ;
#38000 = EDGE_LOOP ( 'NONE', ( #28317, #15744, #52944, #18267 ) ) ;
#38001 = LINE ( 'NONE', #2218, #37436 ) ;
#38002 = VERTEX_POINT ( 'NONE', #28858 ) ;
#38003 = PLANE ( 'NONE',  #44662 ) ;
#38004 = DIRECTION ( 'NONE',  ( -0.5364919789714478471, 0.6444004775717705469, -0.5449076811759709926 ) ) ;
#38005 = PLANE ( 'NONE',  #25953 ) ;
#38006 = LINE ( 'NONE', #30044, #557 ) ;
#38007 = PLANE ( 'NONE',  #27697 ) ;
#38008 = CARTESIAN_POINT ( 'NONE',  ( 2.072287782118878319, 0.000000000000000000, -2.950529333540147015 ) ) ;
#38009 = SHAPE_DEFINITION_REPRESENTATION ( #13296, #12294 ) ;
#38010 = ORIENTED_EDGE ( 'NONE', *, *, #53864, .T. ) ;
#38011 = DIRECTION ( 'NONE',  ( 0.000000000000000000, -1.000000000000000000, 0.000000000000000000 ) ) ;
#38012 = FACE_OUTER_BOUND ( 'NONE', #5198, .T. ) ;
#38013 = CARTESIAN_POINT ( 'NONE',  ( -9.400187731170413841, -0.1191753592594185784, 5.216587788961361660 ) ) ;
#38014 = DIRECTION ( 'NONE',  ( 0.9999697198139515519, 0.000000000000000000, 0.007781995580013368816 ) ) ;
#38015 = DIRECTION ( 'NONE',  ( 0.3535533905932752297, -0.6123724356957952475, 0.7071067811865462405 ) ) ;
#38016 = CARTESIAN_POINT ( 'NONE',  ( -22.40634380310664397, 0.000000000000000000, 5.584705972946605534 ) ) ;
#38017 = DIRECTION ( 'NONE',  ( 0.007781995580012663651, 0.000000000000000000, -0.9999697198139515519 ) ) ;
#38018 = DIRECTION ( 'NONE',  ( -0.5364919789714478471, 0.6444004775717705469, -0.5449076811759709926 ) ) ;
#38019 = VERTEX_POINT ( 'NONE', #11243 ) ;
#38020 = CARTESIAN_POINT ( 'NONE',  ( -31.72782227498118601, 0.000000000000000000, 9.205484770164058972 ) ) ;
#38021 = DIRECTION ( 'NONE',  ( 0.000000000000000000, -1.000000000000000000, 0.000000000000000000 ) ) ;
#38022 = VERTEX_POINT ( 'NONE', #7262 ) ;
#38023 = VERTEX_POINT ( 'NONE', #28569 ) ;
#38024 = FACE_BOUND ( 'NONE', #12369, .T. ) ;
#38025 = EDGE_CURVE ( 'NONE', #52283, #21986, #24568, .T. ) ;
#38026 = EDGE_CURVE ( 'NONE', #29873, #47765, #33397, .T. ) ;
#38027 = EDGE_LOOP ( 'NONE', ( #30948, #27790, #19109, #34129 ) ) ;
#38028 = ORIENTED_EDGE ( 'NONE', *, *, #41030, .F. ) ;
#38029 = CARTESIAN_POINT ( 'NONE',  ( -18.55457632951175384, -0.5179957512181557755, 4.072021903158996814 ) ) ;
#38030 = EDGE_CURVE ( 'NONE', #33009, #12251, #6180, .T. ) ;
#38031 = EDGE_LOOP ( 'NONE', ( #16056, #28280, #49062, #37173 ) ) ;
#38032 = ORIENTED_EDGE ( 'NONE', *, *, #32173, .F. ) ;
#38033 = VERTEX_POINT ( 'NONE', #12072 ) ;
#38034 = DIRECTION ( 'NONE',  ( 0.9999697198139515519, 0.000000000000000000, 0.007781995580013368816 ) ) ;
#38035 = CARTESIAN_POINT ( 'NONE',  ( -65.08325356666762218, -9.157969123114190424, 0.6641167203970371746 ) ) ;
#38036 = FACE_OUTER_BOUND ( 'NONE', #54948, .T. ) ;
#38037 = ORIENTED_EDGE ( 'NONE', *, *, #12987, .T. ) ;
#38038 = VERTEX_POINT ( 'NONE', #39043 ) ;
#38039 = EDGE_CURVE ( 'NONE', #22163, #50409, #52103, .T. ) ;
#38040 = DIRECTION ( 'NONE',  ( 0.000000000000000000, -1.000000000000000000, 0.000000000000000000 ) ) ;
#38041 = CARTESIAN_POINT ( 'NONE',  ( -18.11794600974973690, 0.000000000000000000, 3.819251942559406476 ) ) ;
#38042 = EDGE_LOOP ( 'NONE', ( #50474, #9791, #14328, #27024 ) ) ;
#38043 = ADVANCED_FACE ( 'NONE', ( #12922 ), #8378, .F. ) ;
#38044 = CARTESIAN_POINT ( 'NONE',  ( -14.52177580689696335, 1.581621852479005774, 2.272220598678369896 ) ) ;
#38045 = CARTESIAN_POINT ( 'NONE',  ( -14.63053074338272808, 0.000000000000000000, 7.661205510778215988 ) ) ;
#38046 = ORIENTED_EDGE ( 'NONE', *, *, #4202, .F. ) ;
#38047 = DIRECTION ( 'NONE',  ( -0.005002170337468016433, -0.7660444431189770143, 0.6427681459581293666 ) ) ;
#38048 = DIRECTION ( 'NONE',  ( 0.005961354470445682716, -0.6427876096865404731, -0.7660212471507180654 ) ) ;
#38049 = ORIENTED_EDGE ( 'NONE', *, *, #29960, .T. ) ;
#38050 = EDGE_CURVE ( 'NONE', #27352, #39726, #29408, .T. ) ;
#38051 = CARTESIAN_POINT ( 'NONE',  ( -20.54049170961573267, 0.000000000000000000, 4.660556269540326646 ) ) ;
#38052 = FACE_OUTER_BOUND ( 'NONE', #5264, .T. ) ;
#38053 = ORIENTED_EDGE ( 'NONE', *, *, #365, .T. ) ;
#38054 = CARTESIAN_POINT ( 'NONE',  ( 5.454592090961233097, -6.230699628392518008, 2.061810099490656079 ) ) ;
#38055 = CARTESIAN_POINT ( 'NONE',  ( 0.1285714285714296967, 2.000000000000000000, -5.998622290806041590 ) ) ;
#38056 = DIRECTION ( 'NONE',  ( 0.005961354470445682716, -0.6427876096865404731, -0.7660212471507180654 ) ) ;
#38057 = LINE ( 'NONE', #16196, #20119 ) ;
#38058 = EDGE_CURVE ( 'NONE', #26839, #34987, #17184, .T. ) ;
#38059 = ORIENTED_EDGE ( 'NONE', *, *, #11804, .F. ) ;
#38060 = CARTESIAN_POINT ( 'NONE',  ( -17.40398185690282773, 0.000000000000000000, 5.792961523881334784 ) ) ;
#38061 = CARTESIAN_POINT ( 'NONE',  ( -14.13296160359425535, 0.000000000000000000, 3.433098927415837665 ) ) ;
#38062 = DIRECTION ( 'NONE',  ( -0.005002170337468016433, -0.7660444431189770143, 0.6427681459581293666 ) ) ;
#38063 = CARTESIAN_POINT ( 'NONE',  ( -16.06709938707323460, 0.000000000000000000, 13.13181314741652628 ) ) ;
#38064 = PLANE ( 'NONE',  #51232 ) ;
#38065 = CARTESIAN_POINT ( 'NONE',  ( 2.072287782118878319, 0.000000000000000000, -2.950529333540147015 ) ) ;
#38066 = DIRECTION ( 'NONE',  ( 0.005961354470445682716, -0.6427876096865404731, -0.7660212471507180654 ) ) ;
#38067 = EDGE_LOOP ( 'NONE', ( #23517, #54171, #38168, #24401 ) ) ;
#38068 = CARTESIAN_POINT ( 'NONE',  ( -1.086233639165236964, 0.000000000000000000, -2.796443541562362078 ) ) ;
#38069 = DIRECTION ( 'NONE',  ( 0.8531650599175529814, -0.4028455766673920135, -0.3313982828793697877 ) ) ;
#38070 = ORIENTED_EDGE ( 'NONE', *, *, #18641, .T. ) ;
#38071 = DIRECTION ( 'NONE',  ( 0.6427681459581294776, -0.7660444431189769032, 0.005002170337467562802 ) ) ;
#38072 = CARTESIAN_POINT ( 'NONE',  ( -9.312785598294761158, 0.000000000000000000, 6.835775765571639795 ) ) ;
#38073 = DIRECTION ( 'NONE',  ( 0.005961354470445682716, -0.6427876096865404731, -0.7660212471507180654 ) ) ;
#38074 = DIRECTION ( 'NONE',  ( 0.6427681459581294776, -0.7660444431189769032, 0.005002170337467562802 ) ) ;
#38075 = DIRECTION ( 'NONE',  ( 0.007781995580012663651, 0.000000000000000000, -0.9999697198139515519 ) ) ;
#38076 = ORIENTED_EDGE ( 'NONE', *, *, #16304, .T. ) ;
#38077 = ORIENTED_EDGE ( 'NONE', *, *, #16381, .T. ) ;
#38078 = CARTESIAN_POINT ( 'NONE',  ( 0.2239497891030736432, -1.668917571073590400, 5.998622290806041590 ) ) ;
#38079 = DIRECTION ( 'NONE',  ( 0.005961354470445682716, -0.6427876096865404731, -0.7660212471507180654 ) ) ;
#38080 = ORIENTED_EDGE ( 'NONE', *, *, #1288, .T. ) ;
#38081 = LINE ( 'NONE', #37521, #290 ) ;
#38082 = ADVANCED_FACE ( 'NONE', ( #25168 ), #29968, .F. ) ;
#38083 = ORIENTED_EDGE ( 'NONE', *, *, #46483, .T. ) ;
#38084 = DIRECTION ( 'NONE',  ( 0.007781995580012663651, -3.146120232559066537E-19, -0.9999697198139514409 ) ) ;
#38085 = ORIENTED_EDGE ( 'NONE', *, *, #42110, .F. ) ;
#38086 = DIRECTION ( 'NONE',  ( -0.005002170337468016433, -0.7660444431189770143, 0.6427681459581293666 ) ) ;
#38087 = EDGE_CURVE ( 'NONE', #34545, #34911, #20871, .T. ) ;
#38088 = EDGE_CURVE ( 'NONE', #50295, #32412, #4140, .T. ) ;
#38089 = ORIENTED_EDGE ( 'NONE', *, *, #31929, .F. ) ;
#38090 = VERTEX_POINT ( 'NONE', #116 ) ;
#38091 = ORIENTED_EDGE ( 'NONE', *, *, #31169, .T. ) ;
#38092 = DIRECTION ( 'NONE',  ( -0.5449076811759708816, 0.6444004775717707689, 0.5364919789714475140 ) ) ;
#38093 = CARTESIAN_POINT ( 'NONE',  ( -19.12962290826653700, 0.000000000000000000, 14.40064212555863854 ) ) ;
#38094 = CARTESIAN_POINT ( 'NONE',  ( -13.68990958973064664, 3.362543313726509719, 1.892274790874030943 ) ) ;
#38095 = DIRECTION ( 'NONE',  ( 0.000000000000000000, -1.000000000000000000, 0.000000000000000000 ) ) ;
#38096 = EDGE_LOOP ( 'NONE', ( #7415, #7354, #37615, #40749 ) ) ;
#38097 = ORIENTED_EDGE ( 'NONE', *, *, #17691, .F. ) ;
#38098 = ORIENTED_EDGE ( 'NONE', *, *, #4196, .T. ) ;
#38099 = DIRECTION ( 'NONE',  ( 0.9999697198139515519, 0.000000000000000000, 0.007781995580013368816 ) ) ;
#38100 = LINE ( 'NONE', #55414, #42710 ) ;
#38101 = ORIENTED_EDGE ( 'NONE', *, *, #12474, .T. ) ;
#38102 = CARTESIAN_POINT ( 'NONE',  ( -16.89152113916034992, -4.565544526780660917, 10.73600855493934247 ) ) ;
#38103 = ORIENTED_EDGE ( 'NONE', *, *, #53909, .F. ) ;
#38104 = PLANE ( 'NONE',  #55030 ) ;
#38105 = CARTESIAN_POINT ( 'NONE',  ( -11.22714339797767558, -0.1191753592594190225, 1.142630195505416557 ) ) ;
#38106 = VERTEX_POINT ( 'NONE', #37933 ) ;
#38107 = DIRECTION ( 'NONE',  ( 0.005961354470445682716, -0.6427876096865404731, -0.7660212471507180654 ) ) ;
#38108 = ORIENTED_EDGE ( 'NONE', *, *, #8832, .T. ) ;
#38109 = ADVANCED_FACE ( 'NONE', ( #4422 ), #21733, .F. ) ;
#38110 = VECTOR ( 'NONE', #1628, 1000.000000000000227 ) ;
#38111 = DIRECTION ( 'NONE',  ( 0.007781995580012662783, 0.000000000000000000, -0.9999697198139514409 ) ) ;
#38112 = CARTESIAN_POINT ( 'NONE',  ( -25.20123094555300369, 0.000000000000000000, 6.470945668149052032 ) ) ;
#38114 = ADVANCED_FACE ( 'NONE', ( #20622 ), #29114, .F. ) ;
#38113 = ORIENTED_EDGE ( 'NONE', *, *, #9891, .T. ) ;
#38115 = FACE_OUTER_BOUND ( 'NONE', #10032, .T. ) ;
#38116 = CARTESIAN_POINT ( 'NONE',  ( -11.57295624737693096, 0.2864062442990046309, 1.846691783222848882 ) ) ;
#38117 = DIRECTION ( 'NONE',  ( -0.5449076811759708816, 0.6444004775717707689, 0.5364919789714475140 ) ) ;
#38118 = DIRECTION ( 'NONE',  ( -0.005002170337468016433, -0.7660444431189770143, 0.6427681459581293666 ) ) ;
#38119 = ORIENTED_EDGE ( 'NONE', *, *, #7657, .F. ) ;
#38120 = EDGE_LOOP ( 'NONE', ( #46202, #17495, #1555, #23959 ) ) ;
#38121 = FACE_BOUND ( 'NONE', #45636, .T. ) ;
#38122 = ADVANCED_FACE ( 'NONE', ( #7539 ), #21158, .F. ) ;
#38123 = DIRECTION ( 'NONE',  ( 0.9999697198139515519, 0.000000000000000000, 0.007781995580013368816 ) ) ;
#38124 = CARTESIAN_POINT ( 'NONE',  ( -19.53735095677732403, 0.000000000000000000, 7.084361417893372703 ) ) ;
#38125 = LINE ( 'NONE', #28789, #12190 ) ;
#38126 = FACE_OUTER_BOUND ( 'NONE', #15527, .T. ) ;
#38127 = CARTESIAN_POINT ( 'NONE',  ( -10.47421230394850866, 0.000000000000000000, 10.95934586908605723 ) ) ;
#38128 = ORIENTED_EDGE ( 'NONE', *, *, #29047, .F. ) ;
#38129 = DIRECTION ( 'NONE',  ( 0.6427681459581294776, -0.7660444431189769032, 0.005002170337467562802 ) ) ;
#38130 = CARTESIAN_POINT ( 'NONE',  ( -14.41484887750424448, 0.000000000000000000, 5.646897634310420244 ) ) ;
#38131 = ORIENTED_EDGE ( 'NONE', *, *, #41517, .T. ) ;
#38132 = LINE ( 'NONE', #46099, #5069 ) ;
#38133 = ORIENTED_EDGE ( 'NONE', *, *, #42816, .T. ) ;
#38134 = CARTESIAN_POINT ( 'NONE',  ( -58.00000000000000711, 2.000000000000000000, 7.102951435054649637E-15 ) ) ;
#38135 = LINE ( 'NONE', #46360, #48729 ) ;
#38136 = CARTESIAN_POINT ( 'NONE',  ( -15.88053067323646417, -0.1191753592594197858, 2.950163842912994383 ) ) ;
#38137 = ADVANCED_FACE ( 'NONE', ( #38786 ), #46728, .F. ) ;
#38138 = PLANE ( 'NONE',  #16026 ) ;
#38139 = CARTESIAN_POINT ( 'NONE',  ( -68.27330710698295491, 2.000000000000001332, -8.536061506181777503 ) ) ;
#38140 = EDGE_LOOP ( 'NONE', ( #36357, #33014, #45404, #12835 ) ) ;
#38141 = VERTEX_POINT ( 'NONE', #33947 ) ;
#38142 = CARTESIAN_POINT ( 'NONE',  ( -69.10252959121689287, -0.6012852789374203422, 6.810182420670475523 ) ) ;
#38143 = CARTESIAN_POINT ( 'NONE',  ( -32.65919192261063841, -0.1191753592594197858, 9.467565677904410393 ) ) ;
#38144 = CARTESIAN_POINT ( 'NONE',  ( -22.40478740399063895, 0.000000000000000000, 5.384712028983816623 ) ) ;
#38145 = EDGE_CURVE ( 'NONE', #30915, #44660, #47012, .T. ) ;
#38146 = CARTESIAN_POINT ( 'NONE',  ( -14.66887761629205222, 0.000000000000000000, 12.58869632783390990 ) ) ;
#38147 = CARTESIAN_POINT ( 'NONE',  ( -21.47419595591918906, 0.000000000000000000, 5.222628093224860102 ) ) ;
#38148 = AXIS2_PLACEMENT_3D ( 'NONE', #34693, #17664, #4595 ) ;
#38149 = EDGE_CURVE ( 'NONE', #14066, #53756, #51813, .T. ) ;
#38150 = CARTESIAN_POINT ( 'NONE',  ( -22.40634380310664397, 0.000000000000000000, 5.584705972946605534 ) ) ;
#38151 = EDGE_LOOP ( 'NONE', ( #51385, #13294, #5955, #56186 ) ) ;
#38152 = CARTESIAN_POINT ( 'NONE',  ( -15.88688127818832463, -2.298917212465657833, 6.625850739918041299 ) ) ;
#38153 = ADVANCED_FACE ( 'NONE', ( #25422 ), #55812, .F. ) ;
#38154 = VECTOR ( 'NONE', #42041, 999.9999999999998863 ) ;
#38155 = FACE_OUTER_BOUND ( 'NONE', #7540, .T. ) ;
#38156 = CARTESIAN_POINT ( 'NONE',  ( -19.25678133725660501, 0.000000000000000000, 5.039878470293768231 ) ) ;
#38157 = VERTEX_POINT ( 'NONE', #47271 ) ;
#38158 = DIRECTION ( 'NONE',  ( 0.000000000000000000, -1.000000000000000000, 0.000000000000000000 ) ) ;
#38159 = FACE_OUTER_BOUND ( 'NONE', #33338, .T. ) ;
#38160 = DIRECTION ( 'NONE',  ( 0.007781995580012663651, 0.000000000000000000, -0.9999697198139515519 ) ) ;
#38161 = EDGE_CURVE ( 'NONE', #12315, #165, #31074, .T. ) ;
#38162 = VERTEX_POINT ( 'NONE', #13496 ) ;
#38163 = PLANE ( 'NONE',  #51924 ) ;
#38164 = ORIENTED_EDGE ( 'NONE', *, *, #39770, .F. ) ;
#38165 = EDGE_CURVE ( 'NONE', #17943, #47842, #4971, .T. ) ;
#38166 = ORIENTED_EDGE ( 'NONE', *, *, #45964, .F. ) ;
#38167 = ORIENTED_EDGE ( 'NONE', *, *, #635, .F. ) ;
#38168 = ORIENTED_EDGE ( 'NONE', *, *, #54064, .T. ) ;
#38169 = CARTESIAN_POINT ( 'NONE',  ( -13.17065887352947762, -0.1191753592594197858, 12.04635770780929427 ) ) ;
#38170 = ORIENTED_EDGE ( 'NONE', *, *, #29460, .F. ) ;
#38171 = CARTESIAN_POINT ( 'NONE',  ( -12.33635297242189921, 23.80382832886605726, -3.523096027145014464 ) ) ;
#38172 = VECTOR ( 'NONE', #56177, 1000.000000000000227 ) ;
#38173 = VECTOR ( 'NONE', #3108, 1000.000000000000227 ) ;
#38174 = ORIENTED_EDGE ( 'NONE', *, *, #25247, .T. ) ;
#38175 = DIRECTION ( 'NONE',  ( 0.005002170337468016433, -0.7660444431189770143, -0.6427681459581293666 ) ) ;
#38176 = ORIENTED_EDGE ( 'NONE', *, *, #35015, .T. ) ;
#38177 = ORIENTED_EDGE ( 'NONE', *, *, #52086, .T. ) ;
#38178 = DIRECTION ( 'NONE',  ( 0.6427681459581294776, -0.7660444431189769032, 0.005002170337467562802 ) ) ;
#38179 = CARTESIAN_POINT ( 'NONE',  ( -12.15271748404464880, 0.000000000000000000, 1.601849296007406664 ) ) ;
#38180 = DIRECTION ( 'NONE',  ( -0.005002170337468016433, -0.7660444431189770143, 0.6427681459581293666 ) ) ;
#38181 = FACE_OUTER_BOUND ( 'NONE', #936, .T. ) ;
#38182 = ORIENTED_EDGE ( 'NONE', *, *, #30659, .F. ) ;
#38183 = EDGE_LOOP ( 'NONE', ( #11512, #24823, #10178, #27799 ) ) ;
#38184 = AXIS2_PLACEMENT_3D ( 'NONE', #10759, #15018, #53897 ) ;
#38185 = LINE ( 'NONE', #24022, #45796 ) ;
#38186 = EDGE_CURVE ( 'NONE', #10812, #3022, #18289, .T. ) ;
#38187 = PLANE ( 'NONE',  #42081 ) ;
#38188 = VECTOR ( 'NONE', #46229, 999.9999999999998863 ) ;
#38189 = CARTESIAN_POINT ( 'NONE',  ( -19.51236138453683822, 1.419719901456505617, 4.215899037920694425 ) ) ;
#38190 = DIRECTION ( 'NONE',  ( 0.5364919789714477361, 0.6444004775717706579, 0.5449076811759711036 ) ) ;
#38191 = CARTESIAN_POINT ( 'NONE',  ( -17.65425454225471213, 0.000000000000000000, 3.944353494940506355 ) ) ;
#38192 = DIRECTION ( 'NONE',  ( 0.9321478471874540261, 0.000000000000000000, -0.3620778797217457101 ) ) ;
#38193 = ORIENTED_EDGE ( 'NONE', *, *, #17133, .T. ) ;
#38194 = LINE ( 'NONE', #51815, #55556 ) ;
#38195 = CARTESIAN_POINT ( 'NONE',  ( 5.488878199366571842, 0.000000000000000000, -2.420139938591586493 ) ) ;
#38196 = ORIENTED_EDGE ( 'NONE', *, *, #37393, .F. ) ;
#38197 = EDGE_CURVE ( 'NONE', #38808, #42624, #23136, .T. ) ;
#38198 = DIRECTION ( 'NONE',  ( -0.005002170337468016433, -0.7660444431189770143, 0.6427681459581293666 ) ) ;
#38199 = CARTESIAN_POINT ( 'NONE',  ( -22.40478740399063895, 0.000000000000000000, 5.384712028983816623 ) ) ;
#38200 = FACE_OUTER_BOUND ( 'NONE', #50070, .T. ) ;
#38201 = FACE_OUTER_BOUND ( 'NONE', #4618, .T. ) ;
#38202 = EDGE_CURVE ( 'NONE', #18181, #42292, #39632, .T. ) ;
#38203 = EDGE_CURVE ( 'NONE', #24571, #27123, #13217, .T. ) ;
#38204 = CARTESIAN_POINT ( 'NONE',  ( -16.74509912310952231, 0.000000000000000000, 6.536753241280876203 ) ) ;
#38205 = ORIENTED_EDGE ( 'NONE', *, *, #5515, .F. ) ;
#38206 = ORIENTED_EDGE ( 'NONE', *, *, #49562, .T. ) ;
#38207 = DIRECTION ( 'NONE',  ( 0.5449076811759707706, 0.6444004775717708799, -0.5364919789714476250 ) ) ;
#38208 = LINE ( 'NONE', #51291, #26771 ) ;
#38209 = CARTESIAN_POINT ( 'NONE',  ( -21.14151471908257562, 3.848249166794009746, 11.40903589015699815 ) ) ;
#38210 = VECTOR ( 'NONE', #21808, 999.9999999999998863 ) ;
#38211 = AXIS2_PLACEMENT_3D ( 'NONE', #24624, #15290, #41939 ) ;
#38212 = LINE ( 'NONE', #2717, #10133 ) ;
#38213 = EDGE_CURVE ( 'NONE', #47771, #54647, #30811, .T. ) ;
#38214 = CARTESIAN_POINT ( 'NONE',  ( -17.85293083182822116, 0.000000000000000000, 3.773481336529526775 ) ) ;
#38215 = DIRECTION ( 'NONE',  ( 0.000000000000000000, -1.000000000000000000, 0.000000000000000000 ) ) ;
#38216 = DIRECTION ( 'NONE',  ( 0.000000000000000000, -0.000000000000000000, -1.000000000000000000 ) ) ;
#38217 = EDGE_CURVE ( 'NONE', #6270, #5817, #8962, .T. ) ;
#38218 = CARTESIAN_POINT ( 'NONE',  ( -15.88053067323646417, -0.1191753592594197858, 2.950163842912994383 ) ) ;
#38219 = CARTESIAN_POINT ( 'NONE',  ( -65.88104832801796817, -9.249455602226623441, 1.512899686938066868 ) ) ;
#38220 = CARTESIAN_POINT ( 'NONE',  ( -14.14612558372896878, -4.079838673713159558, 8.872477635332897350 ) ) ;
#38221 = ORIENTED_EDGE ( 'NONE', *, *, #25608, .F. ) ;
#38222 = LINE ( 'NONE', #8141, #25021 ) ;
#38223 = EDGE_CURVE ( 'NONE', #14383, #39021, #48112, .T. ) ;
#38224 = ORIENTED_EDGE ( 'NONE', *, *, #52811, .T. ) ;
#38225 = ORIENTED_EDGE ( 'NONE', *, *, #38526, .T. ) ;
#38226 = VECTOR ( 'NONE', #22488, 1000.000000000000227 ) ;
#38227 = EDGE_CURVE ( 'NONE', #1987, #29115, #48398, .T. ) ;
#38228 = VERTEX_POINT ( 'NONE', #39884 ) ;
#38229 = EDGE_LOOP ( 'NONE', ( #8106, #6094, #30082, #18515 ) ) ;
#38230 = ORIENTED_EDGE ( 'NONE', *, *, #3433, .F. ) ;
#38231 = VERTEX_POINT ( 'NONE', #1252 ) ;
#38232 = PLANE ( 'NONE',  #49595 ) ;
#38233 = CARTESIAN_POINT ( 'NONE',  ( -15.88053067323646417, -0.1191753592594197858, 2.950163842912994383 ) ) ;
#38234 = CARTESIAN_POINT ( 'NONE',  ( -69.33786762168887208, -0.4146581964375588014, 7.487530722355575818 ) ) ;
#38235 = ORIENTED_EDGE ( 'NONE', *, *, #24153, .F. ) ;
#38236 = FACE_OUTER_BOUND ( 'NONE', #39678, .T. ) ;
#38237 = ORIENTED_EDGE ( 'NONE', *, *, #47856, .F. ) ;
#38238 = DIRECTION ( 'NONE',  ( -0.005961354470445682716, -0.6427876096865404731, 0.7660212471507180654 ) ) ;
#38239 = ORIENTED_EDGE ( 'NONE', *, *, #51013, .T. ) ;
#38240 = LINE ( 'NONE', #4469, #39260 ) ;
#38241 = CARTESIAN_POINT ( 'NONE',  ( -18.67775241435682432, 0.000000000000000000, 4.136394454059623804 ) ) ;
#38242 = DIRECTION ( 'NONE',  ( 0.005002170337468016433, -0.7660444431189770143, -0.6427681459581293666 ) ) ;
#38243 = ORIENTED_EDGE ( 'NONE', *, *, #10903, .F. ) ;
#38244 = CARTESIAN_POINT ( 'NONE',  ( -27.99767448711536133, 0.000000000000000000, 7.557179307314289218 ) ) ;
#38245 = ORIENTED_EDGE ( 'NONE', *, *, #35710, .F. ) ;
#38246 = AXIS2_PLACEMENT_3D ( 'NONE', #17781, #48130, #8133 ) ;
#38247 = VECTOR ( 'NONE', #35011, 1000.000000000000227 ) ;
#38248 = LINE ( 'NONE', #42786, #46388 ) ;
#38249 = EDGE_CURVE ( 'NONE', #6678, #21349, #52650, .T. ) ;
#38250 = CARTESIAN_POINT ( 'NONE',  ( -16.89925026227929195, -0.1191753592594197858, 13.49466922669627422 ) ) ;
#38251 = CARTESIAN_POINT ( 'NONE',  ( -9.933042293644859910, -0.002715256824217495563, 1.421395705359619122 ) ) ;
#38252 = AXIS2_PLACEMENT_3D ( 'NONE', #50349, #54890, #3494 ) ;
#38253 = DIRECTION ( 'NONE',  ( -0.005961354470445682716, -0.6427876096865404731, 0.7660212471507180654 ) ) ;
#38254 = FACE_BOUND ( 'NONE', #46490, .T. ) ;
#38255 = CARTESIAN_POINT ( 'NONE',  ( -68.45082166678818680, -0.05101588947699599308, -7.468518229136111408 ) ) ;
#38256 = CARTESIAN_POINT ( 'NONE',  ( -18.14188386713806267, 0.000000000000000000, 6.895215209234613063 ) ) ;
#38257 = CARTESIAN_POINT ( 'NONE',  ( -68.50231803695028532, -8.543494007632165932, -5.847034362371243965 ) ) ;
#38258 = EDGE_LOOP ( 'NONE', ( #36212, #33609, #27992, #22290 ) ) ;
#38259 = CARTESIAN_POINT ( 'NONE',  ( -56.48048524421252381, 6.632812770515467804, -2.293230480183058528 ) ) ;
#38260 = ORIENTED_EDGE ( 'NONE', *, *, #2850, .T. ) ;
#38261 = EDGE_CURVE ( 'NONE', #10471, #31963, #9218, .T. ) ;
#38262 = EDGE_CURVE ( 'NONE', #54647, #3649, #31661, .T. ) ;
#38263 = ADVANCED_FACE ( 'NONE', ( #44693 ), #9808, .F. ) ;
#38264 = DIRECTION ( 'NONE',  ( -0.005961354470445682716, -0.6427876096865404731, 0.7660212471507180654 ) ) ;
#38265 = CARTESIAN_POINT ( 'NONE',  ( -29.86197018149027116, 0.000000000000000000, 8.281335066757780083 ) ) ;
#38266 = DIRECTION ( 'NONE',  ( 0.5449076811759707706, 0.6444004775717708799, -0.5364919789714476250 ) ) ;
#38267 = VECTOR ( 'NONE', #48763, 1000.000000000000227 ) ;
#38268 = CARTESIAN_POINT ( 'NONE',  ( -11.15376843910079607, 0.000000000000000000, 4.564279906913194296 ) ) ;
#38269 = DIRECTION ( 'NONE',  ( 0.000000000000000000, -1.000000000000000000, 0.000000000000000000 ) ) ;
#38270 = VECTOR ( 'NONE', #5794, 1000.000000000000227 ) ;
#38271 = EDGE_CURVE ( 'NONE', #41467, #40214, #14050, .T. ) ;
#38272 = PLANE ( 'NONE',  #38288 ) ;
#38273 = VERTEX_POINT ( 'NONE', #43859 ) ;
#38274 = CARTESIAN_POINT ( 'NONE',  ( -12.20953538199096755, -0.1191753592594198830, 7.960971755595982025 ) ) ;
#38275 = LINE ( 'NONE', #38574, #34927 ) ;
#38276 = LINE ( 'NONE', #51362, #39976 ) ;
#38277 = CARTESIAN_POINT ( 'NONE',  ( -15.40103151951671734, 0.000000000000000000, 12.95233060667165681 ) ) ;
#38278 = EDGE_CURVE ( 'NONE', #17419, #32512, #42830, .T. ) ;
#38279 = LINE ( 'NONE', #55604, #39366 ) ;
#38280 = CARTESIAN_POINT ( 'NONE',  ( -16.81267852042391198, -0.1191753592594197858, 3.312241722634738039 ) ) ;
#38281 = DIRECTION ( 'NONE',  ( -0.005002170337468016433, -0.7660444431189770143, 0.6427681459581293666 ) ) ;
#38282 = EDGE_LOOP ( 'NONE', ( #8564, #32448, #52280 ) ) ;
#38283 = ADVANCED_FACE ( 'NONE', ( #40157 ), #21997, .F. ) ;
#38284 = DIRECTION ( 'NONE',  ( -0.005961354470445682716, -0.6427876096865404731, 0.7660212471507180654 ) ) ;
#38285 = PLANE ( 'NONE',  #28689 ) ;
#38286 = ORIENTED_EDGE ( 'NONE', *, *, #7013, .T. ) ;
#38287 = ADVANCED_FACE ( 'NONE', ( #22840 ), #20241, .F. ) ;
#38288 = AXIS2_PLACEMENT_3D ( 'NONE', #38008, #11864, #55060 ) ;
#38289 = ORIENTED_EDGE ( 'NONE', *, *, #31253, .F. ) ;
#38290 = CARTESIAN_POINT ( 'NONE',  ( 0.000000000000000000, 0.000000000000000000, 0.000000000000000000 ) ) ;
#38291 = VECTOR ( 'NONE', #50383, 999.9999999999998863 ) ;
#38292 = EDGE_CURVE ( 'NONE', #41711, #42294, #27962, .T. ) ;
#38293 = VECTOR ( 'NONE', #49087, 999.9999999999998863 ) ;
#38294 = EDGE_LOOP ( 'NONE', ( #29584, #50357, #20705, #20526 ) ) ;
#38295 = FACE_OUTER_BOUND ( 'NONE', #35680, .T. ) ;
#38296 = VECTOR ( 'NONE', #48499, 999.9999999999998863 ) ;
#38297 = VERTEX_POINT ( 'NONE', #49235 ) ;
#38298 = ORIENTED_EDGE ( 'NONE', *, *, #28128, .F. ) ;
#38299 = AXIS2_PLACEMENT_3D ( 'NONE', #13678, #27296, #44609 ) ;
#38300 = ORIENTED_EDGE ( 'NONE', *, *, #46289, .F. ) ;
#38301 = CARTESIAN_POINT ( 'NONE',  ( -16.33317936670417225, 0.000000000000000000, 13.31440848639340224 ) ) ;
#38302 = CARTESIAN_POINT ( 'NONE',  ( -65.06940864783059908, -9.156381468068820695, -0.6466721865750668652 ) ) ;
#38303 = DIRECTION ( 'NONE',  ( -0.5364919789714478471, 0.6444004775717705469, -0.5449076811759709926 ) ) ;
#38304 = VERTEX_POINT ( 'NONE', #27674 ) ;
#38305 = VECTOR ( 'NONE', #44148, 1000.000000000000000 ) ;
#38306 = ORIENTED_EDGE ( 'NONE', *, *, #45635, .T. ) ;
#38307 = CARTESIAN_POINT ( 'NONE',  ( -20.54049170961573267, 0.000000000000000000, 4.660556269540326646 ) ) ;
#38308 = FACE_OUTER_BOUND ( 'NONE', #129, .T. ) ;
#38309 = EDGE_LOOP ( 'NONE', ( #19467, #37617, #405, #33848 ) ) ;
#38310 = CARTESIAN_POINT ( 'NONE',  ( -12.15116108492864377, 0.000000000000000000, 1.401855352044617975 ) ) ;
#38311 = DIRECTION ( 'NONE',  ( -0.9999697198139514409, -0.000000000000000000, -0.007781995580013368816 ) ) ;
#38312 = EDGE_LOOP ( 'NONE', ( #40071, #47781, #40922, #49280 ) ) ;
#38313 = CARTESIAN_POINT ( 'NONE',  ( -1.086233639165236964, 0.000000000000000000, -2.796443541562362078 ) ) ;
#38314 = ADVANCED_FACE ( 'NONE', ( #19967 ), #10353, .F. ) ;
#38315 = ORIENTED_EDGE ( 'NONE', *, *, #20834, .T. ) ;
#38316 = LINE ( 'NONE', #7970, #55435 ) ;
#38317 = ADVANCED_FACE ( 'NONE', ( #37032 ), #10897, .F. ) ;
#38318 = AXIS2_PLACEMENT_3D ( 'NONE', #35109, #40170, #18299 ) ;
#38319 = LINE ( 'NONE', #56207, #27285 ) ;
#38320 = EDGE_LOOP ( 'NONE', ( #16362, #3406, #22709, #54099 ) ) ;
#38321 = DIRECTION ( 'NONE',  ( -0.05705673239519651330, 0.9983709377222391712, 2.351258244848514932E-16 ) ) ;
#38322 = LINE ( 'NONE', #34623, #45606 ) ;
#38323 = DIRECTION ( 'NONE',  ( 1.000000000000000000, 0.000000000000000000, 0.000000000000000000 ) ) ;
#38324 = AXIS2_PLACEMENT_3D ( 'NONE', #41315, #19986, #27984 ) ;
#38325 = CARTESIAN_POINT ( 'NONE',  ( -21.39391032317488595, -2.784623065533159636, 5.102598372062590038 ) ) ;
#38326 = ORIENTED_EDGE ( 'NONE', *, *, #22568, .T. ) ;
#38327 = EDGE_CURVE ( 'NONE', #8024, #1300, #6370, .T. ) ;
#38328 = EDGE_CURVE ( 'NONE', #21349, #23457, #24250, .T. ) ;
#38329 = ADVANCED_FACE ( 'NONE', ( #10657 ), #7204, .F. ) ;
#38330 = VECTOR ( 'NONE', #9042, 1000.000000000000114 ) ;
#38331 = VECTOR ( 'NONE', #38560, 1000.000000000000227 ) ;
#38332 = CARTESIAN_POINT ( 'NONE',  ( -13.09043773662596166, -2.298917212465658277, 5.539617100752805001 ) ) ;
#38333 = DIRECTION ( 'NONE',  ( 0.005002170337468016433, -0.7660444431189770143, -0.6427681459581293666 ) ) ;
#38334 = DIRECTION ( 'NONE',  ( 0.5449076811759707706, 0.6444004775717708799, -0.5364919789714476250 ) ) ;
#38335 = CARTESIAN_POINT ( 'NONE',  ( -61.56892328330737030, 6.937430383826147740, 2.999999999999993339 ) ) ;
#38336 = EDGE_CURVE ( 'NONE', #33080, #36001, #50056, .T. ) ;
#38337 = DIRECTION ( 'NONE',  ( 0.005961354470445682716, -0.6427876096865404731, -0.7660212471507180654 ) ) ;
#38338 = CARTESIAN_POINT ( 'NONE',  ( -18.67697421479882181, -0.1191753592594197858, 4.036397482078229793 ) ) ;
#38339 = AXIS2_PLACEMENT_3D ( 'NONE', #54359, #2410, #50089 ) ;
#38340 = CARTESIAN_POINT ( 'NONE',  ( -10.47421230394850866, 0.000000000000000000, 10.95934586908605723 ) ) ;
#38341 = VECTOR ( 'NONE', #38563, 1000.000000000000114 ) ;
#38342 = ORIENTED_EDGE ( 'NONE', *, *, #11573, .T. ) ;
#38343 = CARTESIAN_POINT ( 'NONE',  ( -67.84662069460095779, -4.914479465932832227E-13, 5.846634436083241404 ) ) ;
#38344 = VERTEX_POINT ( 'NONE', #45004 ) ;
#38345 = DIRECTION ( 'NONE',  ( 0.9999697198139515519, 0.000000000000000000, 0.007781995580013368816 ) ) ;
#38346 = CARTESIAN_POINT ( 'NONE',  ( 2.072287782118878319, 0.000000000000000000, -2.950529333540147015 ) ) ;
#38347 = CARTESIAN_POINT ( 'NONE',  ( -12.27573167061919079, 0.000000000000000000, 3.616878333782851840 ) ) ;
#38348 = VECTOR ( 'NONE', #35763, 999.9999999999998863 ) ;
#38349 = VECTOR ( 'NONE', #37127, 1000.000000000000000 ) ;
#38350 = CARTESIAN_POINT ( 'NONE',  ( -15.13495153988577968, 0.000000000000000000, 12.76973526769478084 ) ) ;
#38351 = EDGE_CURVE ( 'NONE', #26953, #12681, #21397, .T. ) ;
#38352 = CARTESIAN_POINT ( 'NONE',  ( -9.756983695072257490, 0.000000000000000000, 4.205817938959457436 ) ) ;
#38353 = VERTEX_POINT ( 'NONE', #6116 ) ;
#38354 = VERTEX_POINT ( 'NONE', #46095 ) ;
#38355 = EDGE_CURVE ( 'NONE', #3202, #31910, #41820, .T. ) ;
#38356 = CARTESIAN_POINT ( 'NONE',  ( -16.06709938707323460, 0.000000000000000000, 13.13181314741652628 ) ) ;
#38357 = DIRECTION ( 'NONE',  ( -0.3620778797217457101, 0.000000000000000000, -0.9321478471874540261 ) ) ;
#38358 = EDGE_LOOP ( 'NONE', ( #24367, #2152, #19754, #27512 ) ) ;
#38359 = VECTOR ( 'NONE', #20531, 1000.000000000000227 ) ;
#38360 = DIRECTION ( 'NONE',  ( -0.2588190451025212946, -0.9659258262890680902, 0.000000000000000000 ) ) ;
#38361 = ADVANCED_FACE ( 'NONE', ( #2910 ), #53767, .F. ) ;
#38362 = ORIENTED_EDGE ( 'NONE', *, *, #455, .F. ) ;
#38363 = CARTESIAN_POINT ( 'NONE',  ( -27.06708303904391144, 0.000000000000000000, 7.395095371555332697 ) ) ;
#38364 = VECTOR ( 'NONE', #5211, 999.9999999999998863 ) ;
#38365 = EDGE_LOOP ( 'NONE', ( #50507, #46698, #30120, #14382 ) ) ;
#38366 = LINE ( 'NONE', #29282, #1147 ) ;
#38367 = ADVANCED_FACE ( 'NONE', ( #40993 ), #2076, .F. ) ;
#38368 = ORIENTED_EDGE ( 'NONE', *, *, #51587, .T. ) ;
#38369 = ORIENTED_EDGE ( 'NONE', *, *, #10263, .T. ) ;
#38370 = ORIENTED_EDGE ( 'NONE', *, *, #9491, .F. ) ;
#38371 = LINE ( 'NONE', #43224, #22053 ) ;
#38372 = VECTOR ( 'NONE', #7715, 1000.000000000000227 ) ;
#38373 = DIRECTION ( 'NONE',  ( 0.000000000000000000, -0.000000000000000000, -1.000000000000000000 ) ) ;
#38374 = DIRECTION ( 'NONE',  ( -0.7660212471507179544, -0.6427876096865405842, -0.005961354470445141482 ) ) ;
#38375 = VECTOR ( 'NONE', #16351, 999.9999999999998863 ) ;
#38376 = AXIS2_PLACEMENT_3D ( 'NONE', #23957, #41564, #15429 ) ;
#38377 = FACE_OUTER_BOUND ( 'NONE', #39927, .T. ) ;
#38378 = ORIENTED_EDGE ( 'NONE', *, *, #18032, .T. ) ;
#38379 = ORIENTED_EDGE ( 'NONE', *, *, #41798, .F. ) ;
#38380 = VECTOR ( 'NONE', #24463, 1000.000000000000000 ) ;
#38381 = ORIENTED_EDGE ( 'NONE', *, *, #39120, .F. ) ;
#38382 = LINE ( 'NONE', #55353, #27745 ) ;
#38383 = VECTOR ( 'NONE', #16081, 999.9999999999998863 ) ;
#38384 = FACE_OUTER_BOUND ( 'NONE', #17935, .T. ) ;
#38385 = VERTEX_POINT ( 'NONE', #45813 ) ;
#38386 = LINE ( 'NONE', #55706, #47476 ) ;
#38387 = ORIENTED_EDGE ( 'NONE', *, *, #54692, .F. ) ;
#38388 = DIRECTION ( 'NONE',  ( 0.7660212471507180654, -0.6427876096865404731, 0.005961354470445141482 ) ) ;
#38389 = DIRECTION ( 'NONE',  ( 0.000000000000000000, -1.000000000000000000, 0.000000000000000000 ) ) ;
#38390 = ORIENTED_EDGE ( 'NONE', *, *, #25886, .F. ) ;
#38391 = LINE ( 'NONE', #13416, #50374 ) ;
#38392 = ORIENTED_EDGE ( 'NONE', *, *, #36620, .F. ) ;
#38393 = CARTESIAN_POINT ( 'NONE',  ( -1.086233639165236964, 0.000000000000000000, -2.796443541562362078 ) ) ;
#38394 = DIRECTION ( 'NONE',  ( -0.005961354470445682716, -0.6427876096865404731, 0.7660212471507180654 ) ) ;
#38395 = ORIENTED_EDGE ( 'NONE', *, *, #34918, .F. ) ;
#38396 = FACE_OUTER_BOUND ( 'NONE', #44138, .T. ) ;
#38397 = CARTESIAN_POINT ( 'NONE',  ( -25.20200914511100265, -0.1191753592594197858, 6.570942640130446932 ) ) ;
#38398 = FACE_OUTER_BOUND ( 'NONE', #12654, .T. ) ;
#38399 = CARTESIAN_POINT ( 'NONE',  ( -16.78942516689838271, -5.536956232915662746, 12.29060311582175835 ) ) ;
#38400 = VERTEX_POINT ( 'NONE', #40735 ) ;
#38401 = AXIS2_PLACEMENT_3D ( 'NONE', #22633, #36004, #53011 ) ;
#38402 = EDGE_CURVE ( 'NONE', #48148, #25259, #19710, .T. ) ;
#38403 = CARTESIAN_POINT ( 'NONE',  ( 0.3240706152708093812, -3.670543518250628967, -1.335466778558061241E-15 ) ) ;
#38404 = DIRECTION ( 'NONE',  ( -0.5364919789714478471, 0.6444004775717705469, -0.5449076811759709926 ) ) ;
#38405 = AXIS2_PLACEMENT_3D ( 'NONE', #33288, #50592, #7410 ) ;
#38406 = CARTESIAN_POINT ( 'NONE',  ( -16.61483718085185046, -4.241740624735661491, 10.09711774140462026 ) ) ;
#38407 = EDGE_CURVE ( 'NONE', #40878, #9942, #45265, .T. ) ;
#38408 = EDGE_CURVE ( 'NONE', #1901, #30787, #54072, .T. ) ;
#38409 = DIRECTION ( 'NONE',  ( 0.007781995580012663651, -3.146120232559066537E-19, -0.9999697198139514409 ) ) ;
#38410 = DIRECTION ( 'NONE',  ( -0.6427681459581293666, -0.7660444431189770143, -0.005002170337467561935 ) ) ;
#38411 = DIRECTION ( 'NONE',  ( -0.005961354470445682716, -0.6427876096865404731, 0.7660212471507180654 ) ) ;
#38412 = ORIENTED_EDGE ( 'NONE', *, *, #42055, .F. ) ;
#38413 = DIRECTION ( 'NONE',  ( -0.005961354470445682716, -0.6427876096865404731, 0.7660212471507180654 ) ) ;
#38414 = CARTESIAN_POINT ( 'NONE',  ( -16.81345671998191449, 0.000000000000000000, 3.412238694616132495 ) ) ;
#38415 = DIRECTION ( 'NONE',  ( 0.5364919789714477361, 0.6444004775717706579, 0.5449076811759711036 ) ) ;
#38416 = EDGE_LOOP ( 'NONE', ( #17650, #31124, #19614, #44970 ) ) ;
#38417 = AXIS2_PLACEMENT_3D ( 'NONE', #16298, #21701, #17413 ) ;
#38418 = LINE ( 'NONE', #51499, #44941 ) ;
#38419 = ORIENTED_EDGE ( 'NONE', *, *, #30615, .F. ) ;
#38420 = AXIS2_PLACEMENT_3D ( 'NONE', #54211, #45391, #15308 ) ;
#38421 = LINE ( 'NONE', #13153, #3519 ) ;
#38422 = LINE ( 'NONE', #26991, #27858 ) ;
#38423 = DIRECTION ( 'NONE',  ( -0.6427681459581293666, -0.7660444431189770143, -0.005002170337467561935 ) ) ;
#38424 = CARTESIAN_POINT ( 'NONE',  ( -67.63293690793081225, 0.1329915468650123000, 2.735910648338365725 ) ) ;
#38425 = ORIENTED_EDGE ( 'NONE', *, *, #51370, .T. ) ;
#38426 = VECTOR ( 'NONE', #13154, 999.9999999999998863 ) ;
#38427 = VECTOR ( 'NONE', #3070, 1000.000000000000114 ) ;
#38428 = ORIENTED_EDGE ( 'NONE', *, *, #44884, .F. ) ;
#38429 = CARTESIAN_POINT ( 'NONE',  ( 2.072287782118878319, 0.000000000000000000, -2.950529333540147015 ) ) ;
#38430 = CARTESIAN_POINT ( 'NONE',  ( -18.67619601524082285, 0.000000000000000000, 3.936400510096834893 ) ) ;
#38431 = FACE_OUTER_BOUND ( 'NONE', #3068, .T. ) ;
#38432 = CARTESIAN_POINT ( 'NONE',  ( -26.13415699229845757, -0.1191753592594197858, 6.933020519852192365 ) ) ;
#38433 = CARTESIAN_POINT ( 'NONE',  ( 2.072287782118878319, 0.000000000000000000, -2.950529333540147015 ) ) ;
#38434 = LINE ( 'NONE', #16567, #18570 ) ;
#38435 = ORIENTED_EDGE ( 'NONE', *, *, #22898, .T. ) ;
#38436 = LINE ( 'NONE', #25384, #47369 ) ;
#38437 = EDGE_CURVE ( 'NONE', #32717, #9189, #15702, .T. ) ;
#38438 = CARTESIAN_POINT ( 'NONE',  ( -63.00984630926864583, 1.788483511016180305, -3.000000000000007105 ) ) ;
#38439 = ORIENTED_EDGE ( 'NONE', *, *, #30492, .F. ) ;
#38440 = AXIS2_PLACEMENT_3D ( 'NONE', #25676, #34474, #87 ) ;
#38441 = EDGE_CURVE ( 'NONE', #46316, #41332, #42112, .T. ) ;
#38442 = DIRECTION ( 'NONE',  ( 0.007781995580012663651, 0.000000000000000000, -0.9999697198139515519 ) ) ;
#38443 = CARTESIAN_POINT ( 'NONE',  ( -15.39548367756490777, 5.305366725996510269, 11.56846045315015026 ) ) ;
#38444 = EDGE_CURVE ( 'NONE', #51932, #17026, #43163, .T. ) ;
#38445 = VECTOR ( 'NONE', #48960, 999.9999999999998863 ) ;
#38446 = LINE ( 'NONE', #20841, #8465 ) ;
#38447 = ORIENTED_EDGE ( 'NONE', *, *, #34209, .T. ) ;
#38448 = LINE ( 'NONE', #29687, #8532 ) ;
#38449 = EDGE_CURVE ( 'NONE', #40111, #33095, #33337, .T. ) ;
#38450 = AXIS2_PLACEMENT_3D ( 'NONE', #18091, #43102, #21533 ) ;
#38451 = EDGE_LOOP ( 'NONE', ( #13263, #39889, #9416, #31305 ) ) ;
#38452 = VERTEX_POINT ( 'NONE', #38130 ) ;
#38453 = ORIENTED_EDGE ( 'NONE', *, *, #36509, .F. ) ;
#38454 = ORIENTED_EDGE ( 'NONE', *, *, #53005, .T. ) ;
#38455 = AXIS2_PLACEMENT_3D ( 'NONE', #48869, #48280, #53138 ) ;
#38456 = PLANE ( 'NONE',  #38440 ) ;
#38457 = VERTEX_POINT ( 'NONE', #30179 ) ;
#38458 = CARTESIAN_POINT ( 'NONE',  ( -12.31198489147366715, 23.81789724696114519, -3.517870358740663672 ) ) ;
#38459 = ORIENTED_EDGE ( 'NONE', *, *, #25108, .F. ) ;
#38460 = LINE ( 'NONE', #16901, #20440 ) ;
#38461 = EDGE_LOOP ( 'NONE', ( #27938, #20515, #16841, #45803 ) ) ;
#38462 = ORIENTED_EDGE ( 'NONE', *, *, #13981, .F. ) ;
#38463 = VECTOR ( 'NONE', #22096, 1000.000000000000227 ) ;
#38464 = VECTOR ( 'NONE', #38800, 1000.000000000000227 ) ;
#38465 = DIRECTION ( 'NONE',  ( -0.6427681459581293666, -0.7660444431189770143, -0.005002170337467561935 ) ) ;
#38466 = DIRECTION ( 'NONE',  ( -0.5364919789714478471, 0.6444004775717705469, -0.5449076811759709926 ) ) ;
#38467 = CARTESIAN_POINT ( 'NONE',  ( -15.87975247367846166, 0.000000000000000000, 2.850166870931599927 ) ) ;
#38468 = CARTESIAN_POINT ( 'NONE',  ( -20.54126990917373519, -0.1191753592594197858, 4.760553241521720658 ) ) ;
#38469 = ADVANCED_FACE ( 'NONE', ( #51748 ), #7469, .F. ) ;
#38470 = DIRECTION ( 'NONE',  ( -0.9999697198139514409, -0.000000000000000000, -0.007781995580013368816 ) ) ;
#38471 = EDGE_LOOP ( 'NONE', ( #45362, #17889, #6215, #1526 ) ) ;
#38472 = EDGE_CURVE ( 'NONE', #5817, #17246, #46952, .T. ) ;
#38473 = ORIENTED_EDGE ( 'NONE', *, *, #8250, .F. ) ;
#38474 = CARTESIAN_POINT ( 'NONE',  ( 2.072287782118878319, 0.000000000000000000, -2.950529333540147015 ) ) ;
#38475 = DIRECTION ( 'NONE',  ( 0.9999697198139515519, 0.000000000000000000, 0.007781995580013368816 ) ) ;
#38476 = EDGE_CURVE ( 'NONE', #15150, #6764, #17127, .T. ) ;
#38477 = ADVANCED_FACE ( 'NONE', ( #16270 ), #20812, .F. ) ;
#38478 = LINE ( 'NONE', #34497, #6148 ) ;
#38479 = VECTOR ( 'NONE', #17515, 1000.000000000000114 ) ;
#38480 = CARTESIAN_POINT ( 'NONE',  ( -12.30602860478801830, 0.000000000000000000, 7.509969310323286074 ) ) ;
#38481 = AXIS2_PLACEMENT_3D ( 'NONE', #18795, #44595, #35270 ) ;
#38482 = CARTESIAN_POINT ( 'NONE',  ( -19.32961685222932147, 0.000000000000000000, 14.39908572644263351 ) ) ;
#38483 = CARTESIAN_POINT ( 'NONE',  ( -10.84028925556084388, -0.1191753592594197858, 11.14116300850493246 ) ) ;
#38484 = VERTEX_POINT ( 'NONE', #3504 ) ;
#38485 = CARTESIAN_POINT ( 'NONE',  ( -21.16434561149341675, -4.727446477803162850, 4.951441403346398928 ) ) ;
#38486 = PLANE ( 'NONE',  #9563 ) ;
#38487 = VECTOR ( 'NONE', #16763, 999.9999999999998863 ) ;
#38488 = ORIENTED_EDGE ( 'NONE', *, *, #47741, .T. ) ;
#38489 = PLANE ( 'NONE',  #15277 ) ;
#38490 = DIRECTION ( 'NONE',  ( 0.6427681459581294776, -0.7660444431189769032, 0.005002170337467562802 ) ) ;
#38491 = LINE ( 'NONE', #55249, #28662 ) ;
#38492 = LINE ( 'NONE', #11550, #39542 ) ;
#38493 = ADVANCED_FACE ( 'NONE', ( #51497 ), #42412, .F. ) ;
#38494 = ORIENTED_EDGE ( 'NONE', *, *, #28468, .F. ) ;
#38495 = VECTOR ( 'NONE', #54391, 1000.000000000000114 ) ;
#38496 = ORIENTED_EDGE ( 'NONE', *, *, #27999, .F. ) ;
#38497 = VECTOR ( 'NONE', #11057, 999.9999999999998863 ) ;
#38498 = LINE ( 'NONE', #46436, #18525 ) ;
#38499 = CARTESIAN_POINT ( 'NONE',  ( -18.86354292863559579, 0.000000000000000000, 14.21804678658176080 ) ) ;
#38500 = DIRECTION ( 'NONE',  ( -0.6427681459581293666, -0.7660444431189770143, -0.005002170337467561935 ) ) ;
#38501 = VECTOR ( 'NONE', #29773, 999.9999999999998863 ) ;
#38502 = DIRECTION ( 'NONE',  ( 0.6427681459581294776, -0.7660444431189769032, 0.005002170337467562802 ) ) ;
#38503 = DIRECTION ( 'NONE',  ( 0.005002170337468016433, -0.7660444431189770143, -0.6427681459581293666 ) ) ;
#38504 = LINE ( 'NONE', #12674, #50937 ) ;
#38505 = CARTESIAN_POINT ( 'NONE',  ( -16.99924723426068951, 0.000000000000000000, 13.49389102713827171 ) ) ;
#38506 = VECTOR ( 'NONE', #17989, 999.9999999999998863 ) ;
#38507 = DIRECTION ( 'NONE',  ( 0.000000000000000000, -1.000000000000000000, 0.000000000000000000 ) ) ;
#38508 = AXIS2_PLACEMENT_3D ( 'NONE', #21099, #50656, #11750 ) ;
#38509 = CARTESIAN_POINT ( 'NONE',  ( -70.27375990177029053, -9.753186304793430850, -9.798907322976864620 ) ) ;
#38510 = PLANE ( 'NONE',  #51911 ) ;
#38511 = EDGE_LOOP ( 'NONE', ( #13958, #42970, #8, #16991 ) ) ;
#38512 = DIRECTION ( 'NONE',  ( -0.5449076811759708816, 0.6444004775717707689, 0.5364919789714475140 ) ) ;
#38513 = EDGE_LOOP ( 'NONE', ( #18984, #6127, #21888, #15718 ) ) ;
#38514 = ADVANCED_FACE ( 'NONE', ( #12591 ), #46653, .F. ) ;
#38515 = VERTEX_POINT ( 'NONE', #21085 ) ;
#38516 = AXIS2_PLACEMENT_3D ( 'NONE', #15312, #10779, #6507 ) ;
#38517 = ORIENTED_EDGE ( 'NONE', *, *, #46948, .F. ) ;
#38518 = ORIENTED_EDGE ( 'NONE', *, *, #4003, .F. ) ;
#38519 = ORIENTED_EDGE ( 'NONE', *, *, #44656, .F. ) ;
#38520 = VECTOR ( 'NONE', #26439, 1000.000000000000227 ) ;
#38521 = VERTEX_POINT ( 'NONE', #25365 ) ;
#38522 = CARTESIAN_POINT ( 'NONE',  ( -20.06177075545399191, 0.000000000000000000, 14.76272000528038220 ) ) ;
#38523 = LINE ( 'NONE', #52149, #14811 ) ;
#38524 = DIRECTION ( 'NONE',  ( -0.9999697198139514409, -0.000000000000000000, -0.007781995580013368816 ) ) ;
#38525 = VECTOR ( 'NONE', #45007, 1000.000000000000227 ) ;
#38526 = EDGE_CURVE ( 'NONE', #46316, #14388, #12859, .T. ) ;
#38527 = VERTEX_POINT ( 'NONE', #12311 ) ;
#38528 = DIRECTION ( 'NONE',  ( -0.9999697198139514409, -0.000000000000000000, -0.007781995580013368816 ) ) ;
#38529 = ORIENTED_EDGE ( 'NONE', *, *, #22753, .F. ) ;
#38530 = VECTOR ( 'NONE', #5722, 1000.000000000000227 ) ;
#38531 = DIRECTION ( 'NONE',  ( -0.5364919789714478471, 0.6444004775717705469, -0.5449076811759709926 ) ) ;
#38532 = EDGE_CURVE ( 'NONE', #50552, #2262, #37577, .T. ) ;
#38533 = ORIENTED_EDGE ( 'NONE', *, *, #960, .F. ) ;
#38534 = EDGE_CURVE ( 'NONE', #40212, #8731, #29650, .T. ) ;
#38535 = VECTOR ( 'NONE', #12898, 1000.000000000000000 ) ;
#38536 = VECTOR ( 'NONE', #46033, 1000.000000000000227 ) ;
#38537 = DIRECTION ( 'NONE',  ( -0.9999697198139514409, -0.000000000000000000, -0.007781995580013368816 ) ) ;
#38538 = VECTOR ( 'NONE', #5404, 1000.000000000000000 ) ;
#38539 = VECTOR ( 'NONE', #12692, 1000.000000000000227 ) ;
#38540 = DIRECTION ( 'NONE',  ( 0.6427681459581294776, -0.7660444431189769032, 0.005002170337467562802 ) ) ;
#38541 = CARTESIAN_POINT ( 'NONE',  ( 4.930947970565944694, -1.129146301979397693, 1.967953638241001446 ) ) ;
#38542 = ADVANCED_FACE ( 'NONE', ( #55741 ), #47207, .F. ) ;
#38543 = ORIENTED_EDGE ( 'NONE', *, *, #44192, .F. ) ;
#38544 = CARTESIAN_POINT ( 'NONE',  ( -14.93495759592298988, 0.000000000000000000, 12.77129166681078409 ) ) ;
#38545 = ORIENTED_EDGE ( 'NONE', *, *, #32372, .F. ) ;
#38546 = CIRCLE ( 'NONE', #30368, 2.749999999999997335 ) ;
#38547 = PLANE ( 'NONE',  #19162 ) ;
#38548 = EDGE_CURVE ( 'NONE', #1131, #55375, #8610, .T. ) ;
#38549 = LINE ( 'NONE', #55879, #47484 ) ;
#38550 = EDGE_CURVE ( 'NONE', #10988, #24338, #54901, .T. ) ;
#38551 = VECTOR ( 'NONE', #35878, 1000.000000000000114 ) ;
#38552 = CARTESIAN_POINT ( 'NONE',  ( -12.70458494993575194, -0.1191753592594197858, 11.86531876794841978 ) ) ;
#38553 = AXIS2_PLACEMENT_3D ( 'NONE', #38474, #16916, #29961 ) ;
#38554 = LINE ( 'NONE', #47338, #50368 ) ;
#38555 = DIRECTION ( 'NONE',  ( 0.9999697198139515519, 0.000000000000000000, 0.007781995580013368816 ) ) ;
#38556 = DIRECTION ( 'NONE',  ( 0.9999697198139515519, 0.000000000000000000, 0.007781995580013368816 ) ) ;
#38557 = CARTESIAN_POINT ( 'NONE',  ( -20.96692673303604337, 2.553033558614007603, 9.215550515739858284 ) ) ;
#38558 = CARTESIAN_POINT ( 'NONE',  ( -10.88568941143365087, -10.49235224760979435, 1.009997871305523320 ) ) ;
#38559 = ORIENTED_EDGE ( 'NONE', *, *, #20968, .T. ) ;
#38560 = DIRECTION ( 'NONE',  ( -0.5449076811759708816, 0.6444004775717707689, 0.5364919789714475140 ) ) ;
#38561 = EDGE_LOOP ( 'NONE', ( #8652, #56191, #40711, #49143 ) ) ;
#38562 = EDGE_CURVE ( 'NONE', #10029, #43081, #24791, .T. ) ;
#38563 = DIRECTION ( 'NONE',  ( 0.5449076811759707706, 0.6444004775717708799, -0.5364919789714476250 ) ) ;
#38564 = CARTESIAN_POINT ( 'NONE',  ( -21.47419595591918906, 0.000000000000000000, 5.222628093224860102 ) ) ;
#38565 = CARTESIAN_POINT ( 'NONE',  ( -16.31670919488976779, -1.165603555308156736, 4.932849712129135256 ) ) ;
#38566 = DIRECTION ( 'NONE',  ( 0.9999697198139515519, 0.000000000000000000, 0.007781995580013368816 ) ) ;
#38567 = DIRECTION ( 'NONE',  ( 0.6427681459581294776, -0.7660444431189769032, 0.005002170337467562802 ) ) ;
#38568 = AXIS2_PLACEMENT_3D ( 'NONE', #50914, #55193, #20263 ) ;
#38569 = ADVANCED_FACE ( 'NONE', ( #48903 ), #35855, .F. ) ;
#38570 = DIRECTION ( 'NONE',  ( 0.6427681459581294776, -0.7660444431189769032, 0.005002170337467562802 ) ) ;
#38571 = VECTOR ( 'NONE', #50176, 1000.000000000000000 ) ;
#38572 = ORIENTED_EDGE ( 'NONE', *, *, #17293, .F. ) ;
#38573 = CARTESIAN_POINT ( 'NONE',  ( -19.60990026154428278, 0.000000000000000000, 4.498472333781370125 ) ) ;
#38574 = CARTESIAN_POINT ( 'NONE',  ( -16.06709938707323460, 0.000000000000000000, 13.13181314741652628 ) ) ;
#38575 = LINE ( 'NONE', #7088, #47229 ) ;
#38576 = VECTOR ( 'NONE', #54075, 1000.000000000000000 ) ;
#38577 = DIRECTION ( 'NONE',  ( 0.007781995580012662783, 0.000000000000000000, -0.9999697198139514409 ) ) ;
#38578 = VECTOR ( 'NONE', #18945, 1000.000000000000227 ) ;
#38579 = FACE_OUTER_BOUND ( 'NONE', #8208, .T. ) ;
#38580 = DIRECTION ( 'NONE',  ( 0.005002170337468016433, -0.7660444431189770143, -0.6427681459581293666 ) ) ;
#38581 = CARTESIAN_POINT ( 'NONE',  ( -16.97387228093712253, 4.495856970884011261, 3.131718784769318198 ) ) ;
#38582 = EDGE_LOOP ( 'NONE', ( #49946, #39679, #48523, #39365, #40299, #1761, #6029, #17777, #55528, #25008, #48803, #40246, #7214, #43476, #16533, #20204, #51859, #26726, #48539, #44968, #17278, #45215, #38996, #24296, #25398, #28540, #10742, #751, #39084, #146, #2040, #51644, #15742, #36039, #21906, #20924, #51277, #11408, #42797, #43740, #33230, #32390, #40134, #19945, #51530, #21333, #55332, #19230, #54187, #8871, #53307, #39191, #22679, #51972, #30843, #50490, #28943, #26218, #41283, #41170, #53121, #13123, #7294, #40087, #7790, #25749, #31700, #13472, #23414, #42623, #42557, #8118, #20242, #51493, #22726, #25327, #52633, #14602, #4949, #45895, #13035, #26597, #54658, #31039, #5024, #36703, #9629, #25402, #54788, #53526, #27084, #53673, #50904, #28390, #11447, #11339, #30156, #3119, #9843, #51098, #47538, #921, #51517 ) ) ;
#38583 = DIRECTION ( 'NONE',  ( -0.005961354470445682716, -0.6427876096865404731, 0.7660212471507180654 ) ) ;
#38584 = VECTOR ( 'NONE', #9977, 999.9999999999998863 ) ;
#38585 = DIRECTION ( 'NONE',  ( -0.5364919789714478471, 0.6444004775717705469, -0.5449076811759709926 ) ) ;
#38586 = CIRCLE ( 'NONE', #7735, 2.125000000000000000 ) ;
#38587 = EDGE_LOOP ( 'NONE', ( #14763, #45319, #14650, #36944 ) ) ;
#38588 = ORIENTED_EDGE ( 'NONE', *, *, #8336, .T. ) ;
#38589 = CARTESIAN_POINT ( 'NONE',  ( -16.53317331066696383, 0.000000000000000000, 13.31285208727739899 ) ) ;
#38590 = VECTOR ( 'NONE', #34873, 1000.000000000000227 ) ;
#38591 = ORIENTED_EDGE ( 'NONE', *, *, #12956, .T. ) ;
#38592 = VECTOR ( 'NONE', #15400, 1000.000000000000114 ) ;
#38593 = EDGE_CURVE ( 'NONE', #4269, #42201, #53178, .T. ) ;
#38594 = AXIS2_PLACEMENT_3D ( 'NONE', #23450, #37062, #50090 ) ;
#38595 = EDGE_LOOP ( 'NONE', ( #18498, #29827, #44429, #40695 ) ) ;
#38596 = AXIS2_PLACEMENT_3D ( 'NONE', #25630, #34183, #47496 ) ;
#38597 = VERTEX_POINT ( 'NONE', #903 ) ;
#38598 = ORIENTED_EDGE ( 'NONE', *, *, #26493, .F. ) ;
#38599 = DIRECTION ( 'NONE',  ( 0.9999697198139515519, 0.000000000000000000, 0.007781995580013368816 ) ) ;
#38600 = EDGE_LOOP ( 'NONE', ( #15483, #41500, #11471, #53118 ) ) ;
#38601 = CARTESIAN_POINT ( 'NONE',  ( -9.499406503593807116, 0.000000000000000000, 5.115812617421968689 ) ) ;
#38602 = DIRECTION ( 'NONE',  ( 0.5364919789714477361, 0.6444004775717706579, 0.5449076811759711036 ) ) ;
#38603 = ORIENTED_EDGE ( 'NONE', *, *, #27786, .T. ) ;
#38604 = VERTEX_POINT ( 'NONE', #13687 ) ;
#38605 = EDGE_CURVE ( 'NONE', #2042, #40517, #26761, .T. ) ;
#38606 = AXIS2_PLACEMENT_3D ( 'NONE', #49483, #18831, #31320 ) ;
#38607 = FACE_OUTER_BOUND ( 'NONE', #3457, .T. ) ;
#38608 = FACE_OUTER_BOUND ( 'NONE', #24069, .T. ) ;
#38609 = AXIS2_PLACEMENT_3D ( 'NONE', #27092, #52379, #8944 ) ;
#38610 = ORIENTED_EDGE ( 'NONE', *, *, #7137, .T. ) ;
#38611 = DIRECTION ( 'NONE',  ( -0.005002170337468016433, -0.7660444431189770143, 0.6427681459581293666 ) ) ;
#38612 = CARTESIAN_POINT ( 'NONE',  ( -28.93060053386082231, -0.1191753592594197858, 8.019254159017428663 ) ) ;
#38613 = ORIENTED_EDGE ( 'NONE', *, *, #49709, .T. ) ;
#38614 = VECTOR ( 'NONE', #12997, 1000.000000000000227 ) ;
#38615 = DIRECTION ( 'NONE',  ( 0.000000000000000000, -0.000000000000000000, -1.000000000000000000 ) ) ;
#38616 = ORIENTED_EDGE ( 'NONE', *, *, #49135, .T. ) ;
#38617 = CARTESIAN_POINT ( 'NONE',  ( 2.072287782118878319, 0.000000000000000000, -2.950529333540147015 ) ) ;
#38618 = ADVANCED_FACE ( 'NONE', ( #48320 ), #39558, .F. ) ;
#38619 = VECTOR ( 'NONE', #7687, 1000.000000000000227 ) ;
#38620 = EDGE_CURVE ( 'NONE', #14391, #45526, #35554, .T. ) ;
#38621 = CARTESIAN_POINT ( 'NONE',  ( -12.60458797795435615, 0.000000000000000000, 11.86609696750642229 ) ) ;
#38622 = AXIS2_PLACEMENT_3D ( 'NONE', #15033, #49677, #49092 ) ;
#38623 = VECTOR ( 'NONE', #6921, 1000.000000000000114 ) ;
#38624 = ORIENTED_EDGE ( 'NONE', *, *, #19148, .F. ) ;
#38625 = DIRECTION ( 'NONE',  ( -0.6427681459581293666, -0.7660444431189770143, -0.005002170337467561935 ) ) ;
#38626 = CARTESIAN_POINT ( 'NONE',  ( -15.60102546347950536, 0.000000000000000000, 12.95077420755565356 ) ) ;
#38627 = DIRECTION ( 'NONE',  ( 0.5364919789714477361, 0.6444004775717706579, 0.5449076811759711036 ) ) ;
#38628 = EDGE_CURVE ( 'NONE', #23457, #33064, #52864, .T. ) ;
#38629 = VECTOR ( 'NONE', #7536, 999.9999999999998863 ) ;
#38630 = CARTESIAN_POINT ( 'NONE',  ( -21.47419595591918906, 0.000000000000000000, 5.222628093224860102 ) ) ;
#38631 = ORIENTED_EDGE ( 'NONE', *, *, #3653, .T. ) ;
#38632 = VECTOR ( 'NONE', #8061, 999.9999999999998863 ) ;
#38633 = EDGE_CURVE ( 'NONE', #38231, #48589, #21927, .T. ) ;
#38634 = VECTOR ( 'NONE', #20014, 1000.000000000000227 ) ;
#38635 = DIRECTION ( 'NONE',  ( 0.5449076811759707706, 0.6444004775717708799, -0.5364919789714476250 ) ) ;
#38636 = DIRECTION ( 'NONE',  ( -0.5364919789714478471, 0.6444004775717705469, -0.5449076811759709926 ) ) ;
#38637 = CARTESIAN_POINT ( 'NONE',  ( -12.07573772665640099, 0.000000000000000000, 3.618434732898855977 ) ) ;
#38638 = FACE_OUTER_BOUND ( 'NONE', #21074, .T. ) ;
#38639 = CARTESIAN_POINT ( 'NONE',  ( -13.73672976910459909, 0.000000000000000000, 12.22661844811216270 ) ) ;
#38640 = LINE ( 'NONE', #41744, #2501 ) ;
#38641 = VECTOR ( 'NONE', #40637, 1000.000000000000000 ) ;
#38642 = EDGE_CURVE ( 'NONE', #29025, #18181, #27048, .T. ) ;
#38643 = VECTOR ( 'NONE', #44240, 999.9999999999998863 ) ;
#38644 = DIRECTION ( 'NONE',  ( 0.000000000000000000, -1.000000000000000000, 0.000000000000000000 ) ) ;
#38645 = CARTESIAN_POINT ( 'NONE',  ( -16.81267852042391198, -0.1191753592594197858, 3.312241722634738039 ) ) ;
#38646 = ORIENTED_EDGE ( 'NONE', *, *, #34159, .T. ) ;
#38647 = CARTESIAN_POINT ( 'NONE',  ( -16.46189419481024885, 0.000000000000000000, 4.153638775091319957 ) ) ;
#38648 = ORIENTED_EDGE ( 'NONE', *, *, #36940, .F. ) ;
#38649 = PLANE ( 'NONE',  #39283 ) ;
#38650 = CARTESIAN_POINT ( 'NONE',  ( 2.072287782118878319, 0.000000000000000000, -2.950529333540147015 ) ) ;
#38651 = LINE ( 'NONE', #51127, #53979 ) ;
#38652 = DIRECTION ( 'NONE',  ( -0.8531650599175529814, -0.4028455766673920135, 0.3313982828793697877 ) ) ;
#38653 = FACE_OUTER_BOUND ( 'NONE', #15135, .T. ) ;
#38654 = VECTOR ( 'NONE', #34273, 999.9999999999998863 ) ;
#38655 = EDGE_LOOP ( 'NONE', ( #22880, #1001, #46243, #17666 ) ) ;
#38656 = ORIENTED_EDGE ( 'NONE', *, *, #29460, .T. ) ;
#38657 = PLANE ( 'NONE',  #26814 ) ;
#38658 = CARTESIAN_POINT ( 'NONE',  ( -3.941126747678045827, 5.958485271846477360, -1.687506105637922360 ) ) ;
#38659 = ORIENTED_EDGE ( 'NONE', *, *, #36359, .F. ) ;
#38660 = AXIS2_PLACEMENT_3D ( 'NONE', #33589, #33879, #8054 ) ;
#38661 = EDGE_CURVE ( 'NONE', #428, #16370, #13973, .T. ) ;
#38662 = B_SPLINE_CURVE_WITH_KNOTS ( 'NONE', 3,
 ( #48970, #26544, #23142, #23425, #1562, #52655, #49244, #27117, #18594, #44167, #1809, #53260, #10358, #22308, #26842, #5271, #35943, #14354, #45010, #18888, #6121, #31667, #40471, #53507, #30816, #22581, #970, #44422 ),
 .UNSPECIFIED., .F., .F.,
 ( 4, 2, 2, 2, 2, 2, 2, 2, 2, 2, 2, 2, 2, 4 ),
 ( 7.806255641895624221E-18, 0.002014507434814107479, 0.004029014869628207152, 0.006043522304442306391, 0.007050776021849359046, 0.008058029739256412569, 0.009065283456663466091, 0.01007253717407051788, 0.01208704460888462319, 0.01309429832629167845, 0.01410155204369873023, 0.01510880576110578376, 0.01561243261980931225, 0.01611605947851283901 ),
 .UNSPECIFIED. ) ;
#38663 = CARTESIAN_POINT ( 'NONE',  ( -21.47419595591918906, 0.000000000000000000, 5.222628093224860102 ) ) ;
#38664 = ORIENTED_EDGE ( 'NONE', *, *, #43413, .T. ) ;
#38665 = LINE ( 'NONE', #288, #18617 ) ;
#38666 = VECTOR ( 'NONE', #3780, 1000.000000000000227 ) ;
#38667 = EDGE_CURVE ( 'NONE', #13188, #9765, #30482, .T. ) ;
#38668 = VERTEX_POINT ( 'NONE', #5457 ) ;
#38669 = CARTESIAN_POINT ( 'NONE',  ( -9.965599799550892257, 0.000000000000000000, 5.312190649616747251 ) ) ;
#38670 = VECTOR ( 'NONE', #37102, 1000.000000000000227 ) ;
#38671 = ORIENTED_EDGE ( 'NONE', *, *, #55505, .T. ) ;
#38672 = ORIENTED_EDGE ( 'NONE', *, *, #33372, .F. ) ;
#38673 = ORIENTED_EDGE ( 'NONE', *, *, #6738, .T. ) ;
#38674 = ADVANCED_FACE ( 'NONE', ( #22771 ), #40091, .F. ) ;
#38675 = CARTESIAN_POINT ( 'NONE',  ( -10.69487964927027868, 0.000000000000000000, 5.306515225196732466 ) ) ;
#38676 = LINE ( 'NONE', #3724, #29610 ) ;
#38677 = LINE ( 'NONE', #38094, #39355 ) ;
#38678 = EDGE_CURVE ( 'NONE', #51439, #5375, #21671, .T. ) ;
#38679 = AXIS2_PLACEMENT_3D ( 'NONE', #10948, #46712, #25154 ) ;
#38680 = EDGE_CURVE ( 'NONE', #55993, #1154, #17386, .T. ) ;
#38681 = EDGE_CURVE ( 'NONE', #39497, #16451, #13149, .T. ) ;
#38682 = VECTOR ( 'NONE', #47193, 1000.000000000000000 ) ;
#38683 = DIRECTION ( 'NONE',  ( -0.005961354470445682716, -0.6427876096865404731, 0.7660212471507180654 ) ) ;
#38684 = ORIENTED_EDGE ( 'NONE', *, *, #475, .T. ) ;
#38685 = ORIENTED_EDGE ( 'NONE', *, *, #10711, .T. ) ;
#38686 = VECTOR ( 'NONE', #42229, 999.9999999999998863 ) ;
#38687 = VECTOR ( 'NONE', #26275, 1000.000000000000114 ) ;
#38688 = VERTEX_POINT ( 'NONE', #26209 ) ;
#38689 = CARTESIAN_POINT ( 'NONE',  ( -15.31350409040604887, -1.651309408375657206, 2.776920739002065819 ) ) ;
#38690 = CARTESIAN_POINT ( 'NONE',  ( 2.072287782118878319, 0.000000000000000000, -2.950529333540147015 ) ) ;
#38691 = VERTEX_POINT ( 'NONE', #43512 ) ;
#38692 = DIRECTION ( 'NONE',  ( -0.9335804264972049626, 0.3583679495452921082, 0.000000000000000000 ) ) ;
#38693 = VERTEX_POINT ( 'NONE', #4614 ) ;
#38694 = LINE ( 'NONE', #42383, #30566 ) ;
#38695 = DIRECTION ( 'NONE',  ( 0.9999697198139515519, 0.000000000000000000, 0.007781995580013368816 ) ) ;
#38696 = ORIENTED_EDGE ( 'NONE', *, *, #35043, .T. ) ;
#38697 = CARTESIAN_POINT ( 'NONE',  ( -11.47086027511496731, 1.257817950434005461, 3.401286344105265869 ) ) ;
#38698 = EDGE_CURVE ( 'NONE', #30522, #42624, #39255, .T. ) ;
#38699 = ORIENTED_EDGE ( 'NONE', *, *, #23298, .T. ) ;
#38700 = EDGE_CURVE ( 'NONE', #17943, #16783, #52335, .T. ) ;
#38701 = VECTOR ( 'NONE', #36963, 999.9999999999998863 ) ;
#38702 = ADVANCED_FACE ( 'NONE', ( #4900 ), #685, .F. ) ;
#38703 = DIRECTION ( 'NONE',  ( 0.005002170337468016433, -0.7660444431189770143, -0.6427681459581293666 ) ) ;
#38704 = DIRECTION ( 'NONE',  ( -0.5449076811759708816, 0.6444004775717707689, 0.5364919789714475140 ) ) ;
#38705 = ORIENTED_EDGE ( 'NONE', *, *, #16183, .T. ) ;
#38706 = CARTESIAN_POINT ( 'NONE',  ( -11.22056963685719211, 0.000000000000000000, 1.239771416285661010 ) ) ;
#38707 = DIRECTION ( 'NONE',  ( 0.5364919789714477361, 0.6444004775717706579, 0.5449076811759711036 ) ) ;
#38708 = EDGE_CURVE ( 'NONE', #37378, #9864, #28993, .T. ) ;
#38709 = PLANE ( 'NONE',  #45496 ) ;
#38710 = VERTEX_POINT ( 'NONE', #47142 ) ;
#38711 = EDGE_CURVE ( 'NONE', #29528, #43061, #51122, .T. ) ;
#38712 = DIRECTION ( 'NONE',  ( 0.6427681459581294776, -0.7660444431189769032, 0.005002170337467562802 ) ) ;
#38713 = VECTOR ( 'NONE', #49825, 1000.000000000000000 ) ;
#38714 = DIRECTION ( 'NONE',  ( 0.2113248654051873565, 0.7886751345948121994, -0.5773502691896263972 ) ) ;
#38715 = CARTESIAN_POINT ( 'NONE',  ( -26.13337879274045505, 0.000000000000000000, 6.833023547870798353 ) ) ;
#38716 = LINE ( 'NONE', #48048, #3102 ) ;
#38717 = EDGE_CURVE ( 'NONE', #56109, #55993, #42882, .T. ) ;
#38718 = DIRECTION ( 'NONE',  ( 0.007781995580012663651, 0.000000000000000000, -0.9999697198139515519 ) ) ;
#38719 = VECTOR ( 'NONE', #28501, 1000.000000000000000 ) ;
#38720 = DIRECTION ( 'NONE',  ( -0.6427681459581293666, -0.7660444431189770143, -0.005002170337467561935 ) ) ;
#38721 = ORIENTED_EDGE ( 'NONE', *, *, #36066, .F. ) ;
#38722 = PLANE ( 'NONE',  #32552 ) ;
#38723 = CARTESIAN_POINT ( 'NONE',  ( 5.211213849286742139, 0.000000000000000000, -2.388555951666874844 ) ) ;
#38724 = DIRECTION ( 'NONE',  ( 0.007781995580012663651, 0.000000000000000000, -0.9999697198139515519 ) ) ;
#38725 = ORIENTED_EDGE ( 'NONE', *, *, #15380, .T. ) ;
#38726 = DIRECTION ( 'NONE',  ( 0.007781995580012662783, 0.000000000000000000, -0.9999697198139514409 ) ) ;
#38727 = LINE ( 'NONE', #46800, #38614 ) ;
#38728 = ORIENTED_EDGE ( 'NONE', *, *, #43846, .T. ) ;
#38729 = PLANE ( 'NONE',  #49768 ) ;
#38730 = LINE ( 'NONE', #55746, #26037 ) ;
#38731 = VECTOR ( 'NONE', #17829, 999.9999999999998863 ) ;
#38732 = PLANE ( 'NONE',  #22362 ) ;
#38733 = CARTESIAN_POINT ( 'NONE',  ( -66.79351738431421381, 1.999999999999980460, 6.196202711026808529 ) ) ;
#38734 = ORIENTED_EDGE ( 'NONE', *, *, #30277, .F. ) ;
#38735 = VECTOR ( 'NONE', #17919, 1000.000000000000227 ) ;
#38736 = EDGE_LOOP ( 'NONE', ( #30579, #1686, #27142, #47143 ) ) ;
#38737 = LINE ( 'NONE', #55460, #12196 ) ;
#38738 = DIRECTION ( 'NONE',  ( 0.007781995580012663651, 0.000000000000000000, -0.9999697198139515519 ) ) ;
#38739 = CARTESIAN_POINT ( 'NONE',  ( -13.53673582514181106, 0.000000000000000000, 12.22817484722816772 ) ) ;
#38740 = CARTESIAN_POINT ( 'NONE',  ( -12.09585610119338028, 0.000000000000000000, 6.203602655703208235 ) ) ;
#38741 = DIRECTION ( 'NONE',  ( 0.005002170337468016433, -0.7660444431189770143, -0.6427681459581293666 ) ) ;
#38742 = CARTESIAN_POINT ( 'NONE',  ( -26.13493519185646008, 0.000000000000000000, 7.033017491833586377 ) ) ;
#38743 = EDGE_LOOP ( 'NONE', ( #51185, #20883, #31308, #38829 ) ) ;
#38744 = DIRECTION ( 'NONE',  ( 0.7660212471507180654, -0.6427876096865404731, 0.005961354470445141482 ) ) ;
#38745 = VECTOR ( 'NONE', #1150, 999.9999999999998863 ) ;
#38746 = CARTESIAN_POINT ( 'NONE',  ( -17.26532721389163072, 0.000000000000000000, 13.67648636611514590 ) ) ;
#38747 = ORIENTED_EDGE ( 'NONE', *, *, #24140, .T. ) ;
#38748 = FACE_OUTER_BOUND ( 'NONE', #12886, .T. ) ;
#38749 = LINE ( 'NONE', #55772, #10524 ) ;
#38750 = PLANE ( 'NONE',  #21185 ) ;
#38751 = EDGE_CURVE ( 'NONE', #50517, #44961, #46290, .T. ) ;
#38752 = ADVANCED_FACE ( 'NONE', ( #2839 ), #46576, .F. ) ;
#38753 = ORIENTED_EDGE ( 'NONE', *, *, #36562, .F. ) ;
#38754 = CARTESIAN_POINT ( 'NONE',  ( -20.03163450426368541, -1.165603555308156514, 4.625099379789840981 ) ) ;
#38755 = VECTOR ( 'NONE', #9462, 1000.000000000000227 ) ;
#38756 = ORIENTED_EDGE ( 'NONE', *, *, #6060, .F. ) ;
#38757 = ADVANCED_FACE ( 'NONE', ( #8246 ), #25560, .F. ) ;
#38758 = EDGE_LOOP ( 'NONE', ( #53213, #2433, #40354, #9068 ) ) ;
#38759 = VECTOR ( 'NONE', #40472, 1000.000000000000227 ) ;
#38760 = ORIENTED_EDGE ( 'NONE', *, *, #51382, .T. ) ;
#38761 = ORIENTED_EDGE ( 'NONE', *, *, #52916, .F. ) ;
#38762 = CARTESIAN_POINT ( 'NONE',  ( -16.48077548314530461, 3.848249166794009746, 9.598646491548270987 ) ) ;
#38763 = ORIENTED_EDGE ( 'NONE', *, *, #45467, .F. ) ;
#38764 = LINE ( 'NONE', #17734, #36716 ) ;
#38765 = VECTOR ( 'NONE', #18285, 1000.000000000000227 ) ;
#38766 = VERTEX_POINT ( 'NONE', #38647 ) ;
#38767 = CARTESIAN_POINT ( 'NONE',  ( -11.13054826722768098, 24.50000000000005684, 5.000000000000000000 ) ) ;
#38768 = ORIENTED_EDGE ( 'NONE', *, *, #28373, .T. ) ;
#38769 = LINE ( 'NONE', #13196, #31076 ) ;
#38770 = ORIENTED_EDGE ( 'NONE', *, *, #480, .F. ) ;
#38771 = CARTESIAN_POINT ( 'NONE',  ( -19.63082162219014748, -0.1191753592594168992, 6.244966839838443917 ) ) ;
#38772 = LINE ( 'NONE', #43564, #11421 ) ;
#38773 = CARTESIAN_POINT ( 'NONE',  ( -19.50285499688518343, 4.657758921906511418, 12.10106822468943655 ) ) ;
#38774 = DIRECTION ( 'NONE',  ( 0.000000000000000000, -1.000000000000000000, 0.000000000000000000 ) ) ;
#38775 = DIRECTION ( 'NONE',  ( 0.005961354470445682716, -0.6427876096865404731, -0.7660212471507180654 ) ) ;
#38776 = ORIENTED_EDGE ( 'NONE', *, *, #34825, .F. ) ;
#38778 = VERTEX_POINT ( 'NONE', #29574 ) ;
#38777 = ADVANCED_FACE ( 'NONE', ( #55377 ), #16475, .F. ) ;
#38779 = CARTESIAN_POINT ( 'NONE',  ( -27.06708303904391144, 0.000000000000000000, 7.395095371555332697 ) ) ;
#38780 = DIRECTION ( 'NONE',  ( 0.6427681459581294776, -0.7660444431189769032, 0.005002170337467562802 ) ) ;
#38781 = EDGE_CURVE ( 'NONE', #39543, #5013, #15937, .T. ) ;
#38782 = PLANE ( 'NONE',  #8857 ) ;
#38783 = DIRECTION ( 'NONE',  ( -0.7660212471507179544, -0.6427876096865405842, -0.005961354470445141482 ) ) ;
#38784 = EDGE_CURVE ( 'NONE', #35551, #6162, #24443, .T. ) ;
#38785 = CARTESIAN_POINT ( 'NONE',  ( 2.072287782118878319, 0.000000000000000000, -2.950529333540147015 ) ) ;
#38786 = FACE_OUTER_BOUND ( 'NONE', #52974, .T. ) ;
#38787 = VERTEX_POINT ( 'NONE', #11675 ) ;
#38788 = LINE ( 'NONE', #38485, #32944 ) ;
#38789 = EDGE_CURVE ( 'NONE', #49206, #55415, #16211, .T. ) ;
#38790 = CARTESIAN_POINT ( 'NONE',  ( -18.25036719564678123, 1.581621852479005774, 3.720532117565352070 ) ) ;
#38791 = ORIENTED_EDGE ( 'NONE', *, *, #17132, .F. ) ;
#38792 = DIRECTION ( 'NONE',  ( 0.6427681459581294776, -0.7660444431189769032, 0.005002170337467562802 ) ) ;
#38793 = CARTESIAN_POINT ( 'NONE',  ( -10.69619730365955945, 0.000000000000000000, 5.475830984491707909 ) ) ;
#38794 = ADVANCED_FACE ( 'NONE', ( #50837 ), #29261, .F. ) ;
#38795 = CARTESIAN_POINT ( 'NONE',  ( -18.67775241435682432, 0.000000000000000000, 4.136394454059623804 ) ) ;
#38796 = CARTESIAN_POINT ( 'NONE',  ( -17.74404816805336793, 0.000000000000000000, 3.574322630375089460 ) ) ;
#38797 = VECTOR ( 'NONE', #52121, 999.9999999999998863 ) ;
#38798 = ORIENTED_EDGE ( 'NONE', *, *, #21281, .T. ) ;
#38799 = VERTEX_POINT ( 'NONE', #17611 ) ;
#38800 = DIRECTION ( 'NONE',  ( -0.5449076811759708816, 0.6444004775717707689, 0.5364919789714475140 ) ) ;
#38801 = DIRECTION ( 'NONE',  ( -0.9999697198139514409, -0.000000000000000000, -0.007781995580013368816 ) ) ;
#38802 = DIRECTION ( 'NONE',  ( 0.9999697198139515519, 0.000000000000000000, 0.007781995580013368816 ) ) ;
#38803 = AXIS2_PLACEMENT_3D ( 'NONE', #40667, #40919, #32433 ) ;
#38804 = DIRECTION ( 'NONE',  ( 0.7660212471507180654, -0.6427876096865404731, 0.005961354470445141482 ) ) ;
#38805 = PLANE ( 'NONE',  #7661 ) ;
#38806 = LINE ( 'NONE', #43349, #25530 ) ;
#38807 = CARTESIAN_POINT ( 'NONE',  ( -25.83278826518980154, 17.74370858705499288, -4.604226652742015702 ) ) ;
#38808 = VERTEX_POINT ( 'NONE', #38922 ) ;
#38809 = DIRECTION ( 'NONE',  ( 0.9999697198139515519, 0.000000000000000000, 0.007781995580013368816 ) ) ;
#38810 = LINE ( 'NONE', #17481, #11509 ) ;
#38811 = ORIENTED_EDGE ( 'NONE', *, *, #7859, .F. ) ;
#38812 = CARTESIAN_POINT ( 'NONE',  ( -16.82487927491429502, -0.1134144341942024126, 3.316980910018160422 ) ) ;
#38813 = ORIENTED_EDGE ( 'NONE', *, *, #11205, .F. ) ;
#38814 = LINE ( 'NONE', #16647, #52170 ) ;
#38815 = EDGE_CURVE ( 'NONE', #14388, #4025, #30939, .T. ) ;
#38816 = ORIENTED_EDGE ( 'NONE', *, *, #23093, .T. ) ;
#38817 = ORIENTED_EDGE ( 'NONE', *, *, #49424, .T. ) ;
#38818 = EDGE_CURVE ( 'NONE', #22139, #1353, #40022, .T. ) ;
#38819 = EDGE_CURVE ( 'NONE', #8289, #30652, #8535, .T. ) ;
#38820 = ORIENTED_EDGE ( 'NONE', *, *, #53779, .T. ) ;
#38821 = EDGE_LOOP ( 'NONE', ( #28919, #1648, #32981, #40854 ) ) ;
#38822 = ORIENTED_EDGE ( 'NONE', *, *, #1025, .F. ) ;
#38823 = ORIENTED_EDGE ( 'NONE', *, *, #54553, .F. ) ;
#38824 = LINE ( 'NONE', #38522, #30549 ) ;
#38825 = PLANE ( 'NONE',  #19337 ) ;
#38826 = CARTESIAN_POINT ( 'NONE',  ( -22.40556560354864146, -0.1191753592594197858, 5.484709000965211523 ) ) ;
#38827 = ORIENTED_EDGE ( 'NONE', *, *, #6218, .T. ) ;
#38828 = FACE_OUTER_BOUND ( 'NONE', #31793, .T. ) ;
#38829 = ORIENTED_EDGE ( 'NONE', *, *, #24306, .F. ) ;
#38830 = CARTESIAN_POINT ( 'NONE',  ( -18.62089103150555758, 0.000000000000000000, 8.738147813755425375 ) ) ;
#38831 = ORIENTED_EDGE ( 'NONE', *, *, #4133, .F. ) ;
#38832 = EDGE_CURVE ( 'NONE', #37067, #11552, #1107, .T. ) ;
#38833 = DIRECTION ( 'NONE',  ( 0.007781995580012663651, 0.000000000000000000, -0.9999697198139515519 ) ) ;
#38834 = DIRECTION ( 'NONE',  ( 0.6427681459581294776, -0.7660444431189769032, 0.005002170337467562802 ) ) ;
#38835 = DIRECTION ( 'NONE',  ( 0.9999697198139515519, 0.000000000000000000, 0.007781995580013368816 ) ) ;
#38836 = ORIENTED_EDGE ( 'NONE', *, *, #10738, .F. ) ;
#38837 = FACE_OUTER_BOUND ( 'NONE', #32588, .T. ) ;
#38838 = EDGE_LOOP ( 'NONE', ( #28119, #42827, #17967, #11043 ) ) ;
#38839 = AXIS2_PLACEMENT_3D ( 'NONE', #8836, #52790, #13619 ) ;
#38840 = CARTESIAN_POINT ( 'NONE',  ( -11.82561389535573682, 3.362543313726509719, 1.168119031430539634 ) ) ;
#38841 = DIRECTION ( 'NONE',  ( -0.005002170337468016433, -0.7660444431189770143, 0.6427681459581293666 ) ) ;
#38842 = EDGE_CURVE ( 'NONE', #39505, #93, #34639, .T. ) ;
#38843 = LINE ( 'NONE', #47636, #15134 ) ;
#38844 = PLANE ( 'NONE',  #44001 ) ;
#38845 = FACE_OUTER_BOUND ( 'NONE', #46525, .T. ) ;
#38846 = DIRECTION ( 'NONE',  ( 0.9999697198139515519, 0.000000000000000000, 0.007781995580013368816 ) ) ;
#38847 = DIRECTION ( 'NONE',  ( 0.007781995580012662783, 0.000000000000000000, -0.9999697198139514409 ) ) ;
#38848 = CARTESIAN_POINT ( 'NONE',  ( -66.90530812237336988, -8.360358167099663618, 0.5932824550257441709 ) ) ;
#38849 = VERTEX_POINT ( 'NONE', #44299 ) ;
#38850 = LINE ( 'NONE', #47927, #38331 ) ;
#38851 = ORIENTED_EDGE ( 'NONE', *, *, #54287, .F. ) ;
#38852 = CARTESIAN_POINT ( 'NONE',  ( -17.03414339976229996, 4.495856970884009485, 10.87642811861771186 ) ) ;
#38853 = LINE ( 'NONE', #56165, #33241 ) ;
#38854 = DIRECTION ( 'NONE',  ( 0.000000000000000000, -0.000000000000000000, -1.000000000000000000 ) ) ;
#38855 = EDGE_CURVE ( 'NONE', #34418, #10029, #18444, .T. ) ;
#38856 = CARTESIAN_POINT ( 'NONE',  ( -20.08582687197957029, 2.067327705546507133, 8.076175355576905801 ) ) ;
#38857 = CARTESIAN_POINT ( 'NONE',  ( -14.49969738240122474, -0.1191753592594189115, 3.699573946482198394 ) ) ;
#38858 = DIRECTION ( 'NONE',  ( 0.6246952433987894571, -0.7422098413412800966, -0.2426528472758541777 ) ) ;
#38859 = DIRECTION ( 'NONE',  ( 0.7660212471507180654, -0.6427876096865404731, 0.005961354470445141482 ) ) ;
#38860 = APPLICATION_PROTOCOL_DEFINITION ( 'draft international standard', 'automotive_design', 1998, #12626 ) ;
#38861 = ORIENTED_EDGE ( 'NONE', *, *, #39966, .F. ) ;
#38862 = CARTESIAN_POINT ( 'NONE',  ( -25.57735469142784979, 16.15913242205765599, 4.626755875664946949 ) ) ;
#38863 = DIRECTION ( 'NONE',  ( -0.9999697198139514409, -0.000000000000000000, -0.007781995580013368816 ) ) ;
#38864 = CARTESIAN_POINT ( 'NONE',  ( -11.40636015113596180, 0.000000000000000000, 11.32142374880780089 ) ) ;
#38865 = EDGE_CURVE ( 'NONE', #43820, #5084, #39763, .T. ) ;
#38866 = CARTESIAN_POINT ( 'NONE',  ( -24.26908309836554878, 0.000000000000000000, 6.108867788427308376 ) ) ;
#38867 = DIRECTION ( 'NONE',  ( -0.005002170337468016433, -0.7660444431189770143, 0.6427681459581293666 ) ) ;
#38868 = EDGE_CURVE ( 'NONE', #36173, #44387, #31228, .T. ) ;
#38869 = DIRECTION ( 'NONE',  ( -0.5364919789714478471, 0.6444004775717705469, -0.5449076811759709926 ) ) ;
#38870 = EDGE_CURVE ( 'NONE', #17707, #25181, #13622, .T. ) ;
#38871 = CARTESIAN_POINT ( 'NONE',  ( -15.88579177843824830, -0.1166911823299096179, 2.952207434841243927 ) ) ;
#38872 = ORIENTED_EDGE ( 'NONE', *, *, #42479, .T. ) ;
#38873 = CARTESIAN_POINT ( 'NONE',  ( 0.2239497891030733101, -1.668917571073584627, -5.998622290806041590 ) ) ;
#38874 = CARTESIAN_POINT ( 'NONE',  ( -67.92407581255017135, -9.617479462011470304, -5.273316683197693422 ) ) ;
#38875 = ORIENTED_EDGE ( 'NONE', *, *, #17940, .T. ) ;
#38876 = ORIENTED_EDGE ( 'NONE', *, *, #26500, .F. ) ;
#38877 = FACE_OUTER_BOUND ( 'NONE', #4724, .T. ) ;
#38878 = EDGE_CURVE ( 'NONE', #19762, #20122, #22152, .T. ) ;
#38879 = VECTOR ( 'NONE', #12857, 1000.000000000000000 ) ;
#38880 = VERTEX_POINT ( 'NONE', #9365 ) ;
#38881 = ADVANCED_FACE ( 'NONE', ( #18161 ), #30110, .F. ) ;
#38882 = EDGE_CURVE ( 'NONE', #24617, #30957, #21861, .T. ) ;
#38883 = ORIENTED_EDGE ( 'NONE', *, *, #45821, .F. ) ;
#38884 = ORIENTED_EDGE ( 'NONE', *, *, #13399, .F. ) ;
#38885 = ORIENTED_EDGE ( 'NONE', *, *, #42096, .T. ) ;
#38886 = LINE ( 'NONE', #749, #13940 ) ;
#38887 = ORIENTED_EDGE ( 'NONE', *, *, #26772, .F. ) ;
#38888 = LINE ( 'NONE', #52226, #16919 ) ;
#38889 = LINE ( 'NONE', #26112, #3099 ) ;
#38890 = ADVANCED_FACE ( 'NONE', ( #842 ), #34951, .F. ) ;
#38891 = EDGE_CURVE ( 'NONE', #35565, #26804, #43711, .T. ) ;
#38892 = ORIENTED_EDGE ( 'NONE', *, *, #28065, .F. ) ;
#38893 = ORIENTED_EDGE ( 'NONE', *, *, #6602, .F. ) ;
#38894 = EDGE_CURVE ( 'NONE', #12052, #30300, #26988, .T. ) ;
#38895 = CARTESIAN_POINT ( 'NONE',  ( -66.57831216173161692, 3.903127820947815962E-15, -5.126440291711408470 ) ) ;
#38896 = ORIENTED_EDGE ( 'NONE', *, *, #16425, .F. ) ;
#38897 = DIRECTION ( 'NONE',  ( 0.000000000000000000, -1.000000000000000000, 0.000000000000000000 ) ) ;
#38898 = DIRECTION ( 'NONE',  ( -0.9999697198139514409, -0.000000000000000000, -0.007781995580013368816 ) ) ;
#38899 = ORIENTED_EDGE ( 'NONE', *, *, #1674, .F. ) ;
#38900 = LINE ( 'NONE', #47120, #42127 ) ;
#38901 = VERTEX_POINT ( 'NONE', #52531 ) ;
#38902 = DIRECTION ( 'NONE',  ( 0.7660212471507180654, -0.6427876096865404731, 0.005961354470445141482 ) ) ;
#38903 = DIRECTION ( 'NONE',  ( -0.8531650599175527594, 0.4028455766673922356, 0.3313982828793700652 ) ) ;
#38904 = ORIENTED_EDGE ( 'NONE', *, *, #23589, .T. ) ;
#38905 = DIRECTION ( 'NONE',  ( 0.000000000000000000, -1.000000000000000000, 0.000000000000000000 ) ) ;
#38906 = CARTESIAN_POINT ( 'NONE',  ( -7.148249425445639460, -2.280392264726430529, 8.590678399319719105 ) ) ;
#38907 = FACE_OUTER_BOUND ( 'NONE', #31282, .T. ) ;
#38908 = CARTESIAN_POINT ( 'NONE',  ( -18.67697421479882181, -0.1191753592594197858, 4.036397482078229793 ) ) ;
#38909 = ORIENTED_EDGE ( 'NONE', *, *, #18108, .T. ) ;
#38910 =( GEOMETRIC_REPRESENTATION_CONTEXT ( 3 ) GLOBAL_UNCERTAINTY_ASSIGNED_CONTEXT ( ( #51263 ) ) GLOBAL_UNIT_ASSIGNED_CONTEXT ( ( #26396, #33805, #17063 ) ) REPRESENTATION_CONTEXT ( 'NONE', 'WORKASPACE' ) );
#38911 = FACE_OUTER_BOUND ( 'NONE', #224, .T. ) ;
#38912 = LINE ( 'NONE', #48239, #628 ) ;
#38913 = CARTESIAN_POINT ( 'NONE',  ( -20.18792284424153038, 1.095915999411505082, 6.521580794694486372 ) ) ;
#38914 = DIRECTION ( 'NONE',  ( 0.000000000000000000, -1.000000000000000000, 0.000000000000000000 ) ) ;
#38915 = EDGE_CURVE ( 'NONE', #15160, #42447, #5399, .T. ) ;
#38916 = DIRECTION ( 'NONE',  ( 0.2426528472758541499, 0.7422098413412800966, 0.6246952433987894571 ) ) ;
#38917 = LINE ( 'NONE', #263, #43091 ) ;
#38918 = CARTESIAN_POINT ( 'NONE',  ( -17.28610440469613252, -0.1191753592594162470, 3.496136413696765644 ) ) ;
#38919 = CARTESIAN_POINT ( 'NONE',  ( -9.948355478519198769, 0.000000000000000000, 3.096332430070161124 ) ) ;
#38920 = LINE ( 'NONE', #51955, #48556 ) ;
#38921 = ORIENTED_EDGE ( 'NONE', *, *, #49337, .F. ) ;
#38922 = CARTESIAN_POINT ( 'NONE',  ( -13.58479385624546865, -0.1191753592594188005, 5.553354286307040866 ) ) ;
#38923 = ORIENTED_EDGE ( 'NONE', *, *, #5060, .T. ) ;
#38924 = DIRECTION ( 'NONE',  ( -0.6427681459581293666, -0.7660444431189770143, -0.005002170337467561935 ) ) ;
#38925 = DIRECTION ( 'NONE',  ( 0.005002170337468016433, -0.7660444431189770143, -0.6427681459581293666 ) ) ;
#38926 = EDGE_CURVE ( 'NONE', #33548, #19751, #25867, .T. ) ;
#38927 = CARTESIAN_POINT ( 'NONE',  ( -10.47421230394850866, 0.000000000000000000, 10.95934586908605723 ) ) ;
#38928 = ADVANCED_FACE ( 'NONE', ( #43452 ), #17317, .F. ) ;
#38929 = LINE ( 'NONE', #13083, #1549 ) ;
#38930 = ADVANCED_FACE ( 'NONE', ( #36329 ), #36079, .F. ) ;
#38931 = CARTESIAN_POINT ( 'NONE',  ( -26.13493519185646008, 0.000000000000000000, 7.033017491833586377 ) ) ;
#38932 = VERTEX_POINT ( 'NONE', #49925 ) ;
#38933 = ORIENTED_EDGE ( 'NONE', *, *, #52111, .T. ) ;
#38934 = DIRECTION ( 'NONE',  ( 0.007781995580012662783, 0.000000000000000000, -0.9999697198139514409 ) ) ;
#38935 = CARTESIAN_POINT ( 'NONE',  ( -28.92982233430281980, 0.000000000000000000, 7.919257187036034651 ) ) ;
#38936 = ORIENTED_EDGE ( 'NONE', *, *, #11863, .T. ) ;
#38937 = CARTESIAN_POINT ( 'NONE',  ( -17.36532418587302473, -0.1191753592594177458, 13.67570816655714516 ) ) ;
#38938 = ORIENTED_EDGE ( 'NONE', *, *, #50766, .T. ) ;
#38939 = ADVANCED_FACE ( 'NONE', ( #6790 ), #53638, .F. ) ;
#38940 = CARTESIAN_POINT ( 'NONE',  ( -12.00530485164738970, 0.000000000000000000, 7.881641681912517683 ) ) ;
#38941 = ORIENTED_EDGE ( 'NONE', *, *, #16428, .F. ) ;
#38942 = DIRECTION ( 'NONE',  ( 0.007781995580012663651, 0.000000000000000000, -0.9999697198139515519 ) ) ;
#38943 = EDGE_CURVE ( 'NONE', #4182, #36112, #14744, .T. ) ;
#38944 = VERTEX_POINT ( 'NONE', #53381 ) ;
#38945 = EDGE_LOOP ( 'NONE', ( #16595, #11054, #18255, #5792 ) ) ;
#38946 = ORIENTED_EDGE ( 'NONE', *, *, #43705, .T. ) ;
#38947 = DIRECTION ( 'NONE',  ( 0.007781995580012662783, 0.000000000000000000, -0.9999697198139514409 ) ) ;
#38948 = CARTESIAN_POINT ( 'NONE',  ( -9.027703845352876399, 0.000000000000000000, 4.211493363379472221 ) ) ;
#38949 = DIRECTION ( 'NONE',  ( -0.005002170337468016433, -0.7660444431189770143, 0.6427681459581293666 ) ) ;
#38950 = EDGE_CURVE ( 'NONE', #19740, #2, #28350, .T. ) ;
#38951 = DIRECTION ( 'NONE',  ( 0.005002170337468016433, -0.7660444431189770143, -0.6427681459581293666 ) ) ;
#38952 = ORIENTED_EDGE ( 'NONE', *, *, #49754, .F. ) ;
#38953 = ORIENTED_EDGE ( 'NONE', *, *, #35167, .T. ) ;
#38954 = EDGE_CURVE ( 'NONE', #32592, #31186, #14479, .T. ) ;
#38955 = ORIENTED_EDGE ( 'NONE', *, *, #47442, .T. ) ;
#38956 = CARTESIAN_POINT ( 'NONE',  ( -14.88523388135589443, 0.000000000000000000, 6.381901129057940381 ) ) ;
#38957 = ORIENTED_EDGE ( 'NONE', *, *, #12853, .T. ) ;
#38958 = DIRECTION ( 'NONE',  ( -0.5364919789714478471, 0.6444004775717705469, -0.5449076811759709926 ) ) ;
#38959 = ORIENTED_EDGE ( 'NONE', *, *, #51560, .T. ) ;
#38960 = CARTESIAN_POINT ( 'NONE',  ( -69.11683642851026832, -9.015837829197110409, 7.493101075386320531 ) ) ;
#38961 = DIRECTION ( 'NONE',  ( 0.5364919789714477361, 0.6444004775717706579, 0.5449076811759711036 ) ) ;
#38962 = ORIENTED_EDGE ( 'NONE', *, *, #52269, .T. ) ;
#38963 = CARTESIAN_POINT ( 'NONE',  ( -17.74560456716937296, 0.000000000000000000, 3.774316574337878372 ) ) ;
#38964 = ORIENTED_EDGE ( 'NONE', *, *, #6294, .T. ) ;
#38965 = DIRECTION ( 'NONE',  ( 0.007781995580012663651, -3.146120232559066537E-19, -0.9999697198139514409 ) ) ;
#38966 = ORIENTED_EDGE ( 'NONE', *, *, #44815, .T. ) ;
#38967 = FACE_OUTER_BOUND ( 'NONE', #20229, .T. ) ;
#38968 = LINE ( 'NONE', #12840, #35721 ) ;
#38969 = DIRECTION ( 'NONE',  ( 0.007781995580012663651, -3.146120232559066537E-19, -0.9999697198139514409 ) ) ;
#38970 = ORIENTED_EDGE ( 'NONE', *, *, #4952, .F. ) ;
#38971 = DIRECTION ( 'NONE',  ( 0.5449076811759707706, 0.6444004775717708799, -0.5364919789714476250 ) ) ;
#38972 = CARTESIAN_POINT ( 'NONE',  ( -15.60102546347950536, 0.000000000000000000, 12.95077420755565356 ) ) ;
#38973 = LINE ( 'NONE', #334, #12218 ) ;
#38974 = EDGE_CURVE ( 'NONE', #2376, #36986, #32077, .T. ) ;
#38975 = CARTESIAN_POINT ( 'NONE',  ( -11.98370190339197272, -1.003701604285656579, 2.984053846613921035 ) ) ;
#38976 = LINE ( 'NONE', #43, #47588 ) ;
#38977 = DIRECTION ( 'NONE',  ( 0.007781995580012663651, 0.000000000000000000, -0.9999697198139515519 ) ) ;
#38978 = EDGE_CURVE ( 'NONE', #5370, #1847, #44850, .T. ) ;
#38979 = CARTESIAN_POINT ( 'NONE',  ( -16.89925026227929195, -0.1191753592594197858, 13.49466922669627422 ) ) ;
#38980 = ORIENTED_EDGE ( 'NONE', *, *, #17428, .T. ) ;
#38981 = DIRECTION ( 'NONE',  ( 0.6427681459581294776, -0.7660444431189769032, 0.005002170337467562802 ) ) ;
#38982 = ADVANCED_FACE ( 'NONE', ( #32376 ), #24113, .F. ) ;
#38983 = LINE ( 'NONE', #29907, #40430 ) ;
#38984 = CARTESIAN_POINT ( 'NONE',  ( -20.98837076068963370, 5.305366725996512045, 13.74092773148062285 ) ) ;
#38985 = ORIENTED_EDGE ( 'NONE', *, *, #50497, .T. ) ;
#38986 = LINE ( 'NONE', #30484, #4828 ) ;
#38987 = DIRECTION ( 'NONE',  ( -0.6427681459581293666, -0.7660444431189770143, -0.005002170337467561935 ) ) ;
#38988 = ORIENTED_EDGE ( 'NONE', *, *, #41373, .T. ) ;
#38989 = ADVANCED_FACE ( 'NONE', ( #10204 ), #19573, .F. ) ;
#38990 = EDGE_CURVE ( 'NONE', #10403, #53934, #24420, .T. ) ;
#38991 = EDGE_CURVE ( 'NONE', #45002, #37252, #45674, .T. ) ;
#38992 = CARTESIAN_POINT ( 'NONE',  ( -27.06552663992790997, 0.000000000000000000, 7.195101427592543786 ) ) ;
#38993 = PLANE ( 'NONE',  #20298 ) ;
#38994 = DIRECTION ( 'NONE',  ( -0.6427681459581293666, -0.7660444431189770143, -0.005002170337467561935 ) ) ;
#38995 = CARTESIAN_POINT ( 'NONE',  ( -66.76709096105220453, 1.999999999999983569, -6.184885810276858464 ) ) ;
#38996 = ORIENTED_EDGE ( 'NONE', *, *, #5627, .F. ) ;
#38997 = ORIENTED_EDGE ( 'NONE', *, *, #23296, .T. ) ;
#38998 = DIRECTION ( 'NONE',  ( 0.5449076811759707706, 0.6444004775717708799, -0.5364919789714476250 ) ) ;
#38999 = CARTESIAN_POINT ( 'NONE',  ( -19.60990026154428278, 0.000000000000000000, 4.498472333781370125 ) ) ;
#39000 = DIRECTION ( 'NONE',  ( -0.5449076811759708816, 0.6444004775717707689, 0.5364919789714475140 ) ) ;
#39001 = CARTESIAN_POINT ( 'NONE',  ( 2.072287782118878319, 0.000000000000000000, -2.950529333540147015 ) ) ;
#39002 = CARTESIAN_POINT ( 'NONE',  ( -18.86354292863559579, 0.000000000000000000, 14.21804678658176080 ) ) ;
#39003 = EDGE_CURVE ( 'NONE', #55548, #17566, #48844, .T. ) ;
#39004 = CARTESIAN_POINT ( 'NONE',  ( -22.40478740399063895, 0.000000000000000000, 5.384712028983816623 ) ) ;
#39005 = ORIENTED_EDGE ( 'NONE', *, *, #6377, .F. ) ;
#39006 = PLANE ( 'NONE',  #214 ) ;
#39007 = ADVANCED_FACE ( 'NONE', ( #1685 ), #19010, .F. ) ;
#39008 = CARTESIAN_POINT ( 'NONE',  ( -13.02668629399155265, 0.000000000000000000, 6.396364776129978225 ) ) ;
#39009 = VERTEX_POINT ( 'NONE', #18753 ) ;
#39010 = ADVANCED_FACE ( 'NONE', ( #5665 ), #27835, .F. ) ;
#39011 = PLANE ( 'NONE',  #49252 ) ;
#39012 = FACE_OUTER_BOUND ( 'NONE', #24984, .T. ) ;
#39013 = CARTESIAN_POINT ( 'NONE',  ( -27.06708303904391144, 0.000000000000000000, 7.395095371555332697 ) ) ;
#39014 = VERTEX_POINT ( 'NONE', #19273 ) ;
#39015 = EDGE_CURVE ( 'NONE', #20518, #6678, #23814, .T. ) ;
#39016 = CARTESIAN_POINT ( 'NONE',  ( -11.95764949545960754, -3.756034771668162797, 1.406241090487040157 ) ) ;
#39017 = VERTEX_POINT ( 'NONE', #39057 ) ;
#39018 = VECTOR ( 'NONE', #26923, 1000.000000000000000 ) ;
#39019 = ORIENTED_EDGE ( 'NONE', *, *, #23025, .F. ) ;
#39020 = ORIENTED_EDGE ( 'NONE', *, *, #40358, .T. ) ;
#39021 = VERTEX_POINT ( 'NONE', #42275 ) ;
#39022 = PLANE ( 'NONE',  #41158 ) ;
#39023 = VERTEX_POINT ( 'NONE', #29193 ) ;
#39024 = CARTESIAN_POINT ( 'NONE',  ( -13.23914656339586315, 23.28260020609454983, -3.687136209236635764 ) ) ;
#39025 = ORIENTED_EDGE ( 'NONE', *, *, #52139, .T. ) ;
#39026 = DIRECTION ( 'NONE',  ( 0.007781995580012662783, 0.000000000000000000, -0.9999697198139514409 ) ) ;
#39027 = ORIENTED_EDGE ( 'NONE', *, *, #8618, .T. ) ;
#39028 = CARTESIAN_POINT ( 'NONE',  ( -18.19747506107908563, 0.000000000000000000, 14.03856424583689311 ) ) ;
#39029 = VERTEX_POINT ( 'NONE', #42549 ) ;
#39030 = CARTESIAN_POINT ( 'NONE',  ( -9.498088849204524564, 0.000000000000000000, 4.946496858126993246 ) ) ;
#39031 = LINE ( 'NONE', #51543, #18695 ) ;
#39032 = CARTESIAN_POINT ( 'NONE',  ( -17.51501930259471962, 2.876837460659008805, 8.406129810387598766 ) ) ;
#39033 = LINE ( 'NONE', #34772, #27824 ) ;
#39034 = LINE ( 'NONE', #13744, #29225 ) ;
#39035 = EDGE_LOOP ( 'NONE', ( #54906, #31119, #51654 ) ) ;
#39036 = ORIENTED_EDGE ( 'NONE', *, *, #44338, .F. ) ;
#39037 = CARTESIAN_POINT ( 'NONE',  ( -9.935275981939433620, 0.000000000000000000, 1.415645208431519642 ) ) ;
#39038 = CARTESIAN_POINT ( 'NONE',  ( -14.82598494076193596, -0.5179957512181571078, 2.623710384272013751 ) ) ;
#39039 = EDGE_CURVE ( 'NONE', #50224, #48862, #20697, .T. ) ;
#39040 = LINE ( 'NONE', #50959, #26083 ) ;
#39041 = LINE ( 'NONE', #30552, #13126 ) ;
#39042 = DIRECTION ( 'NONE',  ( -0.7660212471507179544, -0.6427876096865405842, -0.005961354470445141482 ) ) ;
#39043 = CARTESIAN_POINT ( 'NONE',  ( -12.76910910251310227, 0.000000000000000000, 7.306359454592487701 ) ) ;
#39044 = EDGE_LOOP ( 'NONE', ( #13540, #45826, #49275, #47446 ) ) ;
#39045 = DIRECTION ( 'NONE',  ( 0.9999697198139515519, 0.000000000000000000, 0.007781995580013368816 ) ) ;
#39046 = LINE ( 'NONE', #4974, #16805 ) ;
#39047 = ORIENTED_EDGE ( 'NONE', *, *, #12987, .F. ) ;
#39048 = ADVANCED_FACE ( 'NONE', ( #26276 ), #37428, .F. ) ;
#39049 = EDGE_CURVE ( 'NONE', #48365, #7041, #41963, .T. ) ;
#39050 = EDGE_CURVE ( 'NONE', #37328, #34091, #127, .T. ) ;
#39051 = FACE_OUTER_BOUND ( 'NONE', #34929, .T. ) ;
#39052 = FACE_OUTER_BOUND ( 'NONE', #31921, .T. ) ;
#39053 = DIRECTION ( 'NONE',  ( 0.000000000000000000, 0.000000000000000000, 1.000000000000000000 ) ) ;
#39054 = ADVANCED_FACE ( 'NONE', ( #46226 ), #13232, .F. ) ;
#39055 = DIRECTION ( 'NONE',  ( 0.000000000000000000, -1.000000000000000000, 0.000000000000000000 ) ) ;
#39056 = VECTOR ( 'NONE', #41217, 1000.000000000000227 ) ;
#39057 = CARTESIAN_POINT ( 'NONE',  ( -19.16043661833849754, -0.1191753592594170102, 5.509963345090925557 ) ) ;
#39058 = ORIENTED_EDGE ( 'NONE', *, *, #46253, .F. ) ;
#39059 = ORIENTED_EDGE ( 'NONE', *, *, #34897, .F. ) ;
#39060 = LINE ( 'NONE', #42742, #38464 ) ;
#39061 = CARTESIAN_POINT ( 'NONE',  ( -14.56543180263941828, 4.333955019861509328, 9.651788012545988948 ) ) ;
#39062 = DIRECTION ( 'NONE',  ( 0.7660212471507180654, -0.6427876096865404731, 0.005961354470445141482 ) ) ;
#39063 = B_SPLINE_CURVE_WITH_KNOTS ( 'NONE', 3,
 ( #3675, #20446, #37785, #11908 ),
 .UNSPECIFIED., .F., .F.,
 ( 4, 4 ),
 ( 5.447042101129314832E-05, 0.0005066785541756341910 ),
 .UNSPECIFIED. ) ;
#39064 = CARTESIAN_POINT ( 'NONE',  ( -28.93060053386082231, -0.1191753592594197858, 8.019254159017428663 ) ) ;
#39065 = LINE ( 'NONE', #44437, #16703 ) ;
#39066 = PLANE ( 'NONE',  #29173 ) ;
#39067 = DIRECTION ( 'NONE',  ( 0.005961354470445682716, -0.6427876096865404731, -0.7660212471507180654 ) ) ;
#39069 = ADVANCED_FACE ( 'NONE', ( #33205 ), #15858, .F. ) ;
#39068 = ORIENTED_EDGE ( 'NONE', *, *, #37054, .F. ) ;
#39070 = LINE ( 'NONE', #21756, #50445 ) ;
#39071 = LINE ( 'NONE', #144, #47790 ) ;
#39072 = ADVANCED_FACE ( 'NONE', ( #3377 ), #11324, .F. ) ;
#39073 = ORIENTED_EDGE ( 'NONE', *, *, #44258, .F. ) ;
#39074 = LINE ( 'NONE', #21494, #9280 ) ;
#39075 = ORIENTED_EDGE ( 'NONE', *, *, #49948, .T. ) ;
#39076 = CARTESIAN_POINT ( 'NONE',  ( -12.13851405436063047, 0.000000000000000000, 11.68505802764555135 ) ) ;
#39077 = ORIENTED_EDGE ( 'NONE', *, *, #4196, .F. ) ;
#39078 = EDGE_CURVE ( 'NONE', #1003, #441, #47872, .T. ) ;
#39079 = VECTOR ( 'NONE', #23579, 1000.000000000000114 ) ;
#39080 = ORIENTED_EDGE ( 'NONE', *, *, #34192, .F. ) ;
#39081 = EDGE_CURVE ( 'NONE', #54767, #36041, #43585, .T. ) ;
#39082 = EDGE_LOOP ( 'NONE', ( #4460, #39676, #49892 ) ) ;
#39083 = ORIENTED_EDGE ( 'NONE', *, *, #30236, .T. ) ;
#39084 = ORIENTED_EDGE ( 'NONE', *, *, #43124, .T. ) ;
#39085 = ORIENTED_EDGE ( 'NONE', *, *, #18074, .T. ) ;
#39086 = CARTESIAN_POINT ( 'NONE',  ( -9.110551994824897193, 0.000000000000000000, 3.538847790438064411 ) ) ;
#39087 = DIRECTION ( 'NONE',  ( 0.000000000000000000, -0.000000000000000000, -1.000000000000000000 ) ) ;
#39088 = CARTESIAN_POINT ( 'NONE',  ( -14.00280974873554030, 0.000000000000000000, 12.40921378708904044 ) ) ;
#39089 = VECTOR ( 'NONE', #17045, 1000.000000000000000 ) ;
#39090 = ORIENTED_EDGE ( 'NONE', *, *, #19652, .T. ) ;
#39091 = CARTESIAN_POINT ( 'NONE',  ( -16.58287145540726826, 2.876837460659006585, 8.044051930665851557 ) ) ;
#39092 = ORIENTED_EDGE ( 'NONE', *, *, #5926, .T. ) ;
#39093 = VERTEX_POINT ( 'NONE', #15564 ) ;
#39094 = VECTOR ( 'NONE', #16152, 1000.000000000000227 ) ;
#39095 = LINE ( 'NONE', #30305, #41952 ) ;
#39096 = DIRECTION ( 'NONE',  ( 0.000000000000000000, -0.000000000000000000, -1.000000000000000000 ) ) ;
#39097 = DIRECTION ( 'NONE',  ( -0.5364919789714478471, 0.6444004775717705469, -0.5449076811759709926 ) ) ;
#39098 = ORIENTED_EDGE ( 'NONE', *, *, #37522, .F. ) ;
#39099 = DIRECTION ( 'NONE',  ( 0.5449076811759707706, 0.6444004775717708799, -0.5364919789714476250 ) ) ;
#39100 = ORIENTED_EDGE ( 'NONE', *, *, #8094, .F. ) ;
#39101 = CARTESIAN_POINT ( 'NONE',  ( -17.40972996391339578, 0.000000000000000000, 6.531580930396862605 ) ) ;
#39102 = DIRECTION ( 'NONE',  ( -0.005002170337468016433, -0.7660444431189770143, 0.6427681459581293666 ) ) ;
#39103 = CARTESIAN_POINT ( 'NONE',  ( -12.80458192191714595, 0.000000000000000000, 11.86454056839041726 ) ) ;
#39104 = DIRECTION ( 'NONE',  ( 0.000000000000000000, -1.000000000000000000, 0.000000000000000000 ) ) ;
#39105 = CARTESIAN_POINT ( 'NONE',  ( 4.848100717410752658, 0.000000000000000000, 2.029539223447463847 ) ) ;
#39106 = CARTESIAN_POINT ( 'NONE',  ( -10.94028622754223967, 0.000000000000000000, 11.14038480894692995 ) ) ;
#39107 = LINE ( 'NONE', #5329, #45691 ) ;
#39108 = FACE_OUTER_BOUND ( 'NONE', #21272, .T. ) ;
#39109 = ORIENTED_EDGE ( 'NONE', *, *, #8841, .T. ) ;
#39110 = CARTESIAN_POINT ( 'NONE',  ( -55.47117325737978888, 6.581829179614757663, -1.080525476705088916 ) ) ;
#39111 = EDGE_CURVE ( 'NONE', #32474, #41831, #2774, .T. ) ;
#39112 = VECTOR ( 'NONE', #30345, 1000.000000000000000 ) ;
#39113 = VECTOR ( 'NONE', #53361, 999.9999999999998863 ) ;
#39114 = DIRECTION ( 'NONE',  ( 0.9999697198139515519, 0.000000000000000000, 0.007781995580013368816 ) ) ;
#39115 = DIRECTION ( 'NONE',  ( 0.6427681459581294776, -0.7660444431189769032, 0.005002170337467562802 ) ) ;
#39116 = LINE ( 'NONE', #52725, #14533 ) ;
#39117 = CARTESIAN_POINT ( 'NONE',  ( -33.30197399026911853, 11.69932139048425235, -4.869895353451894060 ) ) ;
#39118 = LINE ( 'NONE', #42545, #1412 ) ;
#39119 = EDGE_CURVE ( 'NONE', #48024, #48202, #12160, .T. ) ;
#39120 = EDGE_CURVE ( 'NONE', #27927, #46187, #45975, .T. ) ;
#39121 = LINE ( 'NONE', #21544, #23208 ) ;
#39122 = CARTESIAN_POINT ( 'NONE',  ( -17.74482636761137044, -0.1191753592594197858, 3.674319602356483916 ) ) ;
#39123 = CONTEXT_DEPENDENT_SHAPE_REPRESENTATION ( #8656, #52720 ) ;
#39124 = ORIENTED_EDGE ( 'NONE', *, *, #47523, .F. ) ;
#39125 = DIRECTION ( 'NONE',  ( 0.005961354470445682716, -0.6427876096865404731, -0.7660212471507180654 ) ) ;
#39126 = DIRECTION ( 'NONE',  ( 0.000000000000000000, -0.000000000000000000, -1.000000000000000000 ) ) ;
#39127 = LINE ( 'NONE', #39712, #37253 ) ;
#39128 = FACE_OUTER_BOUND ( 'NONE', #42424, .T. ) ;
#39129 = DIRECTION ( 'NONE',  ( 0.9999697198139515519, 0.000000000000000000, 0.007781995580013368816 ) ) ;
#39130 = DIRECTION ( 'NONE',  ( 0.005961354470445682716, -0.6427876096865404731, -0.7660212471507180654 ) ) ;
#39131 = CARTESIAN_POINT ( 'NONE',  ( -15.52718360830426292, 1.095915999411505082, 4.711191396085759209 ) ) ;
#39132 = VECTOR ( 'NONE', #49715, 1000.000000000000227 ) ;
#39133 = FACE_OUTER_BOUND ( 'NONE', #1838, .T. ) ;
#39134 = CARTESIAN_POINT ( 'NONE',  ( -12.50510409456438587, 0.2864062442990034651, 2.208769662944593648 ) ) ;
#39135 = EDGE_LOOP ( 'NONE', ( #4984, #41405, #38010, #18211 ) ) ;
#39136 = CARTESIAN_POINT ( 'NONE',  ( -16.45746374218896335, 0.000000000000000000, 3.584335127870767135 ) ) ;
#39137 = ORIENTED_EDGE ( 'NONE', *, *, #22411, .F. ) ;
#39138 = EDGE_CURVE ( 'NONE', #19873, #38484, #46815, .T. ) ;
#39139 = ORIENTED_EDGE ( 'NONE', *, *, #39675, .F. ) ;
#39140 = ORIENTED_EDGE ( 'NONE', *, *, #53870, .T. ) ;
#39141 = ORIENTED_EDGE ( 'NONE', *, *, #31740, .F. ) ;
#39142 = ADVANCED_FACE ( 'NONE', ( #3069 ), #7085, .F. ) ;
#39143 = ORIENTED_EDGE ( 'NONE', *, *, #53519, .T. ) ;
#39144 = DIRECTION ( 'NONE',  ( -0.5364919789714478471, 0.6444004775717705469, -0.5449076811759709926 ) ) ;
#39145 = DIRECTION ( 'NONE',  ( -0.6427681459581293666, -0.7660444431189770143, -0.005002170337467561935 ) ) ;
#39146 = VECTOR ( 'NONE', #19790, 1000.000000000000227 ) ;
#39147 = AXIS2_PLACEMENT_3D ( 'NONE', #37, #17957, #328 ) ;
#39148 = ORIENTED_EDGE ( 'NONE', *, *, #2937, .F. ) ;
#39149 = EDGE_LOOP ( 'NONE', ( #51599, #23179, #19130, #539, #46612 ) ) ;
#39150 = EDGE_CURVE ( 'NONE', #45990, #15181, #7931, .T. ) ;
#39151 = VECTOR ( 'NONE', #42099, 999.9999999999998863 ) ;
#39152 = CARTESIAN_POINT ( 'NONE',  ( -27.06552663992790997, 0.000000000000000000, 7.195101427592543786 ) ) ;
#39153 = EDGE_LOOP ( 'NONE', ( #55694, #7519, #32591, #20933 ) ) ;
#39154 = DIRECTION ( 'NONE',  ( 0.6246952433987894571, -0.7422098413412800966, -0.2426528472758541777 ) ) ;
#39155 = CARTESIAN_POINT ( 'NONE',  ( 5.221828392167460642, 0.000000000000000000, -2.393421119419572918 ) ) ;
#39156 = ORIENTED_EDGE ( 'NONE', *, *, #627, .F. ) ;
#39157 = DIRECTION ( 'NONE',  ( 0.000000000000000000, -1.000000000000000000, 0.000000000000000000 ) ) ;
#39158 = ORIENTED_EDGE ( 'NONE', *, *, #3280, .F. ) ;
#39159 = PLANE ( 'NONE',  #52722 ) ;
#39160 = AXIS2_PLACEMENT_3D ( 'NONE', #15288, #11294, #1915 ) ;
#39161 = AXIS2_PLACEMENT_3D ( 'NONE', #42648, #16832, #38703 ) ;
#39162 = DIRECTION ( 'NONE',  ( 0.5364919789714477361, 0.6444004775717706579, 0.5449076811759711036 ) ) ;
#39163 = ORIENTED_EDGE ( 'NONE', *, *, #4275, .T. ) ;
#39164 = FACE_OUTER_BOUND ( 'NONE', #5314, .T. ) ;
#39165 = CARTESIAN_POINT ( 'NONE',  ( -17.26532721389163072, 0.000000000000000000, 13.67648636611514590 ) ) ;
#39166 = LINE ( 'NONE', #25006, #34826 ) ;
#39167 = EDGE_LOOP ( 'NONE', ( #38193, #27578, #38671 ) ) ;
#39168 = DIRECTION ( 'NONE',  ( 0.9321478471874541372, 0.000000000000000000, -0.3620778797217453771 ) ) ;
#39169 = EDGE_CURVE ( 'NONE', #53748, #22074, #55063, .T. ) ;
#39170 = VERTEX_POINT ( 'NONE', #41689 ) ;
#39171 = DIRECTION ( 'NONE',  ( 0.7660212471507180654, -0.6427876096865404731, 0.005961354470445141482 ) ) ;
#39172 = LINE ( 'NONE', #52255, #14230 ) ;
#39173 = CARTESIAN_POINT ( 'NONE',  ( -20.54126990917373519, -0.1191753592594197858, 4.760553241521720658 ) ) ;
#39174 = DIRECTION ( 'NONE',  ( -0.5449076811759708816, 0.6444004775717707689, 0.5364919789714475140 ) ) ;
#39175 = CARTESIAN_POINT ( 'NONE',  ( 0.3240706152708103804, -3.670543518250629855, 2.124999999999998668 ) ) ;
#39176 = CARTESIAN_POINT ( 'NONE',  ( -20.54049170961573267, 0.000000000000000000, 4.660556269540326646 ) ) ;
#39177 = ADVANCED_FACE ( 'NONE', ( #52952 ), #45016, .F. ) ;
#39178 = CARTESIAN_POINT ( 'NONE',  ( 1.086233639165236964, 0.000000000000000000, 2.796443541562362078 ) ) ;
#39179 = FACE_OUTER_BOUND ( 'NONE', #52487, .T. ) ;
#39180 = DIRECTION ( 'NONE',  ( 0.007781995580012662783, 0.000000000000000000, -0.9999697198139514409 ) ) ;
#39181 = VERTEX_POINT ( 'NONE', #427 ) ;
#39182 = PLANE ( 'NONE',  #1161 ) ;
#39183 = DIRECTION ( 'NONE',  ( 0.9999697198139515519, 0.000000000000000000, 0.007781995580013368816 ) ) ;
#39184 = FACE_OUTER_BOUND ( 'NONE', #29082, .T. ) ;
#39185 = AXIS2_PLACEMENT_3D ( 'NONE', #38290, #55615, #34054 ) ;
#39186 = VECTOR ( 'NONE', #44541, 1000.000000000000000 ) ;
#39187 = DIRECTION ( 'NONE',  ( 0.007781995580012663651, -3.146120232559066537E-19, -0.9999697198139514409 ) ) ;
#39188 = CARTESIAN_POINT ( 'NONE',  ( -10.37421533196711465, -0.1191753592594197858, 10.96012406864405975 ) ) ;
#39189 = FACE_OUTER_BOUND ( 'NONE', #25463, .T. ) ;
#39190 = ADVANCED_FACE ( 'NONE', ( #26548 ), #52409, .F. ) ;
#39191 = ORIENTED_EDGE ( 'NONE', *, *, #21089, .T. ) ;
#39192 = VECTOR ( 'NONE', #15805, 999.9999999999998863 ) ;
#39193 = VECTOR ( 'NONE', #19632, 999.9999999999998863 ) ;
#39194 = EDGE_LOOP ( 'NONE', ( #31854, #41938, #23041 ) ) ;
#39195 = CARTESIAN_POINT ( 'NONE',  ( -17.93139508144814442, 0.000000000000000000, 13.85596890686001537 ) ) ;
#39196 = CARTESIAN_POINT ( 'NONE',  ( -25.85160216376510434, 17.67350346510513148, -4.606045122360801436 ) ) ;
#39197 = ORIENTED_EDGE ( 'NONE', *, *, #38950, .T. ) ;
#39198 = CARTESIAN_POINT ( 'NONE',  ( -20.94928162563153862, -3.917936722690662954, 4.893730847070894896 ) ) ;
#39199 = ORIENTED_EDGE ( 'NONE', *, *, #19657, .T. ) ;
#39200 = CARTESIAN_POINT ( 'NONE',  ( -17.26532721389163072, 0.000000000000000000, 13.67648636611514590 ) ) ;
#39201 = VECTOR ( 'NONE', #36002, 1000.000000000000227 ) ;
#39202 = VERTEX_POINT ( 'NONE', #1261 ) ;
#39203 = CARTESIAN_POINT ( 'NONE',  ( -13.79694961163590072, -1.489407457353155717, 4.485506886498618506 ) ) ;
#39204 = ORIENTED_EDGE ( 'NONE', *, *, #21987, .F. ) ;
#39205 = ORIENTED_EDGE ( 'NONE', *, *, #44909, .F. ) ;
#39206 = ORIENTED_EDGE ( 'NONE', *, *, #40320, .T. ) ;
#39207 = CARTESIAN_POINT ( 'NONE',  ( -15.40103151951671734, 0.000000000000000000, 12.95233060667165681 ) ) ;
#39208 = FACE_OUTER_BOUND ( 'NONE', #7543, .T. ) ;
#39209 = DIRECTION ( 'NONE',  ( -0.005002170337468016433, -0.7660444431189770143, 0.6427681459581293666 ) ) ;
#39210 = LINE ( 'NONE', #13653, #14901 ) ;
#39211 = ORIENTED_EDGE ( 'NONE', *, *, #8469, .F. ) ;
#39212 = EDGE_CURVE ( 'NONE', #42908, #40238, #13507, .T. ) ;
#39213 = EDGE_LOOP ( 'NONE', ( #38672, #27687, #4380, #29730 ) ) ;
#39214 = VECTOR ( 'NONE', #11747, 999.9999999999998863 ) ;
#39215 = ORIENTED_EDGE ( 'NONE', *, *, #4327, .F. ) ;
#39216 = DIRECTION ( 'NONE',  ( 0.9999697198139515519, 0.000000000000000000, 0.007781995580013368816 ) ) ;
#39217 = VERTEX_POINT ( 'NONE', #14065 ) ;
#39218 = VECTOR ( 'NONE', #54544, 999.9999999999998863 ) ;
#39219 = DIRECTION ( 'NONE',  ( 0.5449076811759707706, 0.6444004775717708799, -0.5364919789714476250 ) ) ;
#39220 = EDGE_LOOP ( 'NONE', ( #43006, #15344, #31257, #13826 ) ) ;
#39221 = LINE ( 'NONE', #18485, #46882 ) ;
#39222 = DIRECTION ( 'NONE',  ( 0.005002170337468016433, -0.7660444431189770143, -0.6427681459581293666 ) ) ;
#39223 = EDGE_CURVE ( 'NONE', #56039, #35922, #39643, .T. ) ;
#39224 = AXIS2_PLACEMENT_3D ( 'NONE', #28301, #54413, #28042 ) ;
#39225 = VECTOR ( 'NONE', #9025, 999.9999999999998863 ) ;
#39226 = ORIENTED_EDGE ( 'NONE', *, *, #38990, .T. ) ;
#39227 = DIRECTION ( 'NONE',  ( 0.9999697198139515519, 0.000000000000000000, 0.007781995580013368816 ) ) ;
#39228 = EDGE_LOOP ( 'NONE', ( #45949, #24182, #11274, #34789 ) ) ;
#39229 = ADVANCED_FACE ( 'NONE', ( #18041 ), #36210, .F. ) ;
#39230 = ADVANCED_FACE ( 'NONE', ( #27686 ), #35950, .F. ) ;
#39231 = AXIS2_PLACEMENT_3D ( 'NONE', #39285, #372, #4929 ) ;
#39232 = DIRECTION ( 'NONE',  ( 0.007781995580012663651, -3.146120232559066537E-19, -0.9999697198139514409 ) ) ;
#39233 = VECTOR ( 'NONE', #48181, 1000.000000000000227 ) ;
#39234 = ORIENTED_EDGE ( 'NONE', *, *, #6549, .T. ) ;
#39235 = CARTESIAN_POINT ( 'NONE',  ( -19.27845611090958755, 0.000000000000000000, 7.825040337060908513 ) ) ;
#39236 = LINE ( 'NONE', #56022, #46551 ) ;
#39237 = DIRECTION ( 'NONE',  ( 0.005002170337468016433, -0.7660444431189770143, -0.6427681459581293666 ) ) ;
#39238 = EDGE_CURVE ( 'NONE', #39979, #29674, #31398, .T. ) ;
#39239 = ORIENTED_EDGE ( 'NONE', *, *, #44544, .T. ) ;
#39240 = PLANE ( 'NONE',  #32902 ) ;
#39241 = EDGE_CURVE ( 'NONE', #42246, #39979, #5276, .T. ) ;
#39242 = PLANE ( 'NONE',  #30080 ) ;
#39243 = CARTESIAN_POINT ( 'NONE',  ( -20.97491883346917163, 4.819660872929012463, 4.675530102110849739 ) ) ;
#39244 = AXIS2_PLACEMENT_3D ( 'NONE', #39165, #25843, #21000 ) ;
#39245 = PLANE ( 'NONE',  #5027 ) ;
#39246 = VECTOR ( 'NONE', #19675, 1000.000000000000000 ) ;
#39247 = CARTESIAN_POINT ( 'NONE',  ( -9.342070512798265725, 0.000000000000000000, 10.59882438848031505 ) ) ;
#39248 = B_SPLINE_CURVE_WITH_KNOTS ( 'NONE', 1,
 ( #34210, #4087 ),
 .UNSPECIFIED., .F., .F.,
 ( 2, 2 ),
 ( 0.001874228446202061112, 0.003011459512596941206 ),
 .UNSPECIFIED. ) ;
#39249 = EDGE_CURVE ( 'NONE', #27552, #1558, #14613, .T. ) ;
#39250 = PLANE ( 'NONE',  #7058 ) ;
#39251 = DIRECTION ( 'NONE',  ( 0.7660212471507180654, -0.6427876096865404731, 0.005961354470445141482 ) ) ;
#39252 = ORIENTED_EDGE ( 'NONE', *, *, #36388, .T. ) ;
#39253 = PLANE ( 'NONE',  #35271 ) ;
#39254 = CARTESIAN_POINT ( 'NONE',  ( -25.97317167826694728, 17.60920382705421261, -4.611144759605506849 ) ) ;
#39255 = LINE ( 'NONE', #26464, #54998 ) ;
#39256 = ORIENTED_EDGE ( 'NONE', *, *, #42966, .T. ) ;
#39257 = DIRECTION ( 'NONE',  ( 0.5449076811759707706, 0.6444004775717708799, -0.5364919789714476250 ) ) ;
#39258 = DIRECTION ( 'NONE',  ( 0.9999697198139515519, 0.000000000000000000, 0.007781995580013368816 ) ) ;
#39259 = ORIENTED_EDGE ( 'NONE', *, *, #13845, .T. ) ;
#39260 = VECTOR ( 'NONE', #21776, 1000.000000000000227 ) ;
#39261 = EDGE_CURVE ( 'NONE', #30915, #22464, #30821, .T. ) ;
#39262 = DIRECTION ( 'NONE',  ( 0.007781995580012662783, 0.000000000000000000, -0.9999697198139514409 ) ) ;
#39263 = DIRECTION ( 'NONE',  ( 0.007781995580012662783, 0.000000000000000000, -0.9999697198139514409 ) ) ;
#39264 = VECTOR ( 'NONE', #42353, 999.9999999999998863 ) ;
#39265 = LINE ( 'NONE', #21403, #13277 ) ;
#39266 = FACE_OUTER_BOUND ( 'NONE', #13928, .T. ) ;
#39267 = ADVANCED_FACE ( 'NONE', ( #26849 ), #44172, .F. ) ;
#39268 = ORIENTED_EDGE ( 'NONE', *, *, #46909, .T. ) ;
#39269 = ORIENTED_EDGE ( 'NONE', *, *, #36419, .F. ) ;
#39270 = CARTESIAN_POINT ( 'NONE',  ( -23.33693525117809386, 0.000000000000000000, 5.746789908705562944 ) ) ;
#39271 = FACE_OUTER_BOUND ( 'NONE', #40956, .T. ) ;
#39272 = VECTOR ( 'NONE', #36098, 1000.000000000000227 ) ;
#39273 = DIRECTION ( 'NONE',  ( 0.000000000000000000, -1.000000000000000000, 0.000000000000000000 ) ) ;
#39274 = AXIS2_PLACEMENT_3D ( 'NONE', #16138, #7070, #49670 ) ;
#39275 = DIRECTION ( 'NONE',  ( 0.7660212471507180654, -0.6427876096865404731, 0.005961354470445141482 ) ) ;
#39276 = AXIS2_PLACEMENT_3D ( 'NONE', #56101, #17186, #52652 ) ;
#39277 = CARTESIAN_POINT ( 'NONE',  ( -16.67577990931724941, -3.270328918600661439, 3.254419731274814875 ) ) ;
#39278 = DIRECTION ( 'NONE',  ( 0.005002170337468016433, -0.7660444431189770143, -0.6427681459581293666 ) ) ;
#39279 = ORIENTED_EDGE ( 'NONE', *, *, #21440, .F. ) ;
#39280 = CARTESIAN_POINT ( 'NONE',  ( -9.908141408373387193, -0.1191753592594197858, 10.77908512878318703 ) ) ;
#39281 = AXIS2_PLACEMENT_3D ( 'NONE', #23019, #19033, #53135 ) ;
#39282 = DIRECTION ( 'NONE',  ( 0.5000000000000011102, -0.8660254037844380415, 0.000000000000000000 ) ) ;
#39283 = AXIS2_PLACEMENT_3D ( 'NONE', #16777, #13376, #270 ) ;
#39284 = ORIENTED_EDGE ( 'NONE', *, *, #51515, .F. ) ;
#39285 = CARTESIAN_POINT ( 'NONE',  ( -24.26908309836554878, 0.000000000000000000, 6.108867788427308376 ) ) ;
#39286 = CARTESIAN_POINT ( 'NONE',  ( 2.072287782118878319, 0.000000000000000000, -2.950529333540147015 ) ) ;
#39287 = CARTESIAN_POINT ( 'NONE',  ( -11.21901323774118708, 0.000000000000000000, 1.039777472322872098 ) ) ;
#39288 = ORIENTED_EDGE ( 'NONE', *, *, #1927, .F. ) ;
#39289 = DIRECTION ( 'NONE',  ( 0.005002170337468016433, -0.7660444431189770143, -0.6427681459581293666 ) ) ;
#39290 = VECTOR ( 'NONE', #14188, 999.9999999999998863 ) ;
#39291 = ADVANCED_FACE ( 'NONE', ( #35362 ), #5657, .T. ) ;
#39292 = ORIENTED_EDGE ( 'NONE', *, *, #339, .T. ) ;
#39293 = AXIS2_PLACEMENT_3D ( 'NONE', #5165, #44885, #48282 ) ;
#39294 = ORIENTED_EDGE ( 'NONE', *, *, #2856, .T. ) ;
#39295 = ORIENTED_EDGE ( 'NONE', *, *, #1095, .T. ) ;
#39296 = ORIENTED_EDGE ( 'NONE', *, *, #6705, .F. ) ;
#39297 = LINE ( 'NONE', #16589, #35698 ) ;
#39299 = EDGE_CURVE ( 'NONE', #50871, #50902, #14358, .T. ) ;
#39298 = ORIENTED_EDGE ( 'NONE', *, *, #29686, .T. ) ;
#39300 = VECTOR ( 'NONE', #8101, 1000.000000000000227 ) ;
#39301 = LINE ( 'NONE', #9479, #33113 ) ;
#39302 = ADVANCED_FACE ( 'NONE', ( #39339 ), #43870, .F. ) ;
#39303 = ORIENTED_EDGE ( 'NONE', *, *, #49130, .F. ) ;
#39304 = CARTESIAN_POINT ( 'NONE',  ( -14.13560388593797335, 5.467268677019012202, 11.34478904033489322 ) ) ;
#39305 = VERTEX_POINT ( 'NONE', #44428 ) ;
#39306 = LINE ( 'NONE', #17432, #36469 ) ;
#39307 = VECTOR ( 'NONE', #31868, 1000.000000000000227 ) ;
#39308 = ORIENTED_EDGE ( 'NONE', *, *, #51872, .F. ) ;
#39309 = EDGE_CURVE ( 'NONE', #21477, #30276, #5534, .T. ) ;
#39310 = CARTESIAN_POINT ( 'NONE',  ( -23.33693525117809386, 0.000000000000000000, 5.746789908705562944 ) ) ;
#39311 = LINE ( 'NONE', #8951, #6891 ) ;
#39312 = DIRECTION ( 'NONE',  ( -0.005961354470445682716, -0.6427876096865404731, 0.7660212471507180654 ) ) ;
#39313 = CARTESIAN_POINT ( 'NONE',  ( -21.47263955680318404, 0.000000000000000000, 5.022634149262071190 ) ) ;
#39314 = AXIS2_PLACEMENT_3D ( 'NONE', #10026, #17996, #1209 ) ;
#39315 = CARTESIAN_POINT ( 'NONE',  ( -26.13337879274045505, 0.000000000000000000, 6.833023547870798353 ) ) ;
#39316 = ORIENTED_EDGE ( 'NONE', *, *, #25933, .T. ) ;
#39317 =( GEOMETRIC_REPRESENTATION_CONTEXT ( 3 ) GLOBAL_UNCERTAINTY_ASSIGNED_CONTEXT ( ( #21150 ) ) GLOBAL_UNIT_ASSIGNED_CONTEXT ( ( #37557, #37861, #50039 ) ) REPRESENTATION_CONTEXT ( 'NONE', 'WORKASPACE' ) );
#39318 = VECTOR ( 'NONE', #784, 1000.000000000000114 ) ;
#39319 = ORIENTED_EDGE ( 'NONE', *, *, #51187, .T. ) ;
#39320 = EDGE_CURVE ( 'NONE', #12870, #47161, #27386, .T. ) ;
#39321 = LINE ( 'NONE', #22293, #47598 ) ;
#39322 = DIRECTION ( 'NONE',  ( -0.6427681459581293666, -0.7660444431189770143, -0.005002170337467561935 ) ) ;
#39323 = EDGE_CURVE ( 'NONE', #30584, #24781, #46108, .T. ) ;
#39324 = CARTESIAN_POINT ( 'NONE',  ( 0.4518049228021099872, -3.655895688227116747, -5.998622290806042479 ) ) ;
#39325 = AXIS2_PLACEMENT_3D ( 'NONE', #11121, #11696, #20504 ) ;
#39326 = AXIS2_PLACEMENT_3D ( 'NONE', #15565, #2233, #41965 ) ;
#39327 = CARTESIAN_POINT ( 'NONE',  ( -16.99924723426068951, 0.000000000000000000, 13.49389102713827171 ) ) ;
#39328 = DIRECTION ( 'NONE',  ( 0.000000000000000000, -1.000000000000000000, 0.000000000000000000 ) ) ;
#39329 = CARTESIAN_POINT ( 'NONE',  ( -32.65841372305263235, 0.000000000000000000, 9.367568705923016381 ) ) ;
#39330 = ORIENTED_EDGE ( 'NONE', *, *, #39697, .F. ) ;
#39331 = PLANE ( 'NONE',  #43805 ) ;
#39332 = CARTESIAN_POINT ( 'NONE',  ( -16.48907833074707341, 0.000000000000000000, 7.646741863706176368 ) ) ;
#39333 = EDGE_LOOP ( 'NONE', ( #56131, #47618, #43418, #10803 ) ) ;
#39334 = ADVANCED_FACE ( 'NONE', ( #20257, #32510 ), #28504, .F. ) ;
#39335 = FACE_OUTER_BOUND ( 'NONE', #43969, .T. ) ;
#39336 = CARTESIAN_POINT ( 'NONE',  ( 2.072287782118878319, 0.000000000000000000, -2.950529333540147015 ) ) ;
#39337 = DIRECTION ( 'NONE',  ( 1.007958083594381669E-15, -3.869188571150966625E-16, 1.000000000000000000 ) ) ;
#39338 = DIRECTION ( 'NONE',  ( 0.007781995580012663651, 0.000000000000000000, -0.9999697198139515519 ) ) ;
#39339 = FACE_OUTER_BOUND ( 'NONE', #35327, .T. ) ;
#39340 = VERTEX_POINT ( 'NONE', #28224 ) ;
#39341 = AXIS2_PLACEMENT_3D ( 'NONE', #25399, #21127, #29942 ) ;
#39342 = ORIENTED_EDGE ( 'NONE', *, *, #25540, .T. ) ;
#39343 = CARTESIAN_POINT ( 'NONE',  ( -13.57904574923490060, -0.1191753592594181482, 4.814734879791510380 ) ) ;
#39344 = CARTESIAN_POINT ( 'NONE',  ( -14.75409303702196873, -3.756034771668162797, 2.492474729652275567 ) ) ;
#39345 = CARTESIAN_POINT ( 'NONE',  ( -27.99923088623136636, 0.000000000000000000, 7.757173251277078130 ) ) ;
#39346 = VECTOR ( 'NONE', #5880, 999.9999999999998863 ) ;
#39347 = CARTESIAN_POINT ( 'NONE',  ( -12.63916579227093173, -0.6798977022406551551, 2.707240912800944699 ) ) ;
#39348 = CARTESIAN_POINT ( 'NONE',  ( -9.542064456761055524, 0.000000000000000000, 10.59726798936431180 ) ) ;
#39349 = VECTOR ( 'NONE', #14667, 999.9999999999998863 ) ;
#39350 = CARTESIAN_POINT ( 'NONE',  ( -15.89757661009962320, 23.47980571057722443, -3.935101339868287251 ) ) ;
#39351 = CARTESIAN_POINT ( 'NONE',  ( -18.66354898467281132, 0.000000000000000000, 14.21960318569776582 ) ) ;
#39352 = VERTEX_POINT ( 'NONE', #15715 ) ;
#39353 = FACE_OUTER_BOUND ( 'NONE', #11824, .T. ) ;
#39354 = CARTESIAN_POINT ( 'NONE',  ( -12.76048694199725553, 0.000000000000000000, 6.198430344819195525 ) ) ;
#39355 = VECTOR ( 'NONE', #24747, 1000.000000000000000 ) ;
#39356 = EDGE_LOOP ( 'NONE', ( #33152, #23510, #35063, #17517 ) ) ;
#39357 = CARTESIAN_POINT ( 'NONE',  ( -13.95021198066316259, 0.000000000000000000, 5.650513546078428817 ) ) ;
#39358 = ORIENTED_EDGE ( 'NONE', *, *, #42262, .T. ) ;
#39359 = DIRECTION ( 'NONE',  ( 0.5364919789714477361, 0.6444004775717706579, 0.5449076811759711036 ) ) ;
#39360 = EDGE_CURVE ( 'NONE', #48042, #6272, #24513, .T. ) ;
#39361 = DIRECTION ( 'NONE',  ( -0.005002170337468016433, -0.7660444431189770143, 0.6427681459581293666 ) ) ;
#39362 = VECTOR ( 'NONE', #35278, 1000.000000000000114 ) ;
#39363 = ORIENTED_EDGE ( 'NONE', *, *, #48746, .T. ) ;
#39364 = EDGE_CURVE ( 'NONE', #21773, #44736, #49811, .T. ) ;
#39365 = ORIENTED_EDGE ( 'NONE', *, *, #36238, .T. ) ;
#39366 = VECTOR ( 'NONE', #39129, 999.9999999999998863 ) ;
#39367 = ORIENTED_EDGE ( 'NONE', *, *, #41847, .T. ) ;
#39368 = EDGE_LOOP ( 'NONE', ( #18829, #24340, #35470, #23217 ) ) ;
#39369 = VECTOR ( 'NONE', #19208, 999.9999999999998863 ) ;
#39370 = ORIENTED_EDGE ( 'NONE', *, *, #18990, .T. ) ;
#39371 = EDGE_CURVE ( 'NONE', #14113, #12863, #14898, .T. ) ;
#39372 = EDGE_LOOP ( 'NONE', ( #16937, #242, #13275, #11821 ) ) ;
#39373 = DIRECTION ( 'NONE',  ( 0.6427681459581294776, -0.7660444431189769032, 0.005002170337467562802 ) ) ;
#39374 = CARTESIAN_POINT ( 'NONE',  ( -16.81267852042391198, -0.1191753592594197858, 3.312241722634738039 ) ) ;
#39375 = CARTESIAN_POINT ( 'NONE',  ( -16.99924723426068951, 0.000000000000000000, 13.49389102713827171 ) ) ;
#39376 = EDGE_CURVE ( 'NONE', #51007, #51066, #28806, .T. ) ;
#39377 = EDGE_CURVE ( 'NONE', #12878, #24462, #41829, .T. ) ;
#39378 = ADVANCED_FACE ( 'NONE', ( #54914 ), #54604, .F. ) ;
#39379 = ORIENTED_EDGE ( 'NONE', *, *, #20470, .F. ) ;
#39380 = CARTESIAN_POINT ( 'NONE',  ( -16.20409152483680870, 3.524445264749008988, 8.959755678013548774 ) ) ;
#39381 = EDGE_LOOP ( 'NONE', ( #42501, #55475, #36423, #1457 ) ) ;
#39382 = ADVANCED_FACE ( 'NONE', ( #36464 ), #29062, .F. ) ;
#39383 = EDGE_LOOP ( 'NONE', ( #10538, #41328, #45428, #12 ) ) ;
#39384 = VECTOR ( 'NONE', #46408, 1000.000000000000227 ) ;
#39385 = FACE_OUTER_BOUND ( 'NONE', #49571, .T. ) ;
#39386 = VECTOR ( 'NONE', #40701, 1000.000000000000227 ) ;
#39387 = CARTESIAN_POINT ( 'NONE',  ( -11.41981228898398548, 1.743523803501505709, 4.178583624546474695 ) ) ;
#39388 = LINE ( 'NONE', #26596, #20508 ) ;
#39389 = VERTEX_POINT ( 'NONE', #6381 ) ;
#39390 = CARTESIAN_POINT ( 'NONE',  ( -23.33849165029409889, 0.000000000000000000, 5.946783852668351855 ) ) ;
#39391 = CIRCLE ( 'NONE', #18499, 2.749999999999998224 ) ;
#39392 = ORIENTED_EDGE ( 'NONE', *, *, #41729, .T. ) ;
#39393 = CARTESIAN_POINT ( 'NONE',  ( -58.00000000000000711, 8.000000000000000000, 2.750000000000008438 ) ) ;
#39394 = EDGE_CURVE ( 'NONE', #29873, #38799, #50371, .T. ) ;
#39396 = AXIS2_PLACEMENT_3D ( 'NONE', #47391, #5097, #4523 ) ;
#39395 = FACE_OUTER_BOUND ( 'NONE', #45737, .T. ) ;
#39397 = EDGE_CURVE ( 'NONE', #5309, #24312, #11483, .T. ) ;
#39398 = LINE ( 'NONE', #47068, #49627 ) ;
#39399 = CARTESIAN_POINT ( 'NONE',  ( -22.35034652457852644, 4.172053068839010059, 12.41000458341346580 ) ) ;
#39400 = DIRECTION ( 'NONE',  ( -0.9999697198139514409, -0.000000000000000000, -0.007781995580013368816 ) ) ;
#39401 = CARTESIAN_POINT ( 'NONE',  ( 2.072287782118878319, 0.000000000000000000, -2.950529333540147015 ) ) ;
#39402 = EDGE_CURVE ( 'NONE', #32587, #6528, #2653, .T. ) ;
#39403 = PLANE ( 'NONE',  #38450 ) ;
#39404 = VECTOR ( 'NONE', #29755, 999.9999999999998863 ) ;
#39405 = CARTESIAN_POINT ( 'NONE',  ( 1.086233639165236964, 0.000000000000000000, 2.796443541562362078 ) ) ;
#39406 = ORIENTED_EDGE ( 'NONE', *, *, #30027, .T. ) ;
#39407 = LINE ( 'NONE', #500, #53731 ) ;
#39408 = AXIS2_PLACEMENT_3D ( 'NONE', #33452, #37723, #20382 ) ;
#39409 = EDGE_CURVE ( 'NONE', #15255, #26117, #54084, .T. ) ;
#39410 = LINE ( 'NONE', #13562, #28322 ) ;
#39411 = LINE ( 'NONE', #51885, #36892 ) ;
#39412 = DIRECTION ( 'NONE',  ( 0.6427681459581294776, -0.7660444431189769032, 0.005002170337467562802 ) ) ;
#39413 = CARTESIAN_POINT ( 'NONE',  ( -19.74387268839167575, 19.52709482682342923, -4.319799108532053289 ) ) ;
#39414 = CARTESIAN_POINT ( 'NONE',  ( -22.40634380310664397, 0.000000000000000000, 5.584705972946605534 ) ) ;
#39415 = EDGE_CURVE ( 'NONE', #50386, #30703, #10666, .T. ) ;
#39416 = DIRECTION ( 'NONE',  ( 0.9999697198139515519, 0.000000000000000000, 0.007781995580013368816 ) ) ;
#39417 = VECTOR ( 'NONE', #42492, 1000.000000000000114 ) ;
#39418 = CARTESIAN_POINT ( 'NONE',  ( -21.09046673295159735, 4.333955019861509328, 12.18633317059820698 ) ) ;
#39419 = VECTOR ( 'NONE', #43526, 999.9999999999998863 ) ;
#39420 = ORIENTED_EDGE ( 'NONE', *, *, #21354, .T. ) ;
#39421 = CARTESIAN_POINT ( 'NONE',  ( -28.35892388567684108, 14.55319269898841661, 4.728968845017322842 ) ) ;
#39422 = CARTESIAN_POINT ( 'NONE',  ( -22.04727804374295275, 19.65758491770980143, 4.422150965879553475 ) ) ;
#39423 = CARTESIAN_POINT ( 'NONE',  ( -14.13583565709953938, 0.000000000000000000, 3.802408630673602019 ) ) ;
#39424 = FACE_OUTER_BOUND ( 'NONE', #54639, .T. ) ;
#39425 = DIRECTION ( 'NONE',  ( 0.007781995580012662783, 0.000000000000000000, -0.9999697198139514409 ) ) ;
#39426 = FACE_OUTER_BOUND ( 'NONE', #46244, .T. ) ;
#39427 = CARTESIAN_POINT ( 'NONE',  ( -15.99725729796916340, 0.000000000000000000, 4.157254686859329418 ) ) ;
#39428 = AXIS2_PLACEMENT_3D ( 'NONE', #26339, #52475, #14151 ) ;
#39429 = CARTESIAN_POINT ( 'NONE',  ( -15.96710241509184058, -0.1191753592594218814, 13.13259134697452879 ) ) ;
#39430 = VECTOR ( 'NONE', #29881, 1000.000000000000227 ) ;
#39431 = DIRECTION ( 'NONE',  ( 0.007781995580012663651, -3.146120232559066537E-19, -0.9999697198139514409 ) ) ;
#39432 = VECTOR ( 'NONE', #18214, 1000.000000000000114 ) ;
#39433 = VERTEX_POINT ( 'NONE', #45532 ) ;
#39434 = CIRCLE ( 'NONE', #29457, 0.5000000000000004441 ) ;
#39435 = ORIENTED_EDGE ( 'NONE', *, *, #48503, .T. ) ;
#39436 = ORIENTED_EDGE ( 'NONE', *, *, #31142, .T. ) ;
#39437 = VECTOR ( 'NONE', #8902, 999.9999999999998863 ) ;
#39438 = EDGE_LOOP ( 'NONE', ( #1731, #25157, #15900, #7958 ) ) ;
#39439 = VECTOR ( 'NONE', #19172, 1000.000000000000227 ) ;
#39440 = ORIENTED_EDGE ( 'NONE', *, *, #26882, .T. ) ;
#39441 = LINE ( 'NONE', #4258, #3329 ) ;
#39442 = DIRECTION ( 'NONE',  ( 0.9999697198139515519, 0.000000000000000000, 0.007781995580013368816 ) ) ;
#39443 = AXIS2_PLACEMENT_3D ( 'NONE', #39176, #38337, #51116 ) ;
#39444 = EDGE_CURVE ( 'NONE', #44308, #51416, #19424, .T. ) ;
#39445 = ADVANCED_FACE ( 'NONE', ( #6652 ), #4653, .T. ) ;
#39446 = VERTEX_POINT ( 'NONE', #48062 ) ;
#39447 = ORIENTED_EDGE ( 'NONE', *, *, #13742, .F. ) ;
#39448 = EDGE_CURVE ( 'NONE', #46834, #23390, #14296, .T. ) ;
#39449 = AXIS2_PLACEMENT_3D ( 'NONE', #21693, #25963, #22245 ) ;
#39450 = VECTOR ( 'NONE', #48111, 1000.000000000000000 ) ;
#39451 = FACE_OUTER_BOUND ( 'NONE', #8996, .T. ) ;
#39452 = ORIENTED_EDGE ( 'NONE', *, *, #22475, .T. ) ;
#39453 = CYLINDRICAL_SURFACE ( 'NONE', #52740, 0.2499999999999998612 ) ;
#39454 = DIRECTION ( 'NONE',  ( 0.000000000000000000, -1.000000000000000000, 0.000000000000000000 ) ) ;
#39455 = ORIENTED_EDGE ( 'NONE', *, *, #34002, .F. ) ;
#39456 = PLANE ( 'NONE',  #32835 ) ;
#39457 = VERTEX_POINT ( 'NONE', #912 ) ;
#39458 = DIRECTION ( 'NONE',  ( 0.000000000000000000, -1.000000000000000000, 0.000000000000000000 ) ) ;
#39459 = VECTOR ( 'NONE', #45832, 999.9999999999998863 ) ;
#39460 = CARTESIAN_POINT ( 'NONE',  ( -25.20200914511100265, -0.1191753592594197858, 6.570942640130446932 ) ) ;
#39461 = DIRECTION ( 'NONE',  ( -0.005961354470445682716, -0.6427876096865404731, 0.7660212471507180654 ) ) ;
#39462 = ORIENTED_EDGE ( 'NONE', *, *, #20753, .T. ) ;
#39463 = CARTESIAN_POINT ( 'NONE',  ( -24.27063949748155380, 0.000000000000000000, 6.308861732390097288 ) ) ;
#39464 = CARTESIAN_POINT ( 'NONE',  ( -9.636218942796791254, 0.000000000000000000, 6.961408260418826544 ) ) ;
#39466 = VECTOR ( 'NONE', #54713, 1000.000000000000227 ) ;
#39465 = FACE_OUTER_BOUND ( 'NONE', #13059, .T. ) ;
#39467 = ORIENTED_EDGE ( 'NONE', *, *, #20239, .T. ) ;
#39468 = LINE ( 'NONE', #568, #2888 ) ;
#39469 = ORIENTED_EDGE ( 'NONE', *, *, #54389, .F. ) ;
#39470 = VECTOR ( 'NONE', #32068, 1000.000000000000114 ) ;
#39471 = DIRECTION ( 'NONE',  ( -0.9999697198139514409, -0.000000000000000000, -0.007781995580013368816 ) ) ;
#39472 = LINE ( 'NONE', #22141, #50484 ) ;
#39473 = CARTESIAN_POINT ( 'NONE',  ( -28.93137873341882127, 0.000000000000000000, 8.119251130998824451 ) ) ;
#39474 = CARTESIAN_POINT ( 'NONE',  ( -9.337105429206005169, -0.06496798097431694119, 2.955599522707465177 ) ) ;
#39475 = VECTOR ( 'NONE', #46645, 1000.000000000000227 ) ;
#39476 = DIRECTION ( 'NONE',  ( 0.5364919789714477361, 0.6444004775717706579, 0.5449076811759711036 ) ) ;
#39477 = EDGE_CURVE ( 'NONE', #12259, #6907, #48912, .T. ) ;
#39478 = CARTESIAN_POINT ( 'NONE',  ( -15.09229358671853127, 0.000000000000000000, 7.288279895752441284 ) ) ;
#39479 = CARTESIAN_POINT ( 'NONE',  ( -12.33850799832341849, 0.000000000000000000, 11.68350162852954632 ) ) ;
#39481 = AXIS2_PLACEMENT_3D ( 'NONE', #51621, #52185, #22646 ) ;
#39480 = CARTESIAN_POINT ( 'NONE',  ( -14.95473343100087149, -2.298917212465658277, 6.263772860196296755 ) ) ;
#39482 = VECTOR ( 'NONE', #44976, 1000.000000000000114 ) ;
#39483 = EDGE_CURVE ( 'NONE', #48148, #8713, #13446, .T. ) ;
#39485 = DIRECTION ( 'NONE',  ( 0.5449076811759707706, 0.6444004775717708799, -0.5364919789714476250 ) ) ;
#39484 = VECTOR ( 'NONE', #29578, 1000.000000000000227 ) ;
#39486 = ORIENTED_EDGE ( 'NONE', *, *, #30304, .T. ) ;
#39487 = LINE ( 'NONE', #25869, #32912 ) ;
#39489 = EDGE_CURVE ( 'NONE', #18842, #9247, #44365, .T. ) ;
#39488 = PLANE ( 'NONE',  #10031 ) ;
#39491 = VECTOR ( 'NONE', #11549, 1000.000000000000227 ) ;
#39490 = LINE ( 'NONE', #16553, #38632 ) ;
#39492 = VECTOR ( 'NONE', #48151, 1000.000000000000114 ) ;
#39493 = ADVANCED_FACE ( 'NONE', ( #659 ), #36148, .F. ) ;
#39494 = DIRECTION ( 'NONE',  ( -0.005002170337468016433, -0.7660444431189770143, 0.6427681459581293666 ) ) ;
#39495 = LINE ( 'NONE', #47736, #18789 ) ;
#39496 = DIRECTION ( 'NONE',  ( -0.5449076811759708816, 0.6444004775717707689, 0.5364919789714475140 ) ) ;
#39497 = VERTEX_POINT ( 'NONE', #26478 ) ;
#39498 = VECTOR ( 'NONE', #33825, 1000.000000000000227 ) ;
#39499 = AXIS2_PLACEMENT_3D ( 'NONE', #44415, #5812, #5519 ) ;
#39500 = ORIENTED_EDGE ( 'NONE', *, *, #45901, .F. ) ;
#39501 =( BOUNDED_CURVE ( )  B_SPLINE_CURVE ( 3, ( #21584, #56201, #30665, #39155 ),
 .UNSPECIFIED., .F., .F. ) 
 B_SPLINE_CURVE_WITH_KNOTS ( ( 4, 4 ),
 ( 3.528432781240732563, 5.142782291042179210 ),
 .UNSPECIFIED. ) 
 CURVE ( )  GEOMETRIC_REPRESENTATION_ITEM ( )  RATIONAL_B_SPLINE_CURVE ( ( 1.000000000000000000, 0.7943613114863588009, 0.7943613114863588009, 1.000000000000000000 ) ) 
 REPRESENTATION_ITEM ( '' )  );
#39502 = CYLINDRICAL_SURFACE ( 'NONE', #22282, 0.5000000000000004441 ) ;
#39503 = CARTESIAN_POINT ( 'NONE',  ( -14.46888367232926420, 0.000000000000000000, 12.59025272694991315 ) ) ;
#39504 = DIRECTION ( 'NONE',  ( 0.7660212471507180654, -0.6427876096865404731, 0.005961354470445141482 ) ) ;
#39505 = VERTEX_POINT ( 'NONE', #48334 ) ;
#39506 = FACE_OUTER_BOUND ( 'NONE', #4600, .T. ) ;
#39507 = ORIENTED_EDGE ( 'NONE', *, *, #8349, .F. ) ;
#39508 = CARTESIAN_POINT ( 'NONE',  ( -27.99923088623136636, 0.000000000000000000, 7.757173251277078130 ) ) ;
#39509 = VECTOR ( 'NONE', #42358, 1000.000000000000227 ) ;
#39510 = VERTEX_POINT ( 'NONE', #43795 ) ;
#39511 = ORIENTED_EDGE ( 'NONE', *, *, #397, .T. ) ;
#39512 = ORIENTED_EDGE ( 'NONE', *, *, #50301, .F. ) ;
#39513 = VECTOR ( 'NONE', #51974, 1000.000000000000227 ) ;
#39514 = DIRECTION ( 'NONE',  ( 0.5449076811759707706, 0.6444004775717708799, -0.5364919789714476250 ) ) ;
#39515 = DIRECTION ( 'NONE',  ( -0.6427681459581293666, -0.7660444431189770143, -0.005002170337467561935 ) ) ;
#39516 = VECTOR ( 'NONE', #35416, 1000.000000000000227 ) ;
#39517 = LINE ( 'NONE', #48018, #6724 ) ;
#39518 = ADVANCED_FACE ( 'NONE', ( #53448 ), #5752, .F. ) ;
#39519 = DIRECTION ( 'NONE',  ( 0.005961354470445682716, -0.6427876096865404731, -0.7660212471507180654 ) ) ;
#39520 = ORIENTED_EDGE ( 'NONE', *, *, #12487, .T. ) ;
#39521 = VECTOR ( 'NONE', #33522, 999.9999999999998863 ) ;
#39522 = ORIENTED_EDGE ( 'NONE', *, *, #34401, .T. ) ;
#39523 = EDGE_CURVE ( 'NONE', #52679, #25619, #39569, .T. ) ;
#39524 = ADVANCED_FACE ( 'NONE', ( #39266 ), #35301, .F. ) ;
#39525 = AXIS2_PLACEMENT_3D ( 'NONE', #24769, #20525, #15409 ) ;
#39526 = AXIS2_PLACEMENT_3D ( 'NONE', #33620, #37319, #19451 ) ;
#39527 = LINE ( 'NONE', #52306, #31819 ) ;
#39528 = EDGE_LOOP ( 'NONE', ( #50527, #55395, #22176, #10619 ) ) ;
#39529 = DIRECTION ( 'NONE',  ( 0.7660212471507180654, -0.6427876096865404731, 0.005961354470445141482 ) ) ;
#39530 = ORIENTED_EDGE ( 'NONE', *, *, #48019, .F. ) ;
#39531 = CARTESIAN_POINT ( 'NONE',  ( -21.96445785857699562, 4.333955019861511992, 5.075397224011642727 ) ) ;
#39532 = DIRECTION ( 'NONE',  ( 0.7660212471507180654, -0.6427876096865404731, 0.005961354470445141482 ) ) ;
#39533 = VECTOR ( 'NONE', #32757, 999.9999999999998863 ) ;
#39534 = ORIENTED_EDGE ( 'NONE', *, *, #37015, .T. ) ;
#39535 = VECTOR ( 'NONE', #52446, 999.9999999999998863 ) ;
#39536 = CARTESIAN_POINT ( 'NONE',  ( 0.000000000000000000, 0.000000000000000000, 0.000000000000000000 ) ) ;
#39537 = VECTOR ( 'NONE', #48195, 999.9999999999998863 ) ;
#39538 = ORIENTED_EDGE ( 'NONE', *, *, #27450, .F. ) ;
#39539 = ADVANCED_FACE ( 'NONE', ( #53190, #23072 ), #17694, .F. ) ;
#39540 = VECTOR ( 'NONE', #21188, 999.9999999999998863 ) ;
#39541 = DIRECTION ( 'NONE',  ( 0.000000000000000000, -0.000000000000000000, -1.000000000000000000 ) ) ;
#39542 = VECTOR ( 'NONE', #11254, 1000.000000000000114 ) ;
#39543 = VERTEX_POINT ( 'NONE', #31314 ) ;
#39544 = PLANE ( 'NONE',  #45876 ) ;
#39545 = DIRECTION ( 'NONE',  ( -0.005002170337468016433, -0.7660444431189770143, 0.6427681459581293666 ) ) ;
#39546 = CARTESIAN_POINT ( 'NONE',  ( -12.23851102634202448, -0.1191753592594197858, 11.68427982808754884 ) ) ;
#39547 = EDGE_LOOP ( 'NONE', ( #30035, #55392, #52350, #55276 ) ) ;
#39548 = CARTESIAN_POINT ( 'NONE',  ( -16.79925329029790149, 0.000000000000000000, 13.49544742625427496 ) ) ;
#39549 = DIRECTION ( 'NONE',  ( 0.000000000000000000, -1.000000000000000000, 0.000000000000000000 ) ) ;
#39550 = CARTESIAN_POINT ( 'NONE',  ( -19.86151716922415034, 0.000000000000000000, 4.496514192825078915 ) ) ;
#39551 = DIRECTION ( 'NONE',  ( 0.6427681459581294776, -0.7660444431189769032, 0.005002170337467562802 ) ) ;
#39552 = CARTESIAN_POINT ( 'NONE',  ( -15.28175012032331459, 3.038739411681508518, 2.520930751862971331 ) ) ;
#39553 = CARTESIAN_POINT ( 'NONE',  ( -25.20278734466900517, 0.000000000000000000, 6.670939612111840944 ) ) ;
#39554 = AXIS2_PLACEMENT_3D ( 'NONE', #13248, #18315, #30278 ) ;
#39555 = ORIENTED_EDGE ( 'NONE', *, *, #28711, .F. ) ;
#39556 = CARTESIAN_POINT ( 'NONE',  ( -15.13495153988577968, 0.000000000000000000, 12.76973526769478084 ) ) ;
#39557 = DIRECTION ( 'NONE',  ( -0.5449076811759708816, 0.6444004775717707689, 0.5364919789714475140 ) ) ;
#39558 = PLANE ( 'NONE',  #12405 ) ;
#39559 = ORIENTED_EDGE ( 'NONE', *, *, #3850, .T. ) ;
#39560 = FACE_OUTER_BOUND ( 'NONE', #33028, .T. ) ;
#39561 = CARTESIAN_POINT ( 'NONE',  ( 4.912750499197525933, -1.131233082521086342, 2.029539223447463403 ) ) ;
#39562 = VECTOR ( 'NONE', #8686, 1000.000000000000000 ) ;
#39563 = ORIENTED_EDGE ( 'NONE', *, *, #39713, .T. ) ;
#39564 = DIRECTION ( 'NONE',  ( 0.007781995580012663651, -3.146120232559066537E-19, -0.9999697198139514409 ) ) ;
#39565 = ADVANCED_FACE ( 'NONE', ( #35564 ), #26770, .F. ) ;
#39566 = LINE ( 'NONE', #17393, #28443 ) ;
#39567 = VECTOR ( 'NONE', #41140, 1000.000000000000227 ) ;
#39568 = CARTESIAN_POINT ( 'NONE',  ( -25.20278734466900517, 0.000000000000000000, 6.670939612111840944 ) ) ;
#39569 = LINE ( 'NONE', #10006, #32845 ) ;
#39570 = ORIENTED_EDGE ( 'NONE', *, *, #40012, .F. ) ;
#39571 = AXIS2_PLACEMENT_3D ( 'NONE', #44950, #1204, #39845 ) ;
#39572 = VECTOR ( 'NONE', #18866, 1000.000000000000000 ) ;
#39573 = ORIENTED_EDGE ( 'NONE', *, *, #13357, .T. ) ;
#39574 = PLANE ( 'NONE',  #18572 ) ;
#39575 = CARTESIAN_POINT ( 'NONE',  ( -9.765605855588104234, 0.000000000000000000, 5.313747048732751388 ) ) ;
#39576 = CARTESIAN_POINT ( 'NONE',  ( -69.43561177275644525, -9.791245164465275153, -7.501782499249458169 ) ) ;
#39577 = VECTOR ( 'NONE', #37634, 1000.000000000000114 ) ;
#39578 = EDGE_CURVE ( 'NONE', #29224, #55190, #27318, .T. ) ;
#39579 = CARTESIAN_POINT ( 'NONE',  ( -62.23823698199102950, 6.658783344088819334, -5.000000000000000000 ) ) ;
#39581 = DIRECTION ( 'NONE',  ( 0.5449076811759707706, 0.6444004775717708799, -0.5364919789714476250 ) ) ;
#39580 = AXIS2_PLACEMENT_3D ( 'NONE', #54053, #23655, #54321 ) ;
#39582 = DIRECTION ( 'NONE',  ( -0.005002170337468016433, -0.7660444431189770143, 0.6427681459581293666 ) ) ;
#39584 = EDGE_CURVE ( 'NONE', #40212, #47084, #8916, .T. ) ;
#39583 = ORIENTED_EDGE ( 'NONE', *, *, #50006, .T. ) ;
#39585 = DIRECTION ( 'NONE',  ( -0.005002170337468016433, -0.7660444431189770143, 0.6427681459581293666 ) ) ;
#39586 = EDGE_CURVE ( 'NONE', #32587, #11776, #21939, .T. ) ;
#39587 = AXIS2_PLACEMENT_3D ( 'NONE', #25322, #46058, #38373 ) ;
#39588 = AXIS2_PLACEMENT_3D ( 'NONE', #26847, #17195, #44170 ) ;
#39589 = CARTESIAN_POINT ( 'NONE',  ( -15.86710544311044302, 0.000000000000000000, 13.13336954653252953 ) ) ;
#39590 = EDGE_LOOP ( 'NONE', ( #55146, #17457, #9111, #4582 ) ) ;
#39591 = DIRECTION ( 'NONE',  ( 0.5449076811759707706, 0.6444004775717708799, -0.5364919789714476250 ) ) ;
#39592 = EDGE_CURVE ( 'NONE', #42084, #5690, #39833, .T. ) ;
#39593 = DIRECTION ( 'NONE',  ( 0.9999697198139515519, 0.000000000000000000, 0.007781995580013368816 ) ) ;
#39594 = LINE ( 'NONE', #40419, #51987 ) ;
#39595 = ORIENTED_EDGE ( 'NONE', *, *, #34340, .T. ) ;
#39596 = DIRECTION ( 'NONE',  ( 0.6427681459581294776, -0.7660444431189769032, 0.005002170337467562802 ) ) ;
#39597 = ADVANCED_FACE ( 'NONE', ( #18522 ), #10594, .F. ) ;
#39598 = ORIENTED_EDGE ( 'NONE', *, *, #32306, .F. ) ;
#39599 = EDGE_CURVE ( 'NONE', #47757, #11984, #23895, .T. ) ;
#39600 = VECTOR ( 'NONE', #38636, 1000.000000000000000 ) ;
#39601 = ORIENTED_EDGE ( 'NONE', *, *, #10376, .F. ) ;
#39602 = ORIENTED_EDGE ( 'NONE', *, *, #8635, .F. ) ;
#39603 = ORIENTED_EDGE ( 'NONE', *, *, #28741, .T. ) ;
#39604 = LINE ( 'NONE', #48088, #46573 ) ;
#39605 = VECTOR ( 'NONE', #15310, 1000.000000000000227 ) ;
#39606 = VERTEX_POINT ( 'NONE', #27908 ) ;
#39607 = CARTESIAN_POINT ( 'NONE',  ( -11.62127938944716377, 0.000000000000000000, 4.929973698402949189 ) ) ;
#39608 = EDGE_CURVE ( 'NONE', #8988, #54304, #11108, .T. ) ;
#39609 = ORIENTED_EDGE ( 'NONE', *, *, #20775, .T. ) ;
#39610 = DIRECTION ( 'NONE',  ( 0.9999697198139515519, 0.000000000000000000, 0.007781995580013368816 ) ) ;
#39611 = VECTOR ( 'NONE', #31178, 1000.000000000000227 ) ;
#39612 = ORIENTED_EDGE ( 'NONE', *, *, #9713, .F. ) ;
#39613 = CARTESIAN_POINT ( 'NONE',  ( -19.79569077582305070, 0.000000000000000000, 14.58012466630350445 ) ) ;
#39614 = ORIENTED_EDGE ( 'NONE', *, *, #6738, .F. ) ;
#39615 = EDGE_CURVE ( 'NONE', #12878, #35417, #32691, .T. ) ;
#39616 = VECTOR ( 'NONE', #49867, 999.9999999999998863 ) ;
#39617 = DIRECTION ( 'NONE',  ( -0.9999697198139514409, -0.000000000000000000, -0.007781995580013368816 ) ) ;
#39618 = CARTESIAN_POINT ( 'NONE',  ( -9.463279351066496758, -0.1191753592594187727, 2.630772306739904032 ) ) ;
#39619 = DIRECTION ( 'NONE',  ( -0.5449076811759708816, 0.6444004775717707689, 0.5364919789714475140 ) ) ;
#39620 = DIRECTION ( 'NONE',  ( -0.5449076811759708816, 0.6444004775717707689, 0.5364919789714475140 ) ) ;
#39621 = LINE ( 'NONE', #22288, #27456 ) ;
#39622 = VERTEX_POINT ( 'NONE', #15640 ) ;
#39623 = ORIENTED_EDGE ( 'NONE', *, *, #28296, .F. ) ;
#39624 = AXIS2_PLACEMENT_3D ( 'NONE', #34304, #34859, #43097 ) ;
#39625 = CARTESIAN_POINT ( 'NONE',  ( -9.397313677665129816, -0.1191753592594181482, 4.847278085703597306 ) ) ;
#39626 = FACE_OUTER_BOUND ( 'NONE', #32817, .T. ) ;
#39627 = AXIS2_PLACEMENT_3D ( 'NONE', #1649, #22949, #9905 ) ;
#39628 = DIRECTION ( 'NONE',  ( 0.5449076811759707706, 0.6444004775717708799, -0.5364919789714476250 ) ) ;
#39629 = AXIS2_PLACEMENT_3D ( 'NONE', #37751, #54219, #19852 ) ;
#39630 = DIRECTION ( 'NONE',  ( 0.6427681459581294776, -0.7660444431189769032, 0.005002170337467562802 ) ) ;
#39631 = DIRECTION ( 'NONE',  ( 0.6427681459581294776, -0.7660444431189769032, 0.005002170337467562802 ) ) ;
#39632 = LINE ( 'NONE', #5266, #15949 ) ;
#39633 = VERTEX_POINT ( 'NONE', #45750 ) ;
#39634 = PLANE ( 'NONE',  #30245 ) ;
#39635 = DIRECTION ( 'NONE',  ( -0.9983709377222390602, -0.05705673239519638146, 0.000000000000000000 ) ) ;
#39636 = ORIENTED_EDGE ( 'NONE', *, *, #7305, .T. ) ;
#39637 = FACE_OUTER_BOUND ( 'NONE', #5180, .T. ) ;
#39638 = DIRECTION ( 'NONE',  ( -0.5449076811759708816, 0.6444004775717707689, 0.5364919789714475140 ) ) ;
#39639 = EDGE_CURVE ( 'NONE', #23263, #54036, #19073, .T. ) ;
#39640 = CARTESIAN_POINT ( 'NONE',  ( -16.33317936670417225, 0.000000000000000000, 13.31440848639340224 ) ) ;
#39641 = CARTESIAN_POINT ( 'NONE',  ( -20.54204810873173415, 0.000000000000000000, 4.860550213503115558 ) ) ;
#39642 = AXIS2_PLACEMENT_3D ( 'NONE', #24765, #33849, #16245 ) ;
#39643 = LINE ( 'NONE', #53511, #49185 ) ;
#39644 = ORIENTED_EDGE ( 'NONE', *, *, #55538, .T. ) ;
#39645 = ORIENTED_EDGE ( 'NONE', *, *, #4579, .T. ) ;
#39646 = CARTESIAN_POINT ( 'NONE',  ( -32.65997012216863737, 0.000000000000000000, 9.567562649885804404 ) ) ;
#39647 = CARTESIAN_POINT ( 'NONE',  ( 2.072287782118878319, 0.000000000000000000, -2.950529333540147015 ) ) ;
#39648 = PLANE ( 'NONE',  #32434 ) ;
#39649 = DIRECTION ( 'NONE',  ( 0.000000000000000000, -0.000000000000000000, -1.000000000000000000 ) ) ;
#39650 = VECTOR ( 'NONE', #36033, 999.9999999999998863 ) ;
#39651 = LINE ( 'NONE', #5541, #8604 ) ;
#39652 = LINE ( 'NONE', #52673, #52730 ) ;
#39653 = DIRECTION ( 'NONE',  ( -0.005002170337468016433, -0.7660444431189770143, 0.6427681459581293666 ) ) ;
#39654 = EDGE_CURVE ( 'NONE', #45114, #53352, #6052, .T. ) ;
#39656 = VECTOR ( 'NONE', #45011, 1000.000000000000227 ) ;
#39655 = LINE ( 'NONE', #17480, #545 ) ;
#39657 = DIRECTION ( 'NONE',  ( -0.5364919789714478471, 0.6444004775717705469, -0.5449076811759709926 ) ) ;
#39658 = VERTEX_POINT ( 'NONE', #6874 ) ;
#39659 = DIRECTION ( 'NONE',  ( -0.005002170337468016433, -0.7660444431189770143, 0.6427681459581293666 ) ) ;
#39660 = ORIENTED_EDGE ( 'NONE', *, *, #24695, .T. ) ;
#39661 = DIRECTION ( 'NONE',  ( 0.007781995580012662783, 0.000000000000000000, -0.9999697198139514409 ) ) ;
#39662 = LINE ( 'NONE', #741, #36592 ) ;
#39663 = ORIENTED_EDGE ( 'NONE', *, *, #19860, .T. ) ;
#39664 = VECTOR ( 'NONE', #55882, 1000.000000000000227 ) ;
#39665 = LINE ( 'NONE', #40768, #45364 ) ;
#39666 = EDGE_CURVE ( 'NONE', #19164, #47613, #50163, .T. ) ;
#39667 = ORIENTED_EDGE ( 'NONE', *, *, #38476, .T. ) ;
#39668 = EDGE_CURVE ( 'NONE', #50804, #16658, #2317, .T. ) ;
#39669 = ORIENTED_EDGE ( 'NONE', *, *, #31248, .T. ) ;
#39670 = ORIENTED_EDGE ( 'NONE', *, *, #4543, .T. ) ;
#39671 = VERTEX_POINT ( 'NONE', #54834 ) ;
#39672 = ORIENTED_EDGE ( 'NONE', *, *, #26905, .T. ) ;
#39673 = CARTESIAN_POINT ( 'NONE',  ( 1.971453974394196562, 0.000000000000000000, 10.00639841352631088 ) ) ;
#39674 = LINE ( 'NONE', #13800, #19487 ) ;
#39675 = EDGE_CURVE ( 'NONE', #6706, #45963, #2595, .T. ) ;
#39676 = ORIENTED_EDGE ( 'NONE', *, *, #24051, .F. ) ;
#39677 = DIRECTION ( 'NONE',  ( 0.5364919789714477361, 0.6444004775717706579, 0.5449076811759711036 ) ) ;
#39678 = EDGE_LOOP ( 'NONE', ( #31496, #21585, #5789, #11407 ) ) ;
#39679 = ORIENTED_EDGE ( 'NONE', *, *, #37906, .F. ) ;
#39680 = ADVANCED_FACE ( 'NONE', ( #45466 ), #28735, .F. ) ;
#39681 = DIRECTION ( 'NONE',  ( -0.5364919789714478471, 0.6444004775717705469, -0.5449076811759709926 ) ) ;
#39682 = CARTESIAN_POINT ( 'NONE',  ( 4.966775449259088759, -1.125037814383460288, 2.247047898273225375 ) ) ;
#39683 = CARTESIAN_POINT ( 'NONE',  ( -28.92982233430281980, 0.000000000000000000, 7.919257187036034651 ) ) ;
#39684 = ORIENTED_EDGE ( 'NONE', *, *, #7464, .T. ) ;
#39685 = CARTESIAN_POINT ( 'NONE',  ( -25.20278734466900517, 0.000000000000000000, 6.670939612111840944 ) ) ;
#39686 = ORIENTED_EDGE ( 'NONE', *, *, #41986, .T. ) ;
#39687 = LINE ( 'NONE', #17827, #18459 ) ;
#39688 = CARTESIAN_POINT ( 'NONE',  ( -14.89229964275573970, 0.000000000000000000, 7.289836294868443645 ) ) ;
#39689 = VECTOR ( 'NONE', #133, 1000.000000000000227 ) ;
#39690 = PLANE ( 'NONE',  #45822 ) ;
#39691 = DIRECTION ( 'NONE',  ( 0.007781995580012662783, 0.000000000000000000, -0.9999697198139514409 ) ) ;
#39692 = CARTESIAN_POINT ( 'NONE',  ( -21.47263955680318404, 0.000000000000000000, 5.022634149262071190 ) ) ;
#39693 = DIRECTION ( 'NONE',  ( -0.005961354470445682716, -0.6427876096865404731, 0.7660212471507180654 ) ) ;
#39694 = LINE ( 'NONE', #18948, #33145 ) ;
#39695 = ORIENTED_EDGE ( 'NONE', *, *, #37790, .F. ) ;
#39696 = DIRECTION ( 'NONE',  ( -0.005961354470445682716, -0.6427876096865404731, 0.7660212471507180654 ) ) ;
#39697 = EDGE_CURVE ( 'NONE', #41918, #54227, #36550, .T. ) ;
#39698 = VECTOR ( 'NONE', #40988, 999.9999999999998863 ) ;
#39699 = CYLINDRICAL_SURFACE ( 'NONE', #45594, 2.125000000000000000 ) ;
#39700 = FACE_OUTER_BOUND ( 'NONE', #38416, .T. ) ;
#39701 = PLANE ( 'NONE',  #32646 ) ;
#39702 = ADVANCED_FACE ( 'NONE', ( #36399 ), #31862, .F. ) ;
#39703 = CARTESIAN_POINT ( 'NONE',  ( -26.72368083891871748, 15.49730071222468553, -4.674120403987057415 ) ) ;
#39704 = DIRECTION ( 'NONE',  ( -0.005002170337468016433, -0.7660444431189770143, 0.6427681459581293666 ) ) ;
#39705 = DIRECTION ( 'NONE',  ( -0.005002170337468016433, -0.7660444431189770143, 0.6427681459581293666 ) ) ;
#39706 = DIRECTION ( 'NONE',  ( -0.5449076811759708816, 0.6444004775717707689, 0.5364919789714475140 ) ) ;
#39707 = ADVANCED_FACE ( 'NONE', ( #40682 ), #32154, .F. ) ;
#39708 = EDGE_LOOP ( 'NONE', ( #15270, #27563, #40345, #1272 ) ) ;
#39709 = EDGE_CURVE ( 'NONE', #44124, #44724, #49748, .T. ) ;
#39710 = CARTESIAN_POINT ( 'NONE',  ( -28.36653009681956661, 14.54880125093765386, 4.729224108455964526 ) ) ;
#39711 = PLANE ( 'NONE',  #17649 ) ;
#39712 = CARTESIAN_POINT ( 'NONE',  ( -14.01701317841955508, 0.000000000000000000, 2.326005055450897085 ) ) ;
#39713 = EDGE_CURVE ( 'NONE', #45704, #47757, #16484, .T. ) ;
#39714 = EDGE_CURVE ( 'NONE', #35993, #40047, #9565, .T. ) ;
#39715 = EDGE_CURVE ( 'NONE', #17269, #2394, #21024, .T. ) ;
#39716 = CARTESIAN_POINT ( 'NONE',  ( -22.40478740399063895, 0.000000000000000000, 5.384712028983816623 ) ) ;
#39717 = LINE ( 'NONE', #18111, #1290 ) ;
#39718 = DIRECTION ( 'NONE',  ( -0.7660212471507179544, -0.6427876096865405842, -0.005961354470445141482 ) ) ;
#39719 = DIRECTION ( 'NONE',  ( -0.8531650599175527594, 0.4028455766673922356, 0.3313982828793700652 ) ) ;
#39720 = CYLINDRICAL_SURFACE ( 'NONE', #7869, 6.999999999999999112 ) ;
#39721 = DIRECTION ( 'NONE',  ( 0.007781995580012662783, 0.000000000000000000, -0.9999697198139514409 ) ) ;
#39722 = EDGE_LOOP ( 'NONE', ( #50867, #43054, #46984, #14973 ) ) ;
#39723 = ADVANCED_FACE ( 'NONE', ( #38653 ), #37818, .F. ) ;
#39724 = ADVANCED_FACE ( 'NONE', ( #55129 ), #33538, .F. ) ;
#39725 = ORIENTED_EDGE ( 'NONE', *, *, #8901, .T. ) ;
#39726 = VERTEX_POINT ( 'NONE', #3999 ) ;
#39727 = VERTEX_POINT ( 'NONE', #42047 ) ;
#39728 = EDGE_CURVE ( 'NONE', #42362, #14988, #34117, .T. ) ;
#39729 = ORIENTED_EDGE ( 'NONE', *, *, #50187, .T. ) ;
#39730 = PLANE ( 'NONE',  #10607 ) ;
#39731 = DIRECTION ( 'NONE',  ( -0.8660254037844379305, -0.5000000000000011102, 0.000000000000000000 ) ) ;
#39732 = EDGE_CURVE ( 'NONE', #38932, #42567, #29269, .T. ) ;
#39733 = AXIS2_PLACEMENT_3D ( 'NONE', #28417, #41497, #2579 ) ;
#39734 = ORIENTED_EDGE ( 'NONE', *, *, #49247, .F. ) ;
#39735 = EDGE_LOOP ( 'NONE', ( #16724, #43130 ) ) ;
#39736 = CARTESIAN_POINT ( 'NONE',  ( -12.80458192191714595, 0.000000000000000000, 11.86454056839041726 ) ) ;
#39737 = VERTEX_POINT ( 'NONE', #38352 ) ;
#39738 = CARTESIAN_POINT ( 'NONE',  ( -56.70083583094844926, 4.876814673940706335, -3.000000000000007105 ) ) ;
#39739 = DIRECTION ( 'NONE',  ( 0.000000000000000000, -0.000000000000000000, -1.000000000000000000 ) ) ;
#39740 = VERTEX_POINT ( 'NONE', #7404 ) ;
#39741 = LINE ( 'NONE', #9643, #32035 ) ;
#39742 = ORIENTED_EDGE ( 'NONE', *, *, #46063, .T. ) ;
#39743 = CARTESIAN_POINT ( 'NONE',  ( -16.81345671998191449, 0.000000000000000000, 3.412238694616132495 ) ) ;
#39744 = DIRECTION ( 'NONE',  ( 0.005961354470445682716, -0.6427876096865404731, -0.7660212471507180654 ) ) ;
#39745 = LINE ( 'NONE', #5380, #8274 ) ;
#39746 = FACE_OUTER_BOUND ( 'NONE', #6012, .T. ) ;
#39747 = ORIENTED_EDGE ( 'NONE', *, *, #27467, .F. ) ;
#39748 = CARTESIAN_POINT ( 'NONE',  ( -14.10280672071693431, -0.1191753592594197858, 12.40843558753103792 ) ) ;
#39749 = CARTESIAN_POINT ( 'NONE',  ( -14.95573478672749346, -0.1191753592594190225, 2.590941714392399842 ) ) ;
#39750 = PLANE ( 'NONE',  #52036 ) ;
#39751 = ORIENTED_EDGE ( 'NONE', *, *, #6740, .T. ) ;
#39752 = DIRECTION ( 'NONE',  ( -0.005961354470445682716, -0.6427876096865404731, 0.7660212471507180654 ) ) ;
#39753 = VERTEX_POINT ( 'NONE', #50588 ) ;
#39754 = CARTESIAN_POINT ( 'NONE',  ( -17.74482636761137044, -0.1191753592594197858, 3.674319602356483916 ) ) ;
#39755 = LINE ( 'NONE', #35226, #26907 ) ;
#39756 = LINE ( 'NONE', #835, #46715 ) ;
#39757 = DIRECTION ( 'NONE',  ( 0.000000000000000000, -1.000000000000000000, 0.000000000000000000 ) ) ;
#39758 = CARTESIAN_POINT ( 'NONE',  ( -18.94948708026818807, 4.010151117816509903, 10.82328659761999567 ) ) ;
#39759 = CARTESIAN_POINT ( 'NONE',  ( -24.27063949748155380, 0.000000000000000000, 6.308861732390097288 ) ) ;
#39760 = DIRECTION ( 'NONE',  ( 0.000000000000000000, -0.000000000000000000, -1.000000000000000000 ) ) ;
#39761 = PLANE ( 'NONE',  #1198 ) ;
#39762 =( LENGTH_UNIT ( ) NAMED_UNIT ( * ) SI_UNIT ( .MILLI., .METRE. ) );
#39763 = LINE ( 'NONE', #53104, #4220 ) ;
#39764 = ORIENTED_EDGE ( 'NONE', *, *, #38678, .F. ) ;
#39765 = DIRECTION ( 'NONE',  ( -0.5364919789714478471, 0.6444004775717705469, -0.5449076811759709926 ) ) ;
#39766 = CARTESIAN_POINT ( 'NONE',  ( -17.44252728881015102, 0.6102101463440037232, 4.658049875088040359 ) ) ;
#39767 = FACE_OUTER_BOUND ( 'NONE', #42153, .T. ) ;
#39768 = LINE ( 'NONE', #13627, #42279 ) ;
#39769 = EDGE_CURVE ( 'NONE', #3456, #17353, #29852, .T. ) ;
#39770 = EDGE_CURVE ( 'NONE', #47757, #54534, #21617, .T. ) ;
#39771 = VECTOR ( 'NONE', #121, 1000.000000000000114 ) ;
#39772 = LINE ( 'NONE', #43721, #25866 ) ;
#39773 = EDGE_CURVE ( 'NONE', #27291, #9862, #55677, .T. ) ;
#39774 = CARTESIAN_POINT ( 'NONE',  ( -26.13337879274045505, 0.000000000000000000, 6.833023547870798353 ) ) ;
#39775 = DIRECTION ( 'NONE',  ( 0.5449076811759707706, 0.6444004775717708799, -0.5364919789714476250 ) ) ;
#39776 = ORIENTED_EDGE ( 'NONE', *, *, #48325, .T. ) ;
#39777 = ORIENTED_EDGE ( 'NONE', *, *, #54210, .T. ) ;
#39778 = DIRECTION ( 'NONE',  ( 0.9999697198139515519, 0.000000000000000000, 0.007781995580013368816 ) ) ;
#39779 = DIRECTION ( 'NONE',  ( -0.005002170337468016433, -0.7660444431189770143, 0.6427681459581293666 ) ) ;
#39780 = EDGE_LOOP ( 'NONE', ( #33167, #50373, #53209, #13538 ) ) ;
#39781 = DIRECTION ( 'NONE',  ( 0.007781995580012663651, 0.000000000000000000, -0.9999697198139515519 ) ) ;
#39782 = ORIENTED_EDGE ( 'NONE', *, *, #46237, .F. ) ;
#39783 = LINE ( 'NONE', #9388, #41089 ) ;
#39784 = EDGE_CURVE ( 'NONE', #18005, #41229, #50844, .T. ) ;
#39785 = EDGE_LOOP ( 'NONE', ( #13336, #8268, #10814, #3092 ) ) ;
#39786 = ORIENTED_EDGE ( 'NONE', *, *, #42198, .F. ) ;
#39787 = ORIENTED_EDGE ( 'NONE', *, *, #36688, .F. ) ;
#39788 = EDGE_CURVE ( 'NONE', #55101, #35565, #11942, .T. ) ;
#39789 = LINE ( 'NONE', #31816, #47462 ) ;
#39790 = PLANE ( 'NONE',  #11436 ) ;
#39791 = PLANE ( 'NONE',  #21226 ) ;
#39792 = ADVANCED_FACE ( 'NONE', ( #47434 ), #3151, .F. ) ;
#39793 = CARTESIAN_POINT ( 'NONE',  ( -25.20278734466900517, 0.000000000000000000, 6.670939612111840944 ) ) ;
#39794 = EDGE_LOOP ( 'NONE', ( #13471, #36779, #13590, #4923 ) ) ;
#39795 = EDGE_LOOP ( 'NONE', ( #41352, #26465, #28254, #50403 ) ) ;
#39796 = ADVANCED_FACE ( 'NONE', ( #8546 ), #51130, .F. ) ;
#39797 = PLANE ( 'NONE',  #47247 ) ;
#39798 = ORIENTED_EDGE ( 'NONE', *, *, #15268, .F. ) ;
#39799 = DIRECTION ( 'NONE',  ( -0.5449076811759708816, 0.6444004775717707689, 0.5364919789714475140 ) ) ;
#39800 = VERTEX_POINT ( 'NONE', #25568 ) ;
#39801 = DIRECTION ( 'NONE',  ( 0.5364919789714477361, 0.6444004775717706579, 0.5449076811759711036 ) ) ;
#39802 = CARTESIAN_POINT ( 'NONE',  ( -14.00280974873554030, 0.000000000000000000, 12.40921378708904044 ) ) ;
#39803 = VECTOR ( 'NONE', #5206, 1000.000000000000000 ) ;
#39804 = ORIENTED_EDGE ( 'NONE', *, *, #7385, .T. ) ;
#39805 = FACE_OUTER_BOUND ( 'NONE', #23945, .T. ) ;
#39806 = ORIENTED_EDGE ( 'NONE', *, *, #24479, .T. ) ;
#39807 = CARTESIAN_POINT ( 'NONE',  ( -16.29351483940556733, 0.000000000000000000, 8.217601910042732882 ) ) ;
#39808 = ORIENTED_EDGE ( 'NONE', *, *, #35008, .T. ) ;
#39809 = FACE_OUTER_BOUND ( 'NONE', #14346, .T. ) ;
#39810 = CARTESIAN_POINT ( 'NONE',  ( -27.06552663992790997, 0.000000000000000000, 7.195101427592543786 ) ) ;
#39811 = CARTESIAN_POINT ( 'NONE',  ( -14.13453828727398864, 2.229229656569006401, 2.101142315865724974 ) ) ;
#39812 = ORIENTED_EDGE ( 'NONE', *, *, #3395, .F. ) ;
#39813 = CARTESIAN_POINT ( 'NONE',  ( -12.07154601876183975, 0.000000000000000000, 3.079809270346117067 ) ) ;
#39814 = PLANE ( 'NONE',  #24674 ) ;
#39815 = CARTESIAN_POINT ( 'NONE',  ( -15.91580559589089461, -1.813211359398159583, 3.005709578090212997 ) ) ;
#39816 = LINE ( 'NONE', #1472, #26828 ) ;
#39817 = DIRECTION ( 'NONE',  ( 0.007781995580012662783, 0.000000000000000000, -0.9999697198139514409 ) ) ;
#39818 = CARTESIAN_POINT ( 'NONE',  ( -12.10316060731994803, 0.000000000000000000, 7.142216006181524968 ) ) ;
#39819 = ORIENTED_EDGE ( 'NONE', *, *, #43530, .F. ) ;
#39820 = CARTESIAN_POINT ( 'NONE',  ( -16.18264749718321838, 0.7721120973665051013, 4.434378462272783317 ) ) ;
#39821 = CARTESIAN_POINT ( 'NONE',  ( -20.54204810873173415, 0.000000000000000000, 4.860550213503115558 ) ) ;
#39822 = CARTESIAN_POINT ( 'NONE',  ( -25.20123094555300369, 0.000000000000000000, 6.470945668149052032 ) ) ;
#39823 = ORIENTED_EDGE ( 'NONE', *, *, #14750, .T. ) ;
#39824 = FACE_OUTER_BOUND ( 'NONE', #37703, .T. ) ;
#39825 = CARTESIAN_POINT ( 'NONE',  ( -13.12877911992022995, -0.1191753592594185784, 6.664899307848342502 ) ) ;
#39826 = ORIENTED_EDGE ( 'NONE', *, *, #29109, .F. ) ;
#39827 = ADVANCED_FACE ( 'NONE', ( #42893 ), #46298, .T. ) ;
#39828 = DIRECTION ( 'NONE',  ( 0.005002170337468016433, -0.7660444431189770143, -0.6427681459581293666 ) ) ;
#39829 = CARTESIAN_POINT ( 'NONE',  ( 2.072287782118878319, 0.000000000000000000, -2.950529333540147015 ) ) ;
#39830 = EDGE_CURVE ( 'NONE', #50554, #2552, #46895, .T. ) ;
#39831 = ADVANCED_FACE ( 'NONE', ( #23001 ), #26696, .F. ) ;
#39832 = DIRECTION ( 'NONE',  ( -0.6246952433987893460, -0.7422098413412802076, 0.2426528472758542054 ) ) ;
#39833 = LINE ( 'NONE', #40101, #9338 ) ;
#39834 = ORIENTED_EDGE ( 'NONE', *, *, #1060, .T. ) ;
#39835 = ORIENTED_EDGE ( 'NONE', *, *, #12248, .F. ) ;
#39836 = DIRECTION ( 'NONE',  ( 0.005002170337468016433, -0.7660444431189770143, -0.6427681459581293666 ) ) ;
#39837 = CARTESIAN_POINT ( 'NONE',  ( -18.01733923308073670, 4.010151117816509903, 10.46120871789824847 ) ) ;
#39838 = CARTESIAN_POINT ( 'NONE',  ( -23.52058925276516632, 18.95428125501370076, -4.498258577543088776 ) ) ;
#39839 = CARTESIAN_POINT ( 'NONE',  ( -30.79567442779373110, 0.000000000000000000, 8.843406890442315316 ) ) ;
#39840 = VECTOR ( 'NONE', #3138, 999.9999999999998863 ) ;
#39841 = CARTESIAN_POINT ( 'NONE',  ( -13.03938975049497984, -2.784623065533158304, 6.316914381194012940 ) ) ;
#39842 = CARTESIAN_POINT ( 'NONE',  ( -16.00587945848501192, 0.000000000000000000, 5.265183796632624258 ) ) ;
#39843 = ORIENTED_EDGE ( 'NONE', *, *, #50814, .T. ) ;
#39844 = CARTESIAN_POINT ( 'NONE',  ( -17.73140113748535285, 0.000000000000000000, 13.85752530597602039 ) ) ;
#39845 = DIRECTION ( 'NONE',  ( -0.005002170337468016433, -0.7660444431189770143, 0.6427681459581293666 ) ) ;
#39846 = ORIENTED_EDGE ( 'NONE', *, *, #44441, .T. ) ;
#39847 = DIRECTION ( 'NONE',  ( 0.005002170337468016433, -0.7660444431189770143, -0.6427681459581293666 ) ) ;
#39848 = CARTESIAN_POINT ( 'NONE',  ( -13.73672976910459909, 0.000000000000000000, 12.22661844811216270 ) ) ;
#39849 = DIRECTION ( 'NONE',  ( 0.9999697198139515519, 0.000000000000000000, 0.007781995580013368816 ) ) ;
#39850 = ORIENTED_EDGE ( 'NONE', *, *, #1561, .F. ) ;
#39851 = CARTESIAN_POINT ( 'NONE',  ( -9.808144436391993182, 0.000000000000000000, 10.77986332834118777 ) ) ;
#39852 = EDGE_LOOP ( 'NONE', ( #53952, #35656, #48512, #50319, #10288, #51345 ) ) ;
#39853 = EDGE_CURVE ( 'NONE', #2673, #8988, #44307, .T. ) ;
#39854 = EDGE_LOOP ( 'NONE', ( #33719, #51881, #55777, #7105 ) ) ;
#39855 = ORIENTED_EDGE ( 'NONE', *, *, #52536, .F. ) ;
#39856 = EDGE_CURVE ( 'NONE', #10112, #54371, #30416, .T. ) ;
#39857 = ORIENTED_EDGE ( 'NONE', *, *, #2728, .F. ) ;
#39858 = CARTESIAN_POINT ( 'NONE',  ( -15.36711509922867869, 0.000000000000000000, 8.594143436836516159 ) ) ;
#39859 = ADVANCED_FACE ( 'NONE', ( #30701 ), #4838, .F. ) ;
#39860 = ORIENTED_EDGE ( 'NONE', *, *, #29786, .T. ) ;
#39861 = CARTESIAN_POINT ( 'NONE',  ( -13.17065887352947762, -0.1191753592594197858, 12.04635770780929427 ) ) ;
#39862 = DIRECTION ( 'NONE',  ( -0.005002170337468016433, -0.7660444431189770143, 0.6427681459581293666 ) ) ;
#39863 = ORIENTED_EDGE ( 'NONE', *, *, #30338, .T. ) ;
#39864 = LINE ( 'NONE', #9787, #12309 ) ;
#39865 = EDGE_CURVE ( 'NONE', #2789, #39305, #9377, .T. ) ;
#39866 = ORIENTED_EDGE ( 'NONE', *, *, #49709, .F. ) ;
#39867 = FACE_OUTER_BOUND ( 'NONE', #31417, .T. ) ;
#39868 = ORIENTED_EDGE ( 'NONE', *, *, #25788, .F. ) ;
#39869 = CARTESIAN_POINT ( 'NONE',  ( -11.77243710274829525, -0.1191753592594197858, 11.50324088822667612 ) ) ;
#39870 = DIRECTION ( 'NONE',  ( 0.007781995580012663651, 0.000000000000000000, -0.9999697198139515519 ) ) ;
#39871 = DIRECTION ( 'NONE',  ( 0.6246952433987893460, 0.7422098413412802076, -0.2426528472758539279 ) ) ;
#39872 = PLANE ( 'NONE',  #18473 ) ;
#39873 = LINE ( 'NONE', #52387, #33251 ) ;
#39874 = CARTESIAN_POINT ( 'NONE',  ( -14.12468155607537845, -1.327505506330655782, 4.347100419592131004 ) ) ;
#39875 = ORIENTED_EDGE ( 'NONE', *, *, #37999, .F. ) ;
#39876 = ORIENTED_EDGE ( 'NONE', *, *, #45, .T. ) ;
#39877 = CARTESIAN_POINT ( 'NONE',  ( -25.54040953336767927, 17.91251352657781482, -4.591766625787645495 ) ) ;
#39878 = CARTESIAN_POINT ( 'NONE',  ( -50.99228148001754590, 2.341865487272625668, -3.000000000000007105 ) ) ;
#39879 = EDGE_CURVE ( 'NONE', #48284, #43429, #40032, .T. ) ;
#39880 = DIRECTION ( 'NONE',  ( 0.7660212471507180654, -0.6427876096865404731, 0.005961354470445141482 ) ) ;
#39881 = DIRECTION ( 'NONE',  ( 0.007781995580012662783, 0.000000000000000000, -0.9999697198139514409 ) ) ;
#39882 = ORIENTED_EDGE ( 'NONE', *, *, #17490, .T. ) ;
#39883 = PLANE ( 'NONE',  #15932 ) ;
#39884 = CARTESIAN_POINT ( 'NONE',  ( -10.96739633006137105, 0.000000000000000000, 1.041735613279166195 ) ) ;
#39885 = ORIENTED_EDGE ( 'NONE', *, *, #37514, .T. ) ;
#39886 = DIRECTION ( 'NONE',  ( 0.007781995580012662783, 0.000000000000000000, -0.9999697198139514409 ) ) ;
#39887 = EDGE_CURVE ( 'NONE', #54373, #21014, #47998, .T. ) ;
#39888 = DIRECTION ( 'NONE',  ( 0.6427681459581294776, -0.7660444431189769032, 0.005002170337467562802 ) ) ;
#39889 = ORIENTED_EDGE ( 'NONE', *, *, #10651, .F. ) ;
#39890 = DIRECTION ( 'NONE',  ( 0.9999697198139515519, 0.000000000000000000, 0.007781995580013368816 ) ) ;
#39891 = DIRECTION ( 'NONE',  ( 0.000000000000000000, -0.000000000000000000, -1.000000000000000000 ) ) ;
#39892 = EDGE_CURVE ( 'NONE', #18488, #1003, #5143, .T. ) ;
#39893 = LINE ( 'NONE', #39640, #53152 ) ;
#39894 = ADVANCED_FACE ( 'NONE', ( #13630 ), #18170, .F. ) ;
#39895 = CARTESIAN_POINT ( 'NONE',  ( -18.30454488918022449, -2.946525016555660237, 8.627788126430976590 ) ) ;
#39896 = DIRECTION ( 'NONE',  ( 0.6427681459581294776, -0.7660444431189769032, 0.005002170337467562802 ) ) ;
#39897 = EDGE_LOOP ( 'NONE', ( #48113, #23713, #14669, #6271 ) ) ;
#39898 = EDGE_LOOP ( 'NONE', ( #6681, #6005, #2348, #6939 ) ) ;
#39899 = CARTESIAN_POINT ( 'NONE',  ( -25.20278734466900517, 0.000000000000000000, 6.670939612111840944 ) ) ;
#39900 = DIRECTION ( 'NONE',  ( 0.005002170337468016433, -0.7660444431189770143, -0.6427681459581293666 ) ) ;
#39901 = CARTESIAN_POINT ( 'NONE',  ( -10.37421533196711465, -0.1191753592594197858, 10.96012406864405975 ) ) ;
#39902 = CARTESIAN_POINT ( 'NONE',  ( -21.47419595591918906, 0.000000000000000000, 5.222628093224860102 ) ) ;
#39903 = DIRECTION ( 'NONE',  ( -0.5449076811759708816, 0.6444004775717707689, 0.5364919789714475140 ) ) ;
#39904 = ORIENTED_EDGE ( 'NONE', *, *, #55792, .F. ) ;
#39905 = CARTESIAN_POINT ( 'NONE',  ( -14.04345045867546915, 24.55028594321348123, -3.695677582892548774 ) ) ;
#39906 = CARTESIAN_POINT ( 'NONE',  ( -17.66862480978112515, 0.000000000000000000, 5.790902011229328572 ) ) ;
#39907 = EDGE_CURVE ( 'NONE', #37913, #27257, #13084, .T. ) ;
#39908 = VECTOR ( 'NONE', #53849, 1000.000000000000227 ) ;
#39909 = CARTESIAN_POINT ( 'NONE',  ( -19.60912206198628027, -0.1191753592594197858, 4.398475361799976113 ) ) ;
#39910 = LINE ( 'NONE', #25734, #16943 ) ;
#39911 = ORIENTED_EDGE ( 'NONE', *, *, #26736, .F. ) ;
#39912 = PLANE ( 'NONE',  #9316 ) ;
#39913 = VERTEX_POINT ( 'NONE', #26152 ) ;
#39914 = DIRECTION ( 'NONE',  ( -0.7660212471507179544, -0.6427876096865405842, -0.005961354470445141482 ) ) ;
#39915 = CARTESIAN_POINT ( 'NONE',  ( -20.54204810873173415, 0.000000000000000000, 4.860550213503115558 ) ) ;
#39916 = ORIENTED_EDGE ( 'NONE', *, *, #6380, .F. ) ;
#39917 = LINE ( 'NONE', #45301, #47150 ) ;
#39918 = EDGE_LOOP ( 'NONE', ( #2540, #598, #6466, #54301 ) ) ;
#39919 = ORIENTED_EDGE ( 'NONE', *, *, #8292, .F. ) ;
#39920 = ORIENTED_EDGE ( 'NONE', *, *, #49014, .T. ) ;
#39921 = DIRECTION ( 'NONE',  ( -0.9999697198139514409, -0.000000000000000000, -0.007781995580013368816 ) ) ;
#39922 = ORIENTED_EDGE ( 'NONE', *, *, #3314, .F. ) ;
#39923 = VERTEX_POINT ( 'NONE', #44020 ) ;
#39924 = CARTESIAN_POINT ( 'NONE',  ( -10.79122436818839148, -0.1191753592594179401, 4.836430350399566258 ) ) ;
#39925 = DIRECTION ( 'NONE',  ( 0.007781995580012663651, 0.000000000000000000, -0.9999697198139515519 ) ) ;
#39926 = ORIENTED_EDGE ( 'NONE', *, *, #17916, .T. ) ;
#39927 = EDGE_LOOP ( 'NONE', ( #50600, #55098, #56047, #3607 ) ) ;
#39928 = LINE ( 'NONE', #43618, #3169 ) ;
#39929 = EDGE_CURVE ( 'NONE', #53080, #28729, #14229, .T. ) ;
#39930 = ORIENTED_EDGE ( 'NONE', *, *, #21574, .T. ) ;
#39931 = ORIENTED_EDGE ( 'NONE', *, *, #5979, .T. ) ;
#39932 = DIRECTION ( 'NONE',  ( 0.000000000000000000, -1.000000000000000000, 0.000000000000000000 ) ) ;
#39933 = FACE_OUTER_BOUND ( 'NONE', #14466, .T. ) ;
#39934 = DIRECTION ( 'NONE',  ( 0.000000000000000000, -0.000000000000000000, -1.000000000000000000 ) ) ;
#39935 = DIRECTION ( 'NONE',  ( -0.005002170337468016433, -0.7660444431189770143, 0.6427681459581293666 ) ) ;
#39936 = ORIENTED_EDGE ( 'NONE', *, *, #24149, .T. ) ;
#39937 = FACE_OUTER_BOUND ( 'NONE', #48580, .T. ) ;
#39938 = ORIENTED_EDGE ( 'NONE', *, *, #23705, .F. ) ;
#39939 = EDGE_CURVE ( 'NONE', #39023, #43550, #18453, .T. ) ;
#39940 = FACE_OUTER_BOUND ( 'NONE', #39987, .T. ) ;
#39941 = ADVANCED_FACE ( 'NONE', ( #39189 ), #43460, .F. ) ;
#39942 = EDGE_CURVE ( 'NONE', #34091, #10496, #44564, .T. ) ;
#39943 = VECTOR ( 'NONE', #17320, 1000.000000000000227 ) ;
#39944 = DIRECTION ( 'NONE',  ( 0.7660212471507180654, -0.6427876096865404731, 0.005961354470445141482 ) ) ;
#39945 = PLANE ( 'NONE',  #14112 ) ;
#39946 = CARTESIAN_POINT ( 'NONE',  ( 4.848100717410752658, 0.000000000000000000, 2.061810099490657411 ) ) ;
#39947 = DIRECTION ( 'NONE',  ( 0.007781995580012663651, -3.146120232559066537E-19, -0.9999697198139514409 ) ) ;
#39948 = DIRECTION ( 'NONE',  ( 0.000000000000000000, -0.000000000000000000, -1.000000000000000000 ) ) ;
#39949 = CARTESIAN_POINT ( 'NONE',  ( -1.450993146028691116, -7.184208846019964234, 3.781988589515998367 ) ) ;
#39950 = ORIENTED_EDGE ( 'NONE', *, *, #4425, .F. ) ;
#39951 = FACE_OUTER_BOUND ( 'NONE', #54558, .T. ) ;
#39952 = ADVANCED_FACE ( 'NONE', ( #51970 ), #31542, .F. ) ;
#39953 = DIRECTION ( 'NONE',  ( -0.005002170337468016433, -0.7660444431189770143, 0.6427681459581293666 ) ) ;
#39954 = DIRECTION ( 'NONE',  ( 0.005961354470445682716, -0.6427876096865404731, -0.7660212471507180654 ) ) ;
#39955 = EDGE_CURVE ( 'NONE', #42246, #23133, #18109, .T. ) ;
#39956 = CARTESIAN_POINT ( 'NONE',  ( -17.76652592781524120, -0.1191753592594196748, 5.520811080394955717 ) ) ;
#39957 = CARTESIAN_POINT ( 'NONE',  ( -29.57595708578221050, 13.85053825329486976, -4.768235699741624423 ) ) ;
#39958 = DIRECTION ( 'NONE',  ( -0.005961354470445682716, -0.6427876096865404731, 0.7660212471507180654 ) ) ;
#39959 = ADVANCED_FACE ( 'NONE', ( #17622 ), #34959, .F. ) ;
#39960 = DIRECTION ( 'NONE',  ( 0.007781995580012662783, 0.000000000000000000, -0.9999697198139514409 ) ) ;
#39961 = CARTESIAN_POINT ( 'NONE',  ( -13.53673582514181106, 0.000000000000000000, 12.22817484722816772 ) ) ;
#39962 = EDGE_LOOP ( 'NONE', ( #3152, #3376, #39239, #48208 ) ) ;
#39963 = PLANE ( 'NONE',  #37484 ) ;
#39964 = CARTESIAN_POINT ( 'NONE',  ( -14.29695817873406405, 0.000000000000000000, 8.771797659027555483 ) ) ;
#39965 = CARTESIAN_POINT ( 'NONE',  ( -1.086233639165236964, 0.000000000000000000, -2.796443541562362078 ) ) ;
#39966 = EDGE_CURVE ( 'NONE', #7042, #44931, #11040, .T. ) ;
#39967 = FACE_OUTER_BOUND ( 'NONE', #21086, .T. ) ;
#39968 = LINE ( 'NONE', #35433, #52087 ) ;
#39969 = LINE ( 'NONE', #26631, #45098 ) ;
#39970 = CARTESIAN_POINT ( 'NONE',  ( -16.02731548741127199, 0.000000000000000000, 8.019667478731950183 ) ) ;
#39971 = EDGE_CURVE ( 'NONE', #30096, #20287, #36921, .T. ) ;
#39972 = PLANE ( 'NONE',  #600 ) ;
#39973 = PLANE ( 'NONE',  #11095 ) ;
#39974 = VERTEX_POINT ( 'NONE', #32907 ) ;
#39975 = AXIS2_PLACEMENT_3D ( 'NONE', #40364, #6023, #52845 ) ;
#39976 = VECTOR ( 'NONE', #50217, 1000.000000000000227 ) ;
#39977 = ORIENTED_EDGE ( 'NONE', *, *, #54021, .F. ) ;
#39978 = VERTEX_POINT ( 'NONE', #28098 ) ;
#39979 = VERTEX_POINT ( 'NONE', #27845 ) ;
#39980 = ORIENTED_EDGE ( 'NONE', *, *, #14640, .F. ) ;
#39981 = CARTESIAN_POINT ( 'NONE',  ( -16.46033779569424382, 0.000000000000000000, 3.953644831128531489 ) ) ;
#39982 = CARTESIAN_POINT ( 'NONE',  ( -11.67244013076689946, 0.000000000000000000, 11.50401908778467863 ) ) ;
#39983 = ORIENTED_EDGE ( 'NONE', *, *, #31623, .T. ) ;
#39984 = ORIENTED_EDGE ( 'NONE', *, *, #4608, .F. ) ;
#39985 = EDGE_CURVE ( 'NONE', #25477, #693, #11334, .T. ) ;
#39986 = CARTESIAN_POINT ( 'NONE',  ( 2.072287782118878319, 0.000000000000000000, -2.950529333540147015 ) ) ;
#39987 = EDGE_LOOP ( 'NONE', ( #8179, #5369, #16178, #34391 ) ) ;
#39988 = CARTESIAN_POINT ( 'NONE',  ( -13.27065584551087163, 0.000000000000000000, 12.04557950825129176 ) ) ;
#39989 = CARTESIAN_POINT ( 'NONE',  ( -26.13337879274045505, 0.000000000000000000, 6.833023547870798353 ) ) ;
#39990 = ORIENTED_EDGE ( 'NONE', *, *, #16361, .T. ) ;
#39991 = DIRECTION ( 'NONE',  ( 0.9999697198139515519, 0.000000000000000000, 0.007781995580013368816 ) ) ;
#39992 = EDGE_CURVE ( 'NONE', #14652, #35264, #2532, .T. ) ;
#39993 = EDGE_CURVE ( 'NONE', #21352, #31229, #14759, .T. ) ;
#39994 = VERTEX_POINT ( 'NONE', #45987 ) ;
#39995 = VECTOR ( 'NONE', #18450, 1000.000000000000227 ) ;
#39996 = AXIS2_PLACEMENT_3D ( 'NONE', #23327, #37195, #25532 ) ;
#39997 = DIRECTION ( 'NONE',  ( -0.9999697198139514409, -0.000000000000000000, -0.007781995580013368816 ) ) ;
#39998 = FACE_OUTER_BOUND ( 'NONE', #42301, .T. ) ;
#39999 = EDGE_CURVE ( 'NONE', #3951, #42842, #7094, .T. ) ;
#40000 = DIRECTION ( 'NONE',  ( 0.007781995580012663651, -3.146120232559066537E-19, -0.9999697198139514409 ) ) ;
#40001 = CARTESIAN_POINT ( 'NONE',  ( -10.34383179237899775, -0.1191753592594181482, 7.055904481714163623 ) ) ;
#40002 = EDGE_LOOP ( 'NONE', ( #45475, #3028, #1861 ) ) ;
#40003 = CARTESIAN_POINT ( 'NONE',  ( -13.21230997042793120, 0.000000000000000000, 4.548259860725153203 ) ) ;
#40004 = FACE_OUTER_BOUND ( 'NONE', #15819, .T. ) ;
#40005 = LINE ( 'NONE', #48537, #1283 ) ;
#40006 = ORIENTED_EDGE ( 'NONE', *, *, #41651, .F. ) ;
#40007 = CARTESIAN_POINT ( 'NONE',  ( -13.76383987162373579, 0.000000000000000000, 2.127969252444404713 ) ) ;
#40008 = ORIENTED_EDGE ( 'NONE', *, *, #36826, .T. ) ;
#40009 = DIRECTION ( 'NONE',  ( -0.005961354470445682716, -0.6427876096865404731, 0.7660212471507180654 ) ) ;
#40010 = DIRECTION ( 'NONE',  ( 0.9999697198139515519, 0.000000000000000000, 0.007781995580013368816 ) ) ;
#40011 = CARTESIAN_POINT ( 'NONE',  ( -8.975993561185934055, -0.1191753592594197858, 10.41700724906143982 ) ) ;
#40012 = EDGE_CURVE ( 'NONE', #21780, #41291, #40621, .T. ) ;
#40013 = PLANE ( 'NONE',  #47705 ) ;
#40014 = LINE ( 'NONE', #14472, #54062 ) ;
#40015 = FACE_OUTER_BOUND ( 'NONE', #1894, .T. ) ;
#40016 = CARTESIAN_POINT ( 'NONE',  ( -32.65841372305263235, 0.000000000000000000, 9.367568705923016381 ) ) ;
#40017 = VECTOR ( 'NONE', #8507, 1000.000000000000000 ) ;
#40018 = EDGE_CURVE ( 'NONE', #40865, #5570, #5981, .T. ) ;
#40019 = DIRECTION ( 'NONE',  ( 0.9999697198139515519, 0.000000000000000000, 0.007781995580013368816 ) ) ;
#40020 =( LENGTH_UNIT ( ) NAMED_UNIT ( * ) SI_UNIT ( .MILLI., .METRE. ) );
#40021 = EDGE_CURVE ( 'NONE', #54304, #21718, #54220, .T. ) ;
#40022 = LINE ( 'NONE', #35485, #30526 ) ;
#40023 = ORIENTED_EDGE ( 'NONE', *, *, #52903, .T. ) ;
#40024 = DIRECTION ( 'NONE',  ( 0.005961354470445682716, -0.6427876096865404731, -0.7660212471507180654 ) ) ;
#40025 = DIRECTION ( 'NONE',  ( -0.005002170337468016433, -0.7660444431189770143, 0.6427681459581293666 ) ) ;
#40026 = LINE ( 'NONE', #43201, #52661 ) ;
#40027 = B_SPLINE_CURVE_WITH_KNOTS ( 'NONE', 3,
 ( #31476, #1050, #9299, #39422 ),
 .UNSPECIFIED., .F., .F.,
 ( 4, 4 ),
 ( 0.000000000000000000, 0.0003329496823836150814 ),
 .UNSPECIFIED. ) ;
#40028 = LINE ( 'NONE', #6251, #31285 ) ;
#40029 = ADVANCED_FACE ( 'NONE', ( #23825 ), #37172, .F. ) ;
#40030 = LINE ( 'NONE', #5141, #19161 ) ;
#40031 = DIRECTION ( 'NONE',  ( -0.005002170337468016433, -0.7660444431189770143, 0.6427681459581293666 ) ) ;
#40032 = LINE ( 'NONE', #17920, #42859 ) ;
#40033 = ORIENTED_EDGE ( 'NONE', *, *, #4878, .F. ) ;
#40034 = ORIENTED_EDGE ( 'NONE', *, *, #47239, .T. ) ;
#40035 = CARTESIAN_POINT ( 'NONE',  ( -21.36715069126009325, 4.657758921906509642, 12.82522398413292741 ) ) ;
#40036 = PRODUCT_DEFINITION_SHAPE ( 'NONE', 'NONE',  #56240 ) ;
#40037 = CARTESIAN_POINT ( 'NONE',  ( -16.38985955832367836, -0.1191753592594190225, 7.747517035245570227 ) ) ;
#40038 = VECTOR ( 'NONE', #34806, 1000.000000000000114 ) ;
#40039 = VECTOR ( 'NONE', #16131, 1000.000000000000227 ) ;
#40040 = ORIENTED_EDGE ( 'NONE', *, *, #39999, .T. ) ;
#40041 = CARTESIAN_POINT ( 'NONE',  ( -11.77243710274829525, -0.1191753592594197858, 11.50324088822667612 ) ) ;
#40042 = VERTEX_POINT ( 'NONE', #18764 ) ;
#40043 = LINE ( 'NONE', #17339, #55596 ) ;
#40044 = ORIENTED_EDGE ( 'NONE', *, *, #6299, .T. ) ;
#40045 = EDGE_LOOP ( 'NONE', ( #8512, #11705, #52368, #37980 ) ) ;
#40046 = AXIS2_PLACEMENT_3D ( 'NONE', #33581, #15420, #2368 ) ;
#40047 = VERTEX_POINT ( 'NONE', #53391 ) ;
#40048 = CARTESIAN_POINT ( 'NONE',  ( -6.110905869600904872, 1.712176620043476140E-14, -4.599999999999999645 ) ) ;
#40049 = FACE_OUTER_BOUND ( 'NONE', #42757, .T. ) ;
#40050 = CARTESIAN_POINT ( 'NONE',  ( -57.52614991588065152, -8.291364278369167451, 5.150256511358686722E-15 ) ) ;
#40051 = EDGE_CURVE ( 'NONE', #35922, #21974, #36087, .T. ) ;
#40052 = CARTESIAN_POINT ( 'NONE',  ( -15.60102546347950536, 0.000000000000000000, 12.95077420755565356 ) ) ;
#40053 = EDGE_LOOP ( 'NONE', ( #34459, #34339, #39435, #37064 ) ) ;
#40055 = ORIENTED_EDGE ( 'NONE', *, *, #36503, .F. ) ;
#40054 = EDGE_CURVE ( 'NONE', #14368, #873, #15320, .T. ) ;
#40056 = VECTOR ( 'NONE', #18015, 999.9999999999998863 ) ;
#40057 = CARTESIAN_POINT ( 'NONE',  ( -24.26908309836554878, 0.000000000000000000, 6.108867788427308376 ) ) ;
#40058 = ORIENTED_EDGE ( 'NONE', *, *, #49364, .T. ) ;
#40059 = FACE_OUTER_BOUND ( 'NONE', #785, .T. ) ;
#40060 = ORIENTED_EDGE ( 'NONE', *, *, #33425, .T. ) ;
#40061 = LINE ( 'NONE', #44594, #38745 ) ;
#40062 = DIRECTION ( 'NONE',  ( -0.005961354470445682716, -0.6427876096865404731, 0.7660212471507180654 ) ) ;
#40063 = EDGE_CURVE ( 'NONE', #52847, #5849, #44859, .T. ) ;
#40064 = EDGE_CURVE ( 'NONE', #50295, #26566, #32632, .T. ) ;
#40065 = EDGE_CURVE ( 'NONE', #36873, #27011, #45156, .T. ) ;
#40066 = ORIENTED_EDGE ( 'NONE', *, *, #35845, .T. ) ;
#40067 = CARTESIAN_POINT ( 'NONE',  ( -25.20278734466900517, 0.000000000000000000, 6.670939612111840944 ) ) ;
#40068 = ORIENTED_EDGE ( 'NONE', *, *, #19041, .T. ) ;
#40069 = ADVANCED_FACE ( 'NONE', ( #23560 ), #40875, .F. ) ;
#40070 = PLANE ( 'NONE',  #17302 ) ;
#40071 = ORIENTED_EDGE ( 'NONE', *, *, #36623, .F. ) ;
#40072 = DIRECTION ( 'NONE',  ( 0.9999697198139515519, 0.000000000000000000, 0.007781995580013368816 ) ) ;
#40073 = CARTESIAN_POINT ( 'NONE',  ( -13.57329764222433788, -0.1191753592594185784, 4.076115473275981671 ) ) ;
#40074 = LINE ( 'NONE', #40912, #16520 ) ;
#40075 = VERTEX_POINT ( 'NONE', #53933 ) ;
#40076 = VECTOR ( 'NONE', #28674, 1000.000000000000114 ) ;
#40077 = AXIS2_PLACEMENT_3D ( 'NONE', #45442, #1729, #41197 ) ;
#40078 = LINE ( 'NONE', #23342, #33757 ) ;
#40079 = CARTESIAN_POINT ( 'NONE',  ( -22.40478740399063895, 0.000000000000000000, 5.384712028983816623 ) ) ;
#40080 = CARTESIAN_POINT ( 'NONE',  ( -26.13337879274045505, 0.000000000000000000, 6.833023547870798353 ) ) ;
#40081 = CARTESIAN_POINT ( 'NONE',  ( -15.60102546347950536, 0.000000000000000000, 12.95077420755565356 ) ) ;
#40083 = EDGE_CURVE ( 'NONE', #10299, #530, #15054, .T. ) ;
#40082 = DIRECTION ( 'NONE',  ( 0.9999697198139515519, 0.000000000000000000, 0.007781995580013368816 ) ) ;
#40084 = ADVANCED_FACE ( 'NONE', ( #7341 ), #33215, .F. ) ;
#40085 = LINE ( 'NONE', #41208, #1361 ) ;
#40086 = AXIS2_PLACEMENT_3D ( 'NONE', #25930, #34173, #43256 ) ;
#40087 = ORIENTED_EDGE ( 'NONE', *, *, #29960, .F. ) ;
#40088 = FACE_OUTER_BOUND ( 'NONE', #26878, .T. ) ;
#40089 = LINE ( 'NONE', #20477, #54881 ) ;
#40090 = EDGE_CURVE ( 'NONE', #10456, #25250, #42284, .T. ) ;
#40091 = PLANE ( 'NONE',  #51390 ) ;
#40092 = ORIENTED_EDGE ( 'NONE', *, *, #46429, .F. ) ;
#40093 = PLANE ( 'NONE',  #9364 ) ;
#40094 = CARTESIAN_POINT ( 'NONE',  ( -17.43575422274359710, -4.727446477803164626, 3.503129884459415422 ) ) ;
#40095 = VERTEX_POINT ( 'NONE', #3645 ) ;
#40096 = CARTESIAN_POINT ( 'NONE',  ( -17.46532115785441519, 0.000000000000000000, 13.67492996699914265 ) ) ;
#40097 = EDGE_CURVE ( 'NONE', #41167, #44596, #24656, .T. ) ;
#40098 = PLANE ( 'NONE',  #55646 ) ;
#40099 = CARTESIAN_POINT ( 'NONE',  ( -16.03018954091655601, 0.000000000000000000, 8.388977181989714538 ) ) ;
#40100 = EDGE_CURVE ( 'NONE', #20518, #36569, #29507, .T. ) ;
#40101 = CARTESIAN_POINT ( 'NONE',  ( -18.76964031537362487, -1.327505506330657781, 4.129732459434496405 ) ) ;
#40102 = VERTEX_POINT ( 'NONE', #47363 ) ;
#40103 = ORIENTED_EDGE ( 'NONE', *, *, #26257, .F. ) ;
#40104 = FACE_OUTER_BOUND ( 'NONE', #51936, .T. ) ;
#40105 = CARTESIAN_POINT ( 'NONE',  ( -27.99767448711536133, 0.000000000000000000, 7.557179307314289218 ) ) ;
#40106 = LINE ( 'NONE', #917, #8768 ) ;
#40107 = PLANE ( 'NONE',  #12095 ) ;
#40108 = LINE ( 'NONE', #27622, #21959 ) ;
#40109 = PLANE ( 'NONE',  #33079 ) ;
#40110 = VECTOR ( 'NONE', #6125, 1000.000000000000114 ) ;
#40111 = VERTEX_POINT ( 'NONE', #24389 ) ;
#40112 = CARTESIAN_POINT ( 'NONE',  ( -16.92784874604061329, 0.000000000000000000, 4.319338622618287715 ) ) ;
#40113 = DIRECTION ( 'NONE',  ( -0.005002170337468016433, -0.7660444431189770143, 0.6427681459581293666 ) ) ;
#40114 = ORIENTED_EDGE ( 'NONE', *, *, #48779, .F. ) ;
#40115 = CARTESIAN_POINT ( 'NONE',  ( -17.74560456716937296, 0.000000000000000000, 3.774316574337878372 ) ) ;
#40116 = AXIS2_PLACEMENT_3D ( 'NONE', #54355, #36780, #36220 ) ;
#40117 = CARTESIAN_POINT ( 'NONE',  ( -18.66354898467281132, 0.000000000000000000, 14.21960318569776582 ) ) ;
#40118 = CARTESIAN_POINT ( 'NONE',  ( -25.20278734466900517, 0.000000000000000000, 6.670939612111840944 ) ) ;
#40119 = ORIENTED_EDGE ( 'NONE', *, *, #23716, .T. ) ;
#40120 = VECTOR ( 'NONE', #2784, 1000.000000000000114 ) ;
#40121 = VECTOR ( 'NONE', #39168, 1000.000000000000114 ) ;
#40122 = DIRECTION ( 'NONE',  ( -0.9999697198139514409, -0.000000000000000000, -0.007781995580013368816 ) ) ;
#40123 = ORIENTED_EDGE ( 'NONE', *, *, #849, .F. ) ;
#40124 = ORIENTED_EDGE ( 'NONE', *, *, #213, .F. ) ;
#40125 = VECTOR ( 'NONE', #41908, 999.9999999999998863 ) ;
#40126 = ORIENTED_EDGE ( 'NONE', *, *, #33406, .T. ) ;
#40127 = VECTOR ( 'NONE', #19493, 1000.000000000000227 ) ;
#40128 = EDGE_LOOP ( 'NONE', ( #13732, #30107, #13408, #20211, #27599 ) ) ;
#40129 = DIRECTION ( 'NONE',  ( -0.005002170337468016433, -0.7660444431189770143, 0.6427681459581293666 ) ) ;
#40130 = ORIENTED_EDGE ( 'NONE', *, *, #18158, .T. ) ;
#40131 = LINE ( 'NONE', #26805, #43082 ) ;
#40132 = PLANE ( 'NONE',  #31333 ) ;
#40133 = EDGE_CURVE ( 'NONE', #52910, #55300, #20110, .T. ) ;
#40134 = ORIENTED_EDGE ( 'NONE', *, *, #1140, .T. ) ;
#40135 = DIRECTION ( 'NONE',  ( 0.7660212471507180654, -0.6427876096865404731, 0.005961354470445141482 ) ) ;
#40136 = ORIENTED_EDGE ( 'NONE', *, *, #4275, .F. ) ;
#40138 = MECHANICAL_DESIGN_GEOMETRIC_PRESENTATION_REPRESENTATION (  '', ( #25623 ), #41028 ) ;
#40137 = PLANE ( 'NONE',  #11374 ) ;
#40139 = VERTEX_POINT ( 'NONE', #46827 ) ;
#40140 = EDGE_CURVE ( 'NONE', #5645, #5914, #28942, .T. ) ;
#40141 = ADVANCED_FACE ( 'NONE', ( #41977 ), #37442, .F. ) ;
#40142 = CARTESIAN_POINT ( 'NONE',  ( -13.08330893211609869, 0.000000000000000000, 1.763933231766363630 ) ) ;
#40143 = LINE ( 'NONE', #23400, #2111 ) ;
#40144 = LINE ( 'NONE', #14034, #45000 ) ;
#40145 = CARTESIAN_POINT ( 'NONE',  ( -16.25746979822617178, 0.000000000000000000, 3.585891526986769051 ) ) ;
#40146 = LINE ( 'NONE', #30540, #40516 ) ;
#40147 = CARTESIAN_POINT ( 'NONE',  ( -27.06552663992790997, 0.000000000000000000, 7.195101427592543786 ) ) ;
#40148 = ORIENTED_EDGE ( 'NONE', *, *, #19223, .F. ) ;
#40149 = ORIENTED_EDGE ( 'NONE', *, *, #35008, .F. ) ;
#40150 = DIRECTION ( 'NONE',  ( 0.007781995580012663651, 0.000000000000000000, -0.9999697198139515519 ) ) ;
#40151 = CARTESIAN_POINT ( 'NONE',  ( -12.80458192191714595, 0.000000000000000000, 11.86454056839041726 ) ) ;
#40152 = VECTOR ( 'NONE', #6315, 1000.000000000000114 ) ;
#40153 = FACE_OUTER_BOUND ( 'NONE', #9261, .T. ) ;
#40154 = CARTESIAN_POINT ( 'NONE',  ( -15.03495456790438389, -0.1191753592594197858, 12.77051346725278158 ) ) ;
#40155 = ORIENTED_EDGE ( 'NONE', *, *, #53531, .F. ) ;
#40156 = LINE ( 'NONE', #48964, #3154 ) ;
#40157 = FACE_OUTER_BOUND ( 'NONE', #20422, .T. ) ;
#40158 = ORIENTED_EDGE ( 'NONE', *, *, #5733, .F. ) ;
#40160 = FACE_OUTER_BOUND ( 'NONE', #24390, .T. ) ;
#40159 = VECTOR ( 'NONE', #23569, 1000.000000000000114 ) ;
#40161 = DIRECTION ( 'NONE',  ( -0.5449076811759708816, 0.6444004775717707689, 0.5364919789714475140 ) ) ;
#40162 = ORIENTED_EDGE ( 'NONE', *, *, #24753, .F. ) ;
#40163 = VECTOR ( 'NONE', #19260, 1000.000000000000227 ) ;
#40164 = AXIS2_PLACEMENT_3D ( 'NONE', #30872, #35418, #40236 ) ;
#40165 = LINE ( 'NONE', #14606, #7103 ) ;
#40166 = LINE ( 'NONE', #1258, #54156 ) ;
#40167 = FACE_OUTER_BOUND ( 'NONE', #21990, .T. ) ;
#40168 = EDGE_CURVE ( 'NONE', #7643, #9219, #7632, .T. ) ;
#40169 = PLANE ( 'NONE',  #45929 ) ;
#40170 = DIRECTION ( 'NONE',  ( 0.7660212471507180654, -0.6427876096865404731, 0.005961354470445141482 ) ) ;
#40171 = ORIENTED_EDGE ( 'NONE', *, *, #51796, .T. ) ;
#40172 = VECTOR ( 'NONE', #49269, 999.9999999999998863 ) ;
#40173 = VECTOR ( 'NONE', #38726, 1000.000000000000227 ) ;
#40174 = EDGE_CURVE ( 'NONE', #13341, #13570, #17012, .T. ) ;
#40175 = ORIENTED_EDGE ( 'NONE', *, *, #20859, .F. ) ;
#40176 = DIRECTION ( 'NONE',  ( -0.5449076811759708816, 0.6444004775717707689, 0.5364919789714475140 ) ) ;
#40177 = DIRECTION ( 'NONE',  ( 0.9031405107545329436, 0.1035669190568594411, -0.4166666666666669072 ) ) ;
#40178 = DIRECTION ( 'NONE',  ( 0.9999697198139515519, 0.000000000000000000, 0.007781995580013368816 ) ) ;
#40179 = CARTESIAN_POINT ( 'NONE',  ( -11.67244013076689946, 0.000000000000000000, 11.50401908778467863 ) ) ;
#40180 = EDGE_CURVE ( 'NONE', #33398, #54798, #42556, .T. ) ;
#40181 = AXIS2_PLACEMENT_3D ( 'NONE', #8758, #7602, #3050 ) ;
#40182 = CARTESIAN_POINT ( 'NONE',  ( -13.33648223891196949, 0.000000000000000000, 1.961969034772858667 ) ) ;
#40183 = ORIENTED_EDGE ( 'NONE', *, *, #6616, .F. ) ;
#40185 = VECTOR ( 'NONE', #15222, 999.9999999999998863 ) ;
#40184 = DIRECTION ( 'NONE',  ( -0.6427681459581293666, -0.7660444431189770143, -0.005002170337467561935 ) ) ;
#40186 = CARTESIAN_POINT ( 'NONE',  ( -15.81163362153278129, 0.000000000000000000, 6.005359602264157104 ) ) ;
#40187 = LINE ( 'NONE', #47597, #54992 ) ;
#40188 = DIRECTION ( 'NONE',  ( 0.9999697198139515519, 0.000000000000000000, 0.007781995580013368816 ) ) ;
#40189 = ORIENTED_EDGE ( 'NONE', *, *, #29248, .T. ) ;
#40190 = CARTESIAN_POINT ( 'NONE',  ( -18.68049516737052329, 3.200641362704010007, 3.835953230116354362 ) ) ;
#40191 = ORIENTED_EDGE ( 'NONE', *, *, #18264, .T. ) ;
#40192 = CARTESIAN_POINT ( 'NONE',  ( -22.40634380310664397, 0.000000000000000000, 5.584705972946605534 ) ) ;
#40193 = VECTOR ( 'NONE', #50625, 1000.000000000000227 ) ;
#40194 = DIRECTION ( 'NONE',  ( 0.005961354470445682716, -0.6427876096865404731, -0.7660212471507180654 ) ) ;
#40195 = EDGE_LOOP ( 'NONE', ( #14171, #14494, #30068, #26210 ) ) ;
#40196 = FACE_OUTER_BOUND ( 'NONE', #4901, .T. ) ;
#40197 = VECTOR ( 'NONE', #13995, 999.9999999999998863 ) ;
#40198 = VERTEX_POINT ( 'NONE', #37752 ) ;
#40199 = ORIENTED_EDGE ( 'NONE', *, *, #47261, .T. ) ;
#40200 = ORIENTED_EDGE ( 'NONE', *, *, #41551, .T. ) ;
#40201 = DIRECTION ( 'NONE',  ( -0.005961354470445682716, -0.6427876096865404731, 0.7660212471507180654 ) ) ;
#40202 = ORIENTED_EDGE ( 'NONE', *, *, #15372, .F. ) ;
#40203 = ORIENTED_EDGE ( 'NONE', *, *, #36806, .F. ) ;
#40204 = VECTOR ( 'NONE', #23092, 999.9999999999998863 ) ;
#40205 = DIRECTION ( 'NONE',  ( -0.000000000000000000, -0.000000000000000000, 1.000000000000000000 ) ) ;
#40206 = ADVANCED_FACE ( 'NONE', ( #47093 ), #16157, .F. ) ;
#40207 = LINE ( 'NONE', #18638, #44864 ) ;
#40208 = ORIENTED_EDGE ( 'NONE', *, *, #37234, .T. ) ;
#40209 = AXIS2_PLACEMENT_3D ( 'NONE', #3748, #12296, #51479 ) ;
#40210 = AXIS2_PLACEMENT_3D ( 'NONE', #21735, #33654, #34790 ) ;
#40211 = EDGE_CURVE ( 'NONE', #485, #51780, #34046, .T. ) ;
#40212 = VERTEX_POINT ( 'NONE', #55910 ) ;
#40213 = CARTESIAN_POINT ( 'NONE',  ( -19.47419960943008732, -2.577107522633557135, 7.507661911811399413 ) ) ;
#40214 = VERTEX_POINT ( 'NONE', #50783 ) ;
#40215 = ORIENTED_EDGE ( 'NONE', *, *, #54259, .T. ) ;
#40216 = ADVANCED_FACE ( 'NONE', ( #11876 ), #55325, .F. ) ;
#40217 = EDGE_CURVE ( 'NONE', #17834, #13134, #37996, .T. ) ;
#40218 = VECTOR ( 'NONE', #46607, 1000.000000000000114 ) ;
#40219 = VECTOR ( 'NONE', #9884, 1000.000000000000000 ) ;
#40220 = LINE ( 'NONE', #23195, #17487 ) ;
#40221 = PLANE ( 'NONE',  #14002 ) ;
#40222 = LINE ( 'NONE', #18653, #37745 ) ;
#40223 = LINE ( 'NONE', #18348, #39535 ) ;
#40224 = ORIENTED_EDGE ( 'NONE', *, *, #41453, .F. ) ;
#40225 = LINE ( 'NONE', #45065, #2015 ) ;
#40226 = ORIENTED_EDGE ( 'NONE', *, *, #7305, .F. ) ;
#40227 = FACE_OUTER_BOUND ( 'NONE', #25762, .T. ) ;
#40228 = EDGE_CURVE ( 'NONE', #49004, #33246, #19279, .T. ) ;
#40229 = CARTESIAN_POINT ( 'NONE',  ( 0.1285714285714296967, 2.000000000000000000, -5.998622290806041590 ) ) ;
#40230 = CARTESIAN_POINT ( 'NONE',  ( -14.66887761629205222, 0.000000000000000000, 12.58869632783390990 ) ) ;
#40231 = LINE ( 'NONE', #17528, #20366 ) ;
#40232 = VECTOR ( 'NONE', #17164, 1000.000000000000227 ) ;
#40233 = DIRECTION ( 'NONE',  ( 0.5364919789714477361, 0.6444004775717706579, 0.5449076811759711036 ) ) ;
#40234 = DIRECTION ( 'NONE',  ( 0.6246952433987894571, -0.7422098413412800966, -0.2426528472758541777 ) ) ;
#40235 = ORIENTED_EDGE ( 'NONE', *, *, #43536, .T. ) ;
#40236 = DIRECTION ( 'NONE',  ( -0.6427681459581293666, -0.7660444431189770143, -0.005002170337467561935 ) ) ;
#40237 = VECTOR ( 'NONE', #35757, 999.9999999999998863 ) ;
#40238 = VERTEX_POINT ( 'NONE', #12168 ) ;
#40239 = DIRECTION ( 'NONE',  ( -0.3620778797217457656, 0.000000000000000000, -0.9321478471874539151 ) ) ;
#40240 = DIRECTION ( 'NONE',  ( -0.005002170337468016433, -0.7660444431189770143, 0.6427681459581293666 ) ) ;
#40241 = FACE_OUTER_BOUND ( 'NONE', #22060, .T. ) ;
#40242 = AXIS2_PLACEMENT_3D ( 'NONE', #53318, #36265, #39948 ) ;
#40243 = FACE_OUTER_BOUND ( 'NONE', #19977, .T. ) ;
#40244 = DIRECTION ( 'NONE',  ( 0.000000000000000000, -0.000000000000000000, -1.000000000000000000 ) ) ;
#40245 = CARTESIAN_POINT ( 'NONE',  ( -70.83115287062283016, -1.183819181302419339E-15, -9.798907322976862844 ) ) ;
#40246 = ORIENTED_EDGE ( 'NONE', *, *, #23665, .F. ) ;
#40247 = VECTOR ( 'NONE', #22736, 999.9999999999998863 ) ;
#40248 = DIRECTION ( 'NONE',  ( 0.000000000000000000, -0.000000000000000000, -1.000000000000000000 ) ) ;
#40249 = CARTESIAN_POINT ( 'NONE',  ( -13.08486533123210194, 0.000000000000000000, 1.963927175729152541 ) ) ;
#40250 = DIRECTION ( 'NONE',  ( 0.9999697198139515519, 0.000000000000000000, 0.007781995580013368816 ) ) ;
#40251 = VECTOR ( 'NONE', #19889, 1000.000000000000227 ) ;
#40252 = CARTESIAN_POINT ( 'NONE',  ( -22.40634380310664397, 0.000000000000000000, 5.584705972946605534 ) ) ;
#40253 = EDGE_CURVE ( 'NONE', #10480, #15058, #13846, .T. ) ;
#40254 = PLANE ( 'NONE',  #35758 ) ;
#40255 = LINE ( 'NONE', #1344, #39537 ) ;
#40256 = CARTESIAN_POINT ( 'NONE',  ( -20.67116051404115140, -4.079838673713159558, 11.40702279338511538 ) ) ;
#40257 = AXIS2_PLACEMENT_3D ( 'NONE', #25820, #13796, #7652 ) ;
#40258 = VECTOR ( 'NONE', #34262, 1000.000000000000114 ) ;
#40259 = CARTESIAN_POINT ( 'NONE',  ( -23.23471500290295921, 19.24370688441070953, 4.480778704491060971 ) ) ;
#40260 = DIRECTION ( 'NONE',  ( -0.9999697198139514409, -0.000000000000000000, -0.007781995580013368816 ) ) ;
#40261 = ADVANCED_FACE ( 'NONE', ( #43950 ), #35726, .F. ) ;
#40262 = ORIENTED_EDGE ( 'NONE', *, *, #5016, .T. ) ;
#40263 = EDGE_CURVE ( 'NONE', #30962, #3478, #22098, .T. ) ;
#40264 = EDGE_CURVE ( 'NONE', #43270, #31194, #13020, .T. ) ;
#40265 = ORIENTED_EDGE ( 'NONE', *, *, #3592, .F. ) ;
#40266 = ORIENTED_EDGE ( 'NONE', *, *, #42450, .T. ) ;
#40267 = VERTEX_POINT ( 'NONE', #22402 ) ;
#40268 = AXIS2_PLACEMENT_3D ( 'NONE', #17644, #39519, #44042 ) ;
#40269 = VERTEX_POINT ( 'NONE', #30643 ) ;
#40270 = DIRECTION ( 'NONE',  ( -0.005002170337468016433, -0.7660444431189770143, 0.6427681459581293666 ) ) ;
#40271 = EDGE_CURVE ( 'NONE', #23289, #4032, #35187, .T. ) ;
#40272 = LINE ( 'NONE', #15276, #25821 ) ;
#40273 = VECTOR ( 'NONE', #24023, 1000.000000000000000 ) ;
#40275 = EDGE_CURVE ( 'NONE', #19751, #7777, #793, .T. ) ;
#40274 = ORIENTED_EDGE ( 'NONE', *, *, #54597, .F. ) ;
#40276 = EDGE_LOOP ( 'NONE', ( #29874, #50213, #15004, #2564 ) ) ;
#40277 = ORIENTED_EDGE ( 'NONE', *, *, #5613, .F. ) ;
#40278 = VECTOR ( 'NONE', #37081, 999.9999999999998863 ) ;
#40279 = ADVANCED_FACE ( 'NONE', ( #13578 ), #21813, .F. ) ;
#40280 = CARTESIAN_POINT ( 'NONE',  ( -14.20280369269832832, 0.000000000000000000, 12.40765738797303719 ) ) ;
#40281 = AXIS2_PLACEMENT_3D ( 'NONE', #51990, #13649, #35814 ) ;
#40282 = CARTESIAN_POINT ( 'NONE',  ( -12.06998961964583650, 0.000000000000000000, 2.879815326383328156 ) ) ;
#40283 = DIRECTION ( 'NONE',  ( -0.6427681459581293666, -0.7660444431189770143, -0.005002170337467561935 ) ) ;
#40284 = EDGE_LOOP ( 'NONE', ( #6233, #46759, #26178, #44731 ) ) ;
#40285 = CARTESIAN_POINT ( 'NONE',  ( -10.00813838035478298, 0.000000000000000000, 10.77830692922518452 ) ) ;
#40286 = VECTOR ( 'NONE', #21224, 999.9999999999998863 ) ;
#40287 = EDGE_CURVE ( 'NONE', #53425, #31213, #31483, .T. ) ;
#40288 = ORIENTED_EDGE ( 'NONE', *, *, #36066, .T. ) ;
#40289 = CARTESIAN_POINT ( 'NONE',  ( -10.74029228357944987, 0.000000000000000000, 11.14194120806293320 ) ) ;
#40290 = PLANE ( 'NONE',  #32974 ) ;
#40291 = EDGE_CURVE ( 'NONE', #44163, #40865, #8477, .T. ) ;
#40292 = VECTOR ( 'NONE', #41636, 1000.000000000000114 ) ;
#40293 = DIRECTION ( 'NONE',  ( -0.3620778797217457656, 0.000000000000000000, -0.9321478471874539151 ) ) ;
#40294 = CARTESIAN_POINT ( 'NONE',  ( -16.99924723426068951, 0.000000000000000000, 13.49389102713827171 ) ) ;
#40295 = AXIS2_PLACEMENT_3D ( 'NONE', #48915, #43798, #27321 ) ;
#40296 = DIRECTION ( 'NONE',  ( 0.9999697198139515519, 0.000000000000000000, 0.007781995580013368816 ) ) ;
#40297 = DIRECTION ( 'NONE',  ( 0.5364919789714477361, 0.6444004775717706579, 0.5449076811759711036 ) ) ;
#40298 = DIRECTION ( 'NONE',  ( 0.007781995580012662783, 0.000000000000000000, -0.9999697198139514409 ) ) ;
#40299 = ORIENTED_EDGE ( 'NONE', *, *, #42453, .T. ) ;
#40300 = CARTESIAN_POINT ( 'NONE',  ( -10.00813838035478298, 0.000000000000000000, 10.77830692922518452 ) ) ;
#40301 = VERTEX_POINT ( 'NONE', #39427 ) ;
#40302 = DIRECTION ( 'NONE',  ( 0.005002170337468016433, -0.7660444431189770143, -0.6427681459581293666 ) ) ;
#40303 = CARTESIAN_POINT ( 'NONE',  ( -19.59569683186026268, 0.000000000000000000, 14.58168106541950948 ) ) ;
#40304 = DIRECTION ( 'NONE',  ( 0.007781995580012663651, -3.146120232559066537E-19, -0.9999697198139514409 ) ) ;
#40305 = DIRECTION ( 'NONE',  ( 0.000000000000000000, -0.000000000000000000, -1.000000000000000000 ) ) ;
#40306 = PLANE ( 'NONE',  #28649 ) ;
#40307 = DIRECTION ( 'NONE',  ( 1.000000000000000000, 0.000000000000000000, -0.000000000000000000 ) ) ;
#40308 = FACE_OUTER_BOUND ( 'NONE', #21876, .T. ) ;
#40309 = AXIS2_PLACEMENT_3D ( 'NONE', #53676, #14792, #38047 ) ;
#40310 = DIRECTION ( 'NONE',  ( -0.7660212471507179544, -0.6427876096865405842, -0.005961354470445141482 ) ) ;
#40311 = VECTOR ( 'NONE', #24161, 1000.000000000000227 ) ;
#40312 = DIRECTION ( 'NONE',  ( 0.005961354470445682716, -0.6427876096865404731, -0.7660212471507180654 ) ) ;
#40313 = ORIENTED_EDGE ( 'NONE', *, *, #44531, .T. ) ;
#40314 = CARTESIAN_POINT ( 'NONE',  ( -20.54049170961573267, 0.000000000000000000, 4.660556269540326646 ) ) ;
#40315 = LINE ( 'NONE', #13904, #28737 ) ;
#40316 = CARTESIAN_POINT ( 'NONE',  ( -67.98273966911209243, -0.9999999999999983347, -3.909888324369924284 ) ) ;
#40317 = AXIS2_PLACEMENT_3D ( 'NONE', #4820, #52521, #17601 ) ;
#40318 = CARTESIAN_POINT ( 'NONE',  ( -13.20081375640679866, 0.000000000000000000, 3.071021047694093564 ) ) ;
#40319 = CARTESIAN_POINT ( 'NONE',  ( -11.30636317915456779, -0.1191753592594197858, 11.32220194836580340 ) ) ;
#40320 = EDGE_CURVE ( 'NONE', #48789, #20913, #210, .T. ) ;
#40321 = FACE_OUTER_BOUND ( 'NONE', #2730, .T. ) ;
#40322 = DIRECTION ( 'NONE',  ( 0.5449076811759707706, 0.6444004775717708799, -0.5364919789714476250 ) ) ;
#40323 = ORIENTED_EDGE ( 'NONE', *, *, #51013, .F. ) ;
#40324 = VECTOR ( 'NONE', #46155, 1000.000000000000227 ) ;
#40325 = VERTEX_POINT ( 'NONE', #47668 ) ;
#40326 = PLANE ( 'NONE',  #13287 ) ;
#40327 = AXIS2_PLACEMENT_3D ( 'NONE', #42306, #29812, #3404 ) ;
#40328 = LINE ( 'NONE', #5149, #509 ) ;
#40329 = AXIS2_PLACEMENT_3D ( 'NONE', #53170, #48623, #1174 ) ;
#40330 = EDGE_LOOP ( 'NONE', ( #37967, #30751, #21143, #20133 ) ) ;
#40331 = CARTESIAN_POINT ( 'NONE',  ( -29.93654370153088706, 0.000000000000000000, 22.35628214185738116 ) ) ;
#40332 = ORIENTED_EDGE ( 'NONE', *, *, #27794, .F. ) ;
#40333 = LINE ( 'NONE', #49121, #18428 ) ;
#40334 = ADVANCED_FACE ( 'NONE', ( #34587 ), #4241, .F. ) ;
#40335 = AXIS2_PLACEMENT_3D ( 'NONE', #29070, #29673, #42135 ) ;
#40336 = ORIENTED_EDGE ( 'NONE', *, *, #49587, .F. ) ;
#40337 = VECTOR ( 'NONE', #51553, 1000.000000000000000 ) ;
#40338 = ORIENTED_EDGE ( 'NONE', *, *, #37848, .F. ) ;
#40339 = ORIENTED_EDGE ( 'NONE', *, *, #39615, .F. ) ;
#40340 = CARTESIAN_POINT ( 'NONE',  ( -14.01701317841955508, 0.000000000000000000, 2.326005055450897085 ) ) ;
#40341 = DIRECTION ( 'NONE',  ( -0.5449076811759708816, 0.6444004775717707689, 0.5364919789714475140 ) ) ;
#40342 = CARTESIAN_POINT ( 'NONE',  ( -16.74378146872023976, 0.000000000000000000, 6.367437481985902537 ) ) ;
#40343 = FACE_OUTER_BOUND ( 'NONE', #12061, .T. ) ;
#40344 = EDGE_CURVE ( 'NONE', #2394, #31162, #43661, .T. ) ;
#40345 = ORIENTED_EDGE ( 'NONE', *, *, #18135, .T. ) ;
#40346 = ORIENTED_EDGE ( 'NONE', *, *, #24436, .F. ) ;
#40347 = EDGE_CURVE ( 'NONE', #14766, #5010, #30888, .T. ) ;
#40348 = VECTOR ( 'NONE', #55902, 999.9999999999998863 ) ;
#40349 = CARTESIAN_POINT ( 'NONE',  ( -67.91473901113046452, -9.431317234435587338, -7.468518229136111408 ) ) ;
#40350 = AXIS2_PLACEMENT_3D ( 'NONE', #16968, #16664, #8739 ) ;
#40351 = ORIENTED_EDGE ( 'NONE', *, *, #25722, .T. ) ;
#40352 = EDGE_CURVE ( 'NONE', #38297, #31963, #9308, .T. ) ;
#40353 = DIRECTION ( 'NONE',  ( 0.9999697198139515519, 0.000000000000000000, 0.007781995580013368816 ) ) ;
#40354 = ORIENTED_EDGE ( 'NONE', *, *, #20109, .T. ) ;
#40355 = VECTOR ( 'NONE', #40996, 999.9999999999998863 ) ;
#40356 = CARTESIAN_POINT ( 'NONE',  ( 2.072287782118878319, 0.000000000000000000, -2.950529333540147015 ) ) ;
#40357 = LINE ( 'NONE', #17658, #26723 ) ;
#40358 = EDGE_CURVE ( 'NONE', #23668, #54371, #26099, .T. ) ;
#40359 = VERTEX_POINT ( 'NONE', #26938 ) ;
#40360 = LINE ( 'NONE', #14517, #53101 ) ;
#40361 = AXIS2_PLACEMENT_3D ( 'NONE', #7675, #38905, #34622 ) ;
#40362 = VERTEX_POINT ( 'NONE', #38871 ) ;
#40363 = EDGE_CURVE ( 'NONE', #45114, #8988, #44251, .T. ) ;
#40364 = CARTESIAN_POINT ( 'NONE',  ( 2.072287782118878319, 0.000000000000000000, -2.950529333540147015 ) ) ;
#40365 = AXIS2_PLACEMENT_3D ( 'NONE', #14861, #2619, #19941 ) ;
#40366 = VECTOR ( 'NONE', #3761, 999.9999999999998863 ) ;
#40367 = VERTEX_POINT ( 'NONE', #39970 ) ;
#40368 = CARTESIAN_POINT ( 'NONE',  ( 2.072287782118878319, 0.000000000000000000, -2.950529333540147015 ) ) ;
#40369 = CARTESIAN_POINT ( 'NONE',  ( -13.54170968098099159, -3.917936722690661178, 8.371993288704665304 ) ) ;
#40370 = AXIS2_PLACEMENT_3D ( 'NONE', #28153, #10592, #27314 ) ;
#40371 = LINE ( 'NONE', #1467, #5624 ) ;
#40372 = ORIENTED_EDGE ( 'NONE', *, *, #20523, .F. ) ;
#40373 = AXIS2_PLACEMENT_3D ( 'NONE', #18156, #5127, #5395 ) ;
#40374 = DIRECTION ( 'NONE',  ( 0.007781995580012662783, 0.000000000000000000, -0.9999697198139514409 ) ) ;
#40375 = DIRECTION ( 'NONE',  ( 0.6427681459581294776, -0.7660444431189769032, 0.005002170337467562802 ) ) ;
#40376 = CARTESIAN_POINT ( 'NONE',  ( -18.67775241435682432, 0.000000000000000000, 4.136394454059623804 ) ) ;
#40377 = CARTESIAN_POINT ( 'NONE',  ( -11.33651806203188883, 0.000000000000000000, 2.346865288250602255 ) ) ;
#40378 = FACE_OUTER_BOUND ( 'NONE', #29283, .T. ) ;
#40379 = VECTOR ( 'NONE', #11415, 999.9999999999998863 ) ;
#40380 = AXIS2_PLACEMENT_3D ( 'NONE', #29113, #11242, #55508 ) ;
#40381 = CARTESIAN_POINT ( 'NONE',  ( -66.78520713108927964, -9.487000657996272679, 0.6944083025908609486 ) ) ;
#40382 = VERTEX_POINT ( 'NONE', #56182 ) ;
#40383 = CARTESIAN_POINT ( 'NONE',  ( -15.99150919095859713, 0.000000000000000000, 3.418635280343801153 ) ) ;
#40384 = CARTESIAN_POINT ( 'NONE',  ( -14.60047255394062127, 0.000000000000000000, 3.798792718905593890 ) ) ;
#40385 = CARTESIAN_POINT ( 'NONE',  ( -65.67461282944442758, 2.602085213965210642E-15, 1.521991683923406224 ) ) ;
#40386 = ORIENTED_EDGE ( 'NONE', *, *, #2314, .F. ) ;
#40387 = DIRECTION ( 'NONE',  ( 0.6427681459581294776, -0.7660444431189769032, 0.005002170337467562802 ) ) ;
#40388 = CARTESIAN_POINT ( 'NONE',  ( -19.60834386242827776, 0.000000000000000000, 4.298478389818581213 ) ) ;
#40389 = ORIENTED_EDGE ( 'NONE', *, *, #43794, .F. ) ;
#40390 = EDGE_CURVE ( 'NONE', #3168, #50762, #17264, .T. ) ;
#40391 = LINE ( 'NONE', #36981, #36771 ) ;
#40392 = ADVANCED_FACE ( 'NONE', ( #40819 ), #18967, .F. ) ;
#40393 = FACE_OUTER_BOUND ( 'NONE', #14239, .T. ) ;
#40394 = DIRECTION ( 'NONE',  ( 0.007781995580012662783, 0.000000000000000000, -0.9999697198139514409 ) ) ;
#40395 = VECTOR ( 'NONE', #15257, 999.9999999999998863 ) ;
#40396 = VERTEX_POINT ( 'NONE', #27471 ) ;
#40397 = ORIENTED_EDGE ( 'NONE', *, *, #4292, .T. ) ;
#40398 = VECTOR ( 'NONE', #45312, 1000.000000000000227 ) ;
#40399 = EDGE_CURVE ( 'NONE', #24834, #44124, #37114, .T. ) ;
#40400 = DIRECTION ( 'NONE',  ( 0.6427681459581294776, -0.7660444431189769032, 0.005002170337467562802 ) ) ;
#40401 = CARTESIAN_POINT ( 'NONE',  ( -14.40335266348311372, 0.000000000000000000, 4.169658821279362826 ) ) ;
#40402 = VECTOR ( 'NONE', #49312, 999.9999999999998863 ) ;
#40403 = ADVANCED_FACE ( 'NONE', ( #53585 ), #1891, .F. ) ;
#40404 = EDGE_CURVE ( 'NONE', #38944, #27123, #41385, .T. ) ;
#40405 = ADVANCED_FACE ( 'NONE', ( #10451 ), #2476, .F. ) ;
#40406 = DIRECTION ( 'NONE',  ( -0.005002170337468016433, -0.7660444431189770143, 0.6427681459581293666 ) ) ;
#40407 = CARTESIAN_POINT ( 'NONE',  ( -25.20123094555300369, 0.000000000000000000, 6.470945668149052032 ) ) ;
#40408 = VERTEX_POINT ( 'NONE', #36552 ) ;
#40409 = DIRECTION ( 'NONE',  ( -0.7660212471507179544, -0.6427876096865405842, -0.005961354470445141482 ) ) ;
#40410 = VECTOR ( 'NONE', #5046, 1000.000000000000227 ) ;
#40411 = VERTEX_POINT ( 'NONE', #53863 ) ;
#40412 = DIRECTION ( 'NONE',  ( 0.9999697198139515519, 0.000000000000000000, 0.007781995580013368816 ) ) ;
#40413 = DIRECTION ( 'NONE',  ( 0.6427681459581294776, -0.7660444431189769032, 0.005002170337467562802 ) ) ;
#40414 = VECTOR ( 'NONE', #28771, 1000.000000000000114 ) ;
#40416 = ORIENTED_EDGE ( 'NONE', *, *, #15574, .T. ) ;
#40415 = VECTOR ( 'NONE', #28466, 999.9999999999998863 ) ;
#40417 = FACE_OUTER_BOUND ( 'NONE', #9287, .T. ) ;
#40418 = DIRECTION ( 'NONE',  ( -0.7660212471507179544, -0.6427876096865405842, -0.005961354470445141482 ) ) ;
#40419 = CARTESIAN_POINT ( 'NONE',  ( -14.46888367232926420, 0.000000000000000000, 12.59025272694991315 ) ) ;
#40420 = AXIS2_PLACEMENT_3D ( 'NONE', #19569, #33464, #36606 ) ;
#40421 = ORIENTED_EDGE ( 'NONE', *, *, #55040, .T. ) ;
#40422 = VECTOR ( 'NONE', #42923, 1000.000000000000227 ) ;
#40423 = PLANE ( 'NONE',  #52060 ) ;
#40424 = EDGE_CURVE ( 'NONE', #40269, #1575, #27776, .T. ) ;
#40425 = AXIS2_PLACEMENT_3D ( 'NONE', #12167, #43128, #51901 ) ;
#40426 = ORIENTED_EDGE ( 'NONE', *, *, #15289, .F. ) ;
#40427 = VECTOR ( 'NONE', #55209, 999.9999999999998863 ) ;
#40429 = ORIENTED_EDGE ( 'NONE', *, *, #14936, .F. ) ;
#40428 = EDGE_CURVE ( 'NONE', #52847, #27231, #23234, .T. ) ;
#40430 = VECTOR ( 'NONE', #17385, 999.9999999999998863 ) ;
#40431 = ORIENTED_EDGE ( 'NONE', *, *, #10122, .F. ) ;
#40432 = LINE ( 'NONE', #1523, #50469 ) ;
#40433 = EDGE_CURVE ( 'NONE', #42084, #36986, #14434, .T. ) ;
#40434 = ORIENTED_EDGE ( 'NONE', *, *, #9887, .F. ) ;
#40435 = DIRECTION ( 'NONE',  ( 0.007781995580012662783, 0.000000000000000000, -0.9999697198139514409 ) ) ;
#40436 = ORIENTED_EDGE ( 'NONE', *, *, #5333, .F. ) ;
#40437 = CARTESIAN_POINT ( 'NONE',  ( -19.06121784591510249, 0.000000000000000000, 5.610738516630323858 ) ) ;
#40438 = DIRECTION ( 'NONE',  ( 0.000000000000000000, -0.000000000000000000, -1.000000000000000000 ) ) ;
#40439 = ADVANCED_FACE ( 'NONE', ( #1639 ), #40563, .F. ) ;
#40440 = ORIENTED_EDGE ( 'NONE', *, *, #11248, .F. ) ;
#40441 = CARTESIAN_POINT ( 'NONE',  ( -18.67619601524082285, 0.000000000000000000, 3.936400510096834893 ) ) ;
#40442 = ORIENTED_EDGE ( 'NONE', *, *, #14006, .T. ) ;
#40443 = EDGE_CURVE ( 'NONE', #5277, #46034, #49336, .T. ) ;
#40444 = VECTOR ( 'NONE', #11112, 1000.000000000000114 ) ;
#40445 = PLANE ( 'NONE',  #25543 ) ;
#40446 = DIRECTION ( 'NONE',  ( 0.7660212471507180654, -0.6427876096865404731, 0.005961354470445141482 ) ) ;
#40447 = VECTOR ( 'NONE', #31246, 999.9999999999998863 ) ;
#40448 = LINE ( 'NONE', #6101, #39572 ) ;
#40449 = LINE ( 'NONE', #10639, #55642 ) ;
#40450 = LINE ( 'NONE', #1538, #46822 ) ;
#40451 = FACE_OUTER_BOUND ( 'NONE', #31580, .T. ) ;
#40452 = CARTESIAN_POINT ( 'NONE',  ( -10.27421835998572064, 0.000000000000000000, 10.96090226820206048 ) ) ;
#40453 = AXIS2_PLACEMENT_3D ( 'NONE', #46418, #21466, #34250 ) ;
#40454 = ORIENTED_EDGE ( 'NONE', *, *, #17647, .F. ) ;
#40455 = ORIENTED_EDGE ( 'NONE', *, *, #5607, .F. ) ;
#40456 = LINE ( 'NONE', #54060, #40975 ) ;
#40457 = DIRECTION ( 'NONE',  ( 0.007781995580012662783, 0.000000000000000000, -0.9999697198139514409 ) ) ;
#40458 = VECTOR ( 'NONE', #25016, 1000.000000000000227 ) ;
#40459 = DIRECTION ( 'NONE',  ( -0.5449076811759708816, 0.6444004775717707689, 0.5364919789714475140 ) ) ;
#40460 = VECTOR ( 'NONE', #8526, 1000.000000000000227 ) ;
#40461 = VECTOR ( 'NONE', #24487, 1000.000000000000227 ) ;
#40462 = DIRECTION ( 'NONE',  ( -0.000000000000000000, -0.000000000000000000, -1.000000000000000000 ) ) ;
#40463 = ORIENTED_EDGE ( 'NONE', *, *, #11909, .F. ) ;
#40464 = PLANE ( 'NONE',  #10443 ) ;
#40465 = DIRECTION ( 'NONE',  ( 0.007781995580012662783, 0.000000000000000000, -0.9999697198139514409 ) ) ;
#40466 = ORIENTED_EDGE ( 'NONE', *, *, #35426, .T. ) ;
#40467 = PLANE ( 'NONE',  #5760 ) ;
#40468 = PLANE ( 'NONE',  #4081 ) ;
#40469 = ORIENTED_EDGE ( 'NONE', *, *, #54420, .T. ) ;
#40470 = VECTOR ( 'NONE', #48973, 1000.000000000000000 ) ;
#40471 = CARTESIAN_POINT ( 'NONE',  ( -68.35070498065327627, -8.927360579512033212, 6.387117138744199174 ) ) ;
#40472 = DIRECTION ( 'NONE',  ( -0.9999697198139514409, -0.000000000000000000, -0.007781995580013368816 ) ) ;
#40473 = AXIS2_PLACEMENT_3D ( 'NONE', #22896, #1609, #18934 ) ;
#40474 = FACE_OUTER_BOUND ( 'NONE', #18884, .T. ) ;
#40475 = CARTESIAN_POINT ( 'NONE',  ( -26.13337879274045505, 0.000000000000000000, 6.833023547870798353 ) ) ;
#40476 = VECTOR ( 'NONE', #45768, 999.9999999999998863 ) ;
#40477 = DIRECTION ( 'NONE',  ( 0.5449076811759707706, 0.6444004775717708799, -0.5364919789714476250 ) ) ;
#40478 = ORIENTED_EDGE ( 'NONE', *, *, #28275, .T. ) ;
#40479 = VECTOR ( 'NONE', #53573, 999.9999999999998863 ) ;
#40480 = VERTEX_POINT ( 'NONE', #44502 ) ;
#40481 = CARTESIAN_POINT ( 'NONE',  ( -10.30646909681032142, -0.1191753592594186895, 2.254878339363226569 ) ) ;
#40482 = DIRECTION ( 'NONE',  ( -0.005961354470445682716, -0.6427876096865404731, 0.7660212471507180654 ) ) ;
#40483 = LINE ( 'NONE', #6387, #46931 ) ;
#40484 = ADVANCED_FACE ( 'NONE', ( #54165 ), #6458, .F. ) ;
#40485 = EDGE_CURVE ( 'NONE', #17974, #38400, #32316, .T. ) ;
#40486 = CARTESIAN_POINT ( 'NONE',  ( 5.850167541230363533, 0.0001172166011806737484, 1.544991542362377901 ) ) ;
#40487 = CARTESIAN_POINT ( 'NONE',  ( -36.91819796696599099, -1.000000000000000000, 21.84982018086542155 ) ) ;
#40489 = EDGE_CURVE ( 'NONE', #37705, #51242, #5001, .T. ) ;
#40488 = EDGE_LOOP ( 'NONE', ( #6471, #46993, #16714, #38518 ) ) ;
#40490 = CARTESIAN_POINT ( 'NONE',  ( -10.84028925556084388, -0.1191753592594197858, 11.14116300850493246 ) ) ;
#40491 = FACE_OUTER_BOUND ( 'NONE', #14299, .T. ) ;
#40492 = AXIS2_PLACEMENT_3D ( 'NONE', #40624, #27002, #19023 ) ;
#40493 = DIRECTION ( 'NONE',  ( -0.7660212471507179544, -0.6427876096865405842, -0.005961354470445141482 ) ) ;
#40494 = CARTESIAN_POINT ( 'NONE',  ( -22.40634380310664397, 0.000000000000000000, 5.584705972946605534 ) ) ;
#40495 = ORIENTED_EDGE ( 'NONE', *, *, #31578, .T. ) ;
#40496 = FACE_OUTER_BOUND ( 'NONE', #46309, .T. ) ;
#40497 = ORIENTED_EDGE ( 'NONE', *, *, #34926, .T. ) ;
#40498 = CARTESIAN_POINT ( 'NONE',  ( -11.82259098779923256, 0.000000000000000000, 5.097733058581920496 ) ) ;
#40499 = VECTOR ( 'NONE', #33529, 1000.000000000000114 ) ;
#40500 = DIRECTION ( 'NONE',  ( 0.5449076811759707706, 0.6444004775717708799, -0.5364919789714476250 ) ) ;
#40501 = ORIENTED_EDGE ( 'NONE', *, *, #5913, .T. ) ;
#40502 = CARTESIAN_POINT ( 'NONE',  ( -15.08941953321324725, 0.000000000000000000, 6.918970192494675153 ) ) ;
#40503 = VECTOR ( 'NONE', #48497, 999.9999999999998863 ) ;
#40504 = ORIENTED_EDGE ( 'NONE', *, *, #16165, .T. ) ;
#40505 = EDGE_CURVE ( 'NONE', #53467, #27029, #10152, .T. ) ;
#40506 = ORIENTED_EDGE ( 'NONE', *, *, #38832, .T. ) ;
#40507 = AXIS2_PLACEMENT_3D ( 'NONE', #17538, #13563, #30874 ) ;
#40508 = ORIENTED_EDGE ( 'NONE', *, *, #22760, .F. ) ;
#40509 = CARTESIAN_POINT ( 'NONE',  ( -12.13851405436063047, 0.000000000000000000, 11.68505802764555135 ) ) ;
#40510 = ORIENTED_EDGE ( 'NONE', *, *, #19449, .T. ) ;
#40511 = ORIENTED_EDGE ( 'NONE', *, *, #4499, .F. ) ;
#40512 = LINE ( 'NONE', #23462, #5730 ) ;
#40513 = DIRECTION ( 'NONE',  ( -0.5364919789714478471, 0.6444004775717705469, -0.5449076811759709926 ) ) ;
#40514 = ORIENTED_EDGE ( 'NONE', *, *, #36396, .F. ) ;
#40515 = EDGE_CURVE ( 'NONE', #291, #10918, #2176, .T. ) ;
#40516 = VECTOR ( 'NONE', #47848, 1000.000000000000114 ) ;
#40517 = VERTEX_POINT ( 'NONE', #19509 ) ;
#40518 = DIRECTION ( 'NONE',  ( -0.5364919789714478471, 0.6444004775717705469, -0.5449076811759709926 ) ) ;
#40519 = ORIENTED_EDGE ( 'NONE', *, *, #47935, .T. ) ;
#40520 = EDGE_LOOP ( 'NONE', ( #3258, #49202, #37613, #3879 ) ) ;
#40521 = EDGE_CURVE ( 'NONE', #19083, #24779, #32577, .T. ) ;
#40522 = VECTOR ( 'NONE', #50737, 999.9999999999998863 ) ;
#40523 = VECTOR ( 'NONE', #36765, 999.9999999999998863 ) ;
#40524 = PLANE ( 'NONE',  #37552 ) ;
#40525 = EDGE_CURVE ( 'NONE', #41560, #12666, #2721, .T. ) ;
#40526 = LINE ( 'NONE', #35998, #27580 ) ;
#40527 = CARTESIAN_POINT ( 'NONE',  ( -26.13493519185646008, 0.000000000000000000, 7.033017491833586377 ) ) ;
#40528 = PLANE ( 'NONE',  #40473 ) ;
#40529 = EDGE_CURVE ( 'NONE', #52907, #9714, #24890, .T. ) ;
#40530 = ORIENTED_EDGE ( 'NONE', *, *, #31402, .F. ) ;
#40531 = CARTESIAN_POINT ( 'NONE',  ( -20.53653072179030659, -0.1046794588179832119, 4.772753996012100153 ) ) ;
#40532 = EDGE_LOOP ( 'NONE', ( #3096, #4168, #34903, #44837 ) ) ;
#40533 = EDGE_CURVE ( 'NONE', #25397, #38228, #50987, .T. ) ;
#40534 = CARTESIAN_POINT ( 'NONE',  ( -27.99845268667336384, -0.1191753592594197858, 7.657176279295684118 ) ) ;
#40535 = VECTOR ( 'NONE', #12565, 999.9999999999998863 ) ;
#40536 = LINE ( 'NONE', #48768, #15214 ) ;
#40537 = LINE ( 'NONE', #33032, #52155 ) ;
#40538 = CARTESIAN_POINT ( 'NONE',  ( -12.70458494993575194, -0.1191753592594197858, 11.86531876794841978 ) ) ;
#40539 = DIRECTION ( 'NONE',  ( -0.9999697198139514409, -0.000000000000000000, -0.007781995580013368816 ) ) ;
#40540 = DIRECTION ( 'NONE',  ( -0.9999697198139514409, -0.000000000000000000, -0.007781995580013368816 ) ) ;
#40541 = EDGE_LOOP ( 'NONE', ( #34985, #7254, #3104, #46399 ) ) ;
#40542 = DIRECTION ( 'NONE',  ( 0.6427681459581294776, -0.7660444431189769032, 0.005002170337467562802 ) ) ;
#40543 = B_SPLINE_SURFACE_WITH_KNOTS ( 'NONE', 1, 3, ( 
 ( #11741, #19134, #27967, #49807, #46102, #6945, #10905, #37290, #28800, #23960, #54599, #41567, #16017, #29058 ),
 ( #41293, #28216, #33342, #45528, #46359, #7474, #6648, #36459, #53776, #32222, #45274, #40998, #2386, #54341 ) ),
 .UNSPECIFIED., .F., .F., .F.,
 ( 2, 2 ),
 ( 4, 2, 2, 2, 2, 2, 4 ),
 ( 0.000000000000000000, 1.000000000000000000 ),
 ( 0.000000000000000000, 0.1159099261691615840, 0.2318198523383231680, 0.4636397046766463359, 0.6954595570149695316, 0.9272794093532926718, 1.000000000000000000 ),
 .UNSPECIFIED. ) ;
#40544 = EDGE_LOOP ( 'NONE', ( #35335, #33742, #25169, #35832 ) ) ;
#40545 = CARTESIAN_POINT ( 'NONE',  ( -22.40634380310664397, 0.000000000000000000, 5.584705972946605534 ) ) ;
#40546 = DIRECTION ( 'NONE',  ( 0.005961354470445682716, -0.6427876096865404731, -0.7660212471507180654 ) ) ;
#40548 = CARTESIAN_POINT ( 'NONE',  ( -15.41378572042718353, -3.432230869623161595, 2.759052810919471188 ) ) ;
#40547 = VECTOR ( 'NONE', #2941, 1000.000000000000227 ) ;
#40549 = CARTESIAN_POINT ( 'NONE',  ( -18.43979397367102280, -1.489407457353156827, 3.996443418800899927 ) ) ;
#40550 = PLANE ( 'NONE',  #4198 ) ;
#40551 = AXIS2_PLACEMENT_3D ( 'NONE', #8387, #56106, #38490 ) ;
#40552 = CARTESIAN_POINT ( 'NONE',  ( -10.47421230394850866, 0.000000000000000000, 10.95934586908605723 ) ) ;
#40553 = ORIENTED_EDGE ( 'NONE', *, *, #44150, .T. ) ;
#40554 = CARTESIAN_POINT ( 'NONE',  ( 2.072287782118878319, 0.000000000000000000, -2.950529333540147015 ) ) ;
#40555 = CARTESIAN_POINT ( 'NONE',  ( -18.67775241435682432, 0.000000000000000000, 4.136394454059623804 ) ) ;
#40556 = DIRECTION ( 'NONE',  ( -0.5449076811759708816, 0.6444004775717707689, 0.5364919789714475140 ) ) ;
#40557 = ADVANCED_FACE ( 'NONE', ( #7562 ), #25192, .F. ) ;
#40558 = AXIS2_PLACEMENT_3D ( 'NONE', #5381, #53366, #1922 ) ;
#40559 = DIRECTION ( 'NONE',  ( 0.005002170337468016433, -0.7660444431189770143, -0.6427681459581293666 ) ) ;
#40560 = LINE ( 'NONE', #14693, #2178 ) ;
#40561 = ADVANCED_FACE ( 'NONE', ( #12097 ), #29431, .F. ) ;
#40562 = ADVANCED_FACE ( 'NONE', ( #7872 ), #12413, .F. ) ;
#40563 = PLANE ( 'NONE',  #44653 ) ;
#40564 = VECTOR ( 'NONE', #30415, 1000.000000000000227 ) ;
#40565 = DIRECTION ( 'NONE',  ( 0.005002170337468016433, -0.7660444431189770143, -0.6427681459581293666 ) ) ;
#40566 = DIRECTION ( 'NONE',  ( 0.000000000000000000, -0.000000000000000000, -1.000000000000000000 ) ) ;
#40567 = VERTEX_POINT ( 'NONE', #20892 ) ;
#40568 = VERTEX_POINT ( 'NONE', #28880 ) ;
#40569 = ORIENTED_EDGE ( 'NONE', *, *, #55222, .F. ) ;
#40570 = EDGE_LOOP ( 'NONE', ( #21064, #36246, #21136, #29386 ) ) ;
#40571 = ORIENTED_EDGE ( 'NONE', *, *, #11511, .F. ) ;
#40572 = CARTESIAN_POINT ( 'NONE',  ( -18.67697421479882181, -0.1191753592594197858, 4.036397482078229793 ) ) ;
#40573 = LINE ( 'NONE', #31495, #28523 ) ;
#40574 = B_SPLINE_CURVE_WITH_KNOTS ( 'NONE', 3,
 ( #41206, #19637, #49982, #11092 ),
 .UNSPECIFIED., .F., .F.,
 ( 4, 4 ),
 ( 0.000000000000000000, 0.0002286084161106520290 ),
 .UNSPECIFIED. ) ;
#40575 = ORIENTED_EDGE ( 'NONE', *, *, #26345, .T. ) ;
#40576 = EDGE_LOOP ( 'NONE', ( #50798, #49452, #52072, #16047, #40833 ) ) ;
#40577 = EDGE_LOOP ( 'NONE', ( #21274, #42980, #86, #24251 ) ) ;
#40578 = EDGE_CURVE ( 'NONE', #40517, #13439, #28590, .T. ) ;
#40579 = VECTOR ( 'NONE', #2399, 1000.000000000000000 ) ;
#40580 = CARTESIAN_POINT ( 'NONE',  ( -66.86496996703597517, -9.362286032850320794, -4.884162593219725679 ) ) ;
#40581 = EDGE_CURVE ( 'NONE', #54113, #25817, #42210, .T. ) ;
#40582 = FACE_OUTER_BOUND ( 'NONE', #54855, .T. ) ;
#40583 = FACE_OUTER_BOUND ( 'NONE', #36315, .T. ) ;
#40584 = VERTEX_POINT ( 'NONE', #20048 ) ;
#40585 = DIRECTION ( 'NONE',  ( 0.007781995580012662783, 0.000000000000000000, -0.9999697198139514409 ) ) ;
#40586 = ORIENTED_EDGE ( 'NONE', *, *, #41203, .F. ) ;
#40587 = AXIS2_PLACEMENT_3D ( 'NONE', #7260, #2980, #14954 ) ;
#40588 = DIRECTION ( 'NONE',  ( -0.6427681459581293666, -0.7660444431189770143, -0.005002170337467561935 ) ) ;
#40589 = EDGE_CURVE ( 'NONE', #42375, #40584, #3319, .T. ) ;
#40590 = CARTESIAN_POINT ( 'NONE',  ( -12.70458494993575194, -0.1191753592594197858, 11.86531876794841978 ) ) ;
#40591 = CARTESIAN_POINT ( 'NONE',  ( -17.16329905896135699, -4.403642575758163424, 3.407630086004865611 ) ) ;
#40592 = DIRECTION ( 'NONE',  ( 0.005961354470445682716, -0.6427876096865404731, -0.7660212471507180654 ) ) ;
#40593 = CARTESIAN_POINT ( 'NONE',  ( -11.91804826722769128, 25.86399001096056338, 3.000000000000000000 ) ) ;
#40594 = CARTESIAN_POINT ( 'NONE',  ( -23.33693525117809386, 0.000000000000000000, 5.746789908705562944 ) ) ;
#40595 = DIRECTION ( 'NONE',  ( 0.007781995580012663651, 0.000000000000000000, -0.9999697198139515519 ) ) ;
#40596 = VERTEX_POINT ( 'NONE', #20338 ) ;
#40597 = DIRECTION ( 'NONE',  ( 0.7660212471507180654, -0.6427876096865404731, 0.005961354470445141482 ) ) ;
#40598 = ORIENTED_EDGE ( 'NONE', *, *, #16613, .F. ) ;
#40599 = ADVANCED_FACE ( 'NONE', ( #24591 ), #41906, .F. ) ;
#40600 = B_SPLINE_CURVE_WITH_KNOTS ( 'NONE', 3,
 ( #3779, #16029, #33058, #12016 ),
 .UNSPECIFIED., .F., .F.,
 ( 4, 4 ),
 ( 0.6246544700140113093, 0.6386939402607147986 ),
 .UNSPECIFIED. ) ;
#40601 = CARTESIAN_POINT ( 'NONE',  ( -18.67775241435682432, 0.000000000000000000, 4.136394454059623804 ) ) ;
#40602 = DIRECTION ( 'NONE',  ( 0.7660212471507180654, -0.6427876096865404731, 0.005961354470445141482 ) ) ;
#40603 = FACE_OUTER_BOUND ( 'NONE', #2182, .T. ) ;
#40604 = DIRECTION ( 'NONE',  ( 0.5449076811759707706, 0.6444004775717708799, -0.5364919789714476250 ) ) ;
#40605 = CARTESIAN_POINT ( 'NONE',  ( -27.99845268667336384, -0.1191753592594197858, 7.657176279295684118 ) ) ;
#40606 = CARTESIAN_POINT ( 'NONE',  ( -21.47419595591918906, 0.000000000000000000, 5.222628093224860102 ) ) ;
#40608 = EDGE_CURVE ( 'NONE', #33095, #48957, #33419, .T. ) ;
#40607 = DIRECTION ( 'NONE',  ( 0.6427681459581294776, -0.7660444431189769032, 0.005002170337467562802 ) ) ;
#40609 = PLANE ( 'NONE',  #4817 ) ;
#40610 = DIRECTION ( 'NONE',  ( -0.005961354470445682716, -0.6427876096865404731, 0.7660212471507180654 ) ) ;
#40611 = ORIENTED_EDGE ( 'NONE', *, *, #46878, .T. ) ;
#40612 = CARTESIAN_POINT ( 'NONE',  ( -0.6946271361862269567, -5.340650597229416263, 3.488190344995370396 ) ) ;
#40613 = PLANE ( 'NONE',  #24900 ) ;
#40614 = EDGE_CURVE ( 'NONE', #29543, #17332, #42494, .T. ) ;
#40615 = LINE ( 'NONE', #37744, #12785 ) ;
#40616 = DIRECTION ( 'NONE',  ( 0.000000000000000000, -0.000000000000000000, -1.000000000000000000 ) ) ;
#40617 = EDGE_CURVE ( 'NONE', #32117, #3254, #55261, .T. ) ;
#40618 = CARTESIAN_POINT ( 'NONE',  ( -18.67619601524082285, 0.000000000000000000, 3.936400510096834893 ) ) ;
#40619 = CARTESIAN_POINT ( 'NONE',  ( -30.79567442779373110, 0.000000000000000000, 8.843406890442315316 ) ) ;
#40620 = ADVANCED_FACE ( 'NONE', ( #33677 ), #47035, .F. ) ;
#40621 = LINE ( 'NONE', #1694, #2965 ) ;
#40622 = ORIENTED_EDGE ( 'NONE', *, *, #54100, .T. ) ;
#40623 = EDGE_LOOP ( 'NONE', ( #7289, #43906, #26278, #35404 ) ) ;
#40624 = CARTESIAN_POINT ( 'NONE',  ( -15.60102546347950536, 0.000000000000000000, 12.95077420755565356 ) ) ;
#40625 = CARTESIAN_POINT ( 'NONE',  ( -18.79370083953152459, 0.000000000000000000, 5.243488326024565715 ) ) ;
#40626 = EDGE_CURVE ( 'NONE', #19288, #24739, #42751, .T. ) ;
#40627 = VECTOR ( 'NONE', #2001, 1000.000000000000000 ) ;
#40628 = ORIENTED_EDGE ( 'NONE', *, *, #51808, .T. ) ;
#40629 = CARTESIAN_POINT ( 'NONE',  ( -11.60247866929946525, 0.000000000000000000, 2.514121534893573262 ) ) ;
#40630 = ORIENTED_EDGE ( 'NONE', *, *, #30197, .F. ) ;
#40631 = PLANE ( 'NONE',  #30195 ) ;
#40632 = ADVANCED_FACE ( 'NONE', ( #37373 ), #11264, .F. ) ;
#40633 = EDGE_LOOP ( 'NONE', ( #1522, #1216, #28243, #42376, #10627 ) ) ;
#40634 = ORIENTED_EDGE ( 'NONE', *, *, #5916, .T. ) ;
#40635 = ORIENTED_EDGE ( 'NONE', *, *, #22062, .T. ) ;
#40636 = DIRECTION ( 'NONE',  ( 0.007781995580012663651, -3.146120232559066537E-19, -0.9999697198139514409 ) ) ;
#40637 = DIRECTION ( 'NONE',  ( -0.5364919789714478471, 0.6444004775717705469, -0.5449076811759709926 ) ) ;
#40638 = DIRECTION ( 'NONE',  ( -0.6427681459581293666, -0.7660444431189770143, -0.005002170337467561935 ) ) ;
#40639 = DIRECTION ( 'NONE',  ( -0.005002170337468016433, -0.7660444431189770143, 0.6427681459581293666 ) ) ;
#40640 = VERTEX_POINT ( 'NONE', #8712 ) ;
#40641 = ORIENTED_EDGE ( 'NONE', *, *, #25440, .F. ) ;
#40642 = DIRECTION ( 'NONE',  ( 0.5449076811759707706, 0.6444004775717708799, -0.5364919789714476250 ) ) ;
#40643 = ORIENTED_EDGE ( 'NONE', *, *, #25404, .F. ) ;
#40644 = CARTESIAN_POINT ( 'NONE',  ( -8.782761204222188312, 0.000000000000000000, 4.382725577236319836 ) ) ;
#40645 = VERTEX_POINT ( 'NONE', #31103 ) ;
#40646 = PLANE ( 'NONE',  #13111 ) ;
#40647 = CARTESIAN_POINT ( 'NONE',  ( -23.33771345073609638, -0.1191753592594197858, 5.846786880686956955 ) ) ;
#40648 = VERTEX_POINT ( 'NONE', #26561 ) ;
#40649 = CARTESIAN_POINT ( 'NONE',  ( -12.55851384766255663, -4.403642575758160760, 8.787212689424128698 ) ) ;
#40650 = EDGE_CURVE ( 'NONE', #47105, #31087, #5288, .T. ) ;
#40651 = EDGE_LOOP ( 'NONE', ( #10482, #2676, #29634, #47609 ) ) ;
#40652 = FACE_OUTER_BOUND ( 'NONE', #55130, .T. ) ;
#40653 = ADVANCED_FACE ( 'NONE', ( #47593 ), #29987, .F. ) ;
#40654 = ORIENTED_EDGE ( 'NONE', *, *, #9445, .T. ) ;
#40655 = DIRECTION ( 'NONE',  ( 0.8660254037844380415, 0.5000000000000011102, 0.000000000000000000 ) ) ;
#40656 = CARTESIAN_POINT ( 'NONE',  ( -19.79569077582305070, 0.000000000000000000, 14.58012466630350445 ) ) ;
#40657 = CARTESIAN_POINT ( 'NONE',  ( -20.23897083037251576, 0.6102101463440048335, 5.744283514253277545 ) ) ;
#40658 = ORIENTED_EDGE ( 'NONE', *, *, #11433, .T. ) ;
#40659 = ADVANCED_FACE ( 'NONE', ( #43053 ), #12675, .F. ) ;
#40660 = VECTOR ( 'NONE', #27831, 1000.000000000000227 ) ;
#40661 = CARTESIAN_POINT ( 'NONE',  ( -21.32662440292010686, -3.756034771668159689, 11.13020985957213860 ) ) ;
#40662 = DIRECTION ( 'NONE',  ( -0.5364919789714478471, 0.6444004775717705469, -0.5449076811759709926 ) ) ;
#40663 = LINE ( 'NONE', #13679, #11280 ) ;
#40664 = CARTESIAN_POINT ( 'NONE',  ( -56.62967144059850000, 4.128180327486781209, -2.384865143139781374 ) ) ;
#40665 = EDGE_CURVE ( 'NONE', #40102, #23572, #34811, .T. ) ;
#40666 = CARTESIAN_POINT ( 'NONE',  ( -18.35624807862726371, 0.000000000000000000, 8.740207326407432475 ) ) ;
#40668 = EDGE_CURVE ( 'NONE', #1004, #4402, #22326, .T. ) ;
#40667 = CARTESIAN_POINT ( 'NONE',  ( -17.74404816805336793, 0.000000000000000000, 3.574322630375089460 ) ) ;
#40669 = CARTESIAN_POINT ( 'NONE',  ( -67.85651025736190434, -11.48909734946287386, 5.667235587292936749 ) ) ;
#40670 = ORIENTED_EDGE ( 'NONE', *, *, #2239, .F. ) ;
#40671 = CARTESIAN_POINT ( 'NONE',  ( -10.74029228357944987, 0.000000000000000000, 11.14194120806293320 ) ) ;
#40672 = LINE ( 'NONE', #35553, #47637 ) ;
#40673 = CARTESIAN_POINT ( 'NONE',  ( -69.19654577526263495, 4.553649124439119412E-15, -7.934121704141924525 ) ) ;
#40674 = ORIENTED_EDGE ( 'NONE', *, *, #49469, .T. ) ;
#40675 = CARTESIAN_POINT ( 'NONE',  ( -22.12213066651850113, 5.629170628041515023, 5.095318538108095652 ) ) ;
#40676 = CARTESIAN_POINT ( 'NONE',  ( -1.086233639165236964, 0.000000000000000000, -2.796443541562362078 ) ) ;
#40677 = ORIENTED_EDGE ( 'NONE', *, *, #19102, .F. ) ;
#40678 = EDGE_CURVE ( 'NONE', #25320, #38090, #13777, .T. ) ;
#40679 = LINE ( 'NONE', #49475, #5923 ) ;
#40680 = LINE ( 'NONE', #10286, #32328 ) ;
#40681 = ADVANCED_FACE ( 'NONE', ( #17784 ), #9541, .F. ) ;
#40682 = FACE_OUTER_BOUND ( 'NONE', #51701, .T. ) ;
#40683 = ORIENTED_EDGE ( 'NONE', *, *, #34617, .T. ) ;
#40684 = ORIENTED_EDGE ( 'NONE', *, *, #21364, .F. ) ;
#40685 = DIRECTION ( 'NONE',  ( -0.7660212471507179544, -0.6427876096865405842, -0.005961354470445141482 ) ) ;
#40686 = LINE ( 'NONE', #48917, #54108 ) ;
#40687 = CARTESIAN_POINT ( 'NONE',  ( -15.32299166378033739, 3.038739411681507185, 7.820380517850593627 ) ) ;
#40688 = ADVANCED_FACE ( 'NONE', ( #30578 ), #8984, .F. ) ;
#40689 = VERTEX_POINT ( 'NONE', #35121 ) ;
#40690 = DIRECTION ( 'NONE',  ( -1.000000000000000000, 0.000000000000000000, 0.000000000000000000 ) ) ;
#40691 = ORIENTED_EDGE ( 'NONE', *, *, #19298, .T. ) ;
#40692 = CARTESIAN_POINT ( 'NONE',  ( -19.60834386242827776, 0.000000000000000000, 4.298478389818581213 ) ) ;
#40693 = ADVANCED_FACE ( 'NONE', ( #21754 ), #52126, .F. ) ;
#40694 = PLANE ( 'NONE',  #19687 ) ;
#40695 = ORIENTED_EDGE ( 'NONE', *, *, #32558, .T. ) ;
#40696 = LINE ( 'NONE', #1767, #5718 ) ;
#40697 = DIRECTION ( 'NONE',  ( -0.6427681459581293666, -0.7660444431189770143, -0.005002170337467561935 ) ) ;
#40698 = PLANE ( 'NONE',  #49328 ) ;
#40699 = ORIENTED_EDGE ( 'NONE', *, *, #9188, .F. ) ;
#40700 = VECTOR ( 'NONE', #30480, 999.9999999999998863 ) ;
#40701 = DIRECTION ( 'NONE',  ( -0.9999697198139514409, -0.000000000000000000, -0.007781995580013368816 ) ) ;
#40702 = ORIENTED_EDGE ( 'NONE', *, *, #10232, .F. ) ;
#40703 = ORIENTED_EDGE ( 'NONE', *, *, #50425, .F. ) ;
#40704 = VERTEX_POINT ( 'NONE', #38807 ) ;
#40705 = DIRECTION ( 'NONE',  ( 1.000000000000000000, -3.469446951953611033E-15, 0.000000000000000000 ) ) ;
#40706 = ORIENTED_EDGE ( 'NONE', *, *, #782, .F. ) ;
#40707 = CARTESIAN_POINT ( 'NONE',  ( -66.90530812237336988, -8.360358167099661841, 0.5932824550257441709 ) ) ;
#40708 = ORIENTED_EDGE ( 'NONE', *, *, #12634, .F. ) ;
#40709 = DIRECTION ( 'NONE',  ( -0.7660212471507179544, -0.6427876096865405842, -0.005961354470445141482 ) ) ;
#40710 = DIRECTION ( 'NONE',  ( 0.000000000000000000, 0.000000000000000000, 1.000000000000000000 ) ) ;
#40711 = ORIENTED_EDGE ( 'NONE', *, *, #41307, .T. ) ;
#40712 = CARTESIAN_POINT ( 'NONE',  ( -19.60990026154428278, 0.000000000000000000, 4.498472333781370125 ) ) ;
#40713 = EDGE_CURVE ( 'NONE', #27792, #5782, #9241, .T. ) ;
#40714 = VERTEX_POINT ( 'NONE', #39906 ) ;
#40715 = CARTESIAN_POINT ( 'NONE',  ( -14.93495759592298988, 0.000000000000000000, 12.77129166681078409 ) ) ;
#40716 = EDGE_CURVE ( 'NONE', #25279, #28407, #4704, .T. ) ;
#40717 = DIRECTION ( 'NONE',  ( -0.9999697198139514409, -0.000000000000000000, -0.007781995580013368816 ) ) ;
#40718 = CARTESIAN_POINT ( 'NONE',  ( -27.13182931993292257, 16.99370688441070953, 4.657440554554202805 ) ) ;
#40719 = ADVANCED_FACE ( 'NONE', ( #34272 ), #52420, .F. ) ;
#40720 = DIRECTION ( 'NONE',  ( 0.9999697198139515519, 0.000000000000000000, 0.007781995580013368816 ) ) ;
#40721 = FACE_OUTER_BOUND ( 'NONE', #34220, .T. ) ;
#40722 = CARTESIAN_POINT ( 'NONE',  ( -26.13415699229845757, -0.1191753592594197858, 6.933020519852192365 ) ) ;
#40723 = CARTESIAN_POINT ( 'NONE',  ( -11.37388075760056161, 0.000000000000000000, 7.147891430601540641 ) ) ;
#40724 = ORIENTED_EDGE ( 'NONE', *, *, #2007, .T. ) ;
#40725 = ADVANCED_FACE ( 'NONE', ( #30832 ), #12946, .F. ) ;
#40726 = EDGE_CURVE ( 'NONE', #15181, #50938, #35372, .T. ) ;
#40727 = ADVANCED_FACE ( 'NONE', ( #30275 ), #31946, .F. ) ;
#40728 = VERTEX_POINT ( 'NONE', #40186 ) ;
#40729 = DIRECTION ( 'NONE',  ( -0.005961354470445682716, -0.6427876096865404731, 0.7660212471507180654 ) ) ;
#40730 = CARTESIAN_POINT ( 'NONE',  ( -16.79925329029790149, 0.000000000000000000, 13.49544742625427496 ) ) ;
#40731 = CARTESIAN_POINT ( 'NONE',  ( -18.71016998902382511, -0.1191753592594162470, 7.360127773147754127 ) ) ;
#40732 = CARTESIAN_POINT ( 'NONE',  ( -6.110905869600904872, 1.712176620043476140E-14, 2.600000000000000089 ) ) ;
#40733 = VERTEX_POINT ( 'NONE', #31411 ) ;
#40734 = PLANE ( 'NONE',  #20379 ) ;
#40735 = CARTESIAN_POINT ( 'NONE',  ( -18.36067853124854921, 0.000000000000000000, 9.309510973627983077 ) ) ;
#40736 = ORIENTED_EDGE ( 'NONE', *, *, #49477, .F. ) ;
#40737 = DIRECTION ( 'NONE',  ( 0.005961354470445682716, -0.6427876096865404731, -0.7660212471507180654 ) ) ;
#40738 = CARTESIAN_POINT ( 'NONE',  ( -20.84197899872283699, 20.43270222331197061, 4.347644189603123266 ) ) ;
#40739 = VERTEX_POINT ( 'NONE', #28742 ) ;
#40740 =( GEOMETRIC_REPRESENTATION_CONTEXT ( 3 ) GLOBAL_UNCERTAINTY_ASSIGNED_CONTEXT ( ( #24562 ) ) GLOBAL_UNIT_ASSIGNED_CONTEXT ( ( #48842, #582, #5663 ) ) REPRESENTATION_CONTEXT ( 'NONE', 'WORKASPACE' ) );
#40741 = DIRECTION ( 'NONE',  ( -0.7660212471507179544, -0.6427876096865405842, -0.005961354470445141482 ) ) ;
#40742 = PLANE ( 'NONE',  #22423 ) ;
#40743 = EDGE_CURVE ( 'NONE', #39023, #45704, #19917, .T. ) ;
#40744 = DIRECTION ( 'NONE',  ( 0.007781995580012663651, 0.000000000000000000, -0.9999697198139515519 ) ) ;
#40745 = FACE_OUTER_BOUND ( 'NONE', #16035, .T. ) ;
#40746 = EDGE_CURVE ( 'NONE', #19074, #46703, #18616, .T. ) ;
#40747 = DIRECTION ( 'NONE',  ( 0.5364919789714477361, 0.6444004775717706579, 0.5449076811759711036 ) ) ;
#40748 = EDGE_LOOP ( 'NONE', ( #19866, #2998, #20153, #17205 ) ) ;
#40749 = ORIENTED_EDGE ( 'NONE', *, *, #40063, .T. ) ;
#40750 = ADVANCED_FACE ( 'NONE', ( #40491 ), #18907, .F. ) ;
#40751 = LINE ( 'NONE', #23433, #10349 ) ;
#40752 = CARTESIAN_POINT ( 'NONE',  ( -10.81131361120978696, -0.1191753592594194527, 7.417854936013363876 ) ) ;
#40753 = LINE ( 'NONE', #5281, #13385 ) ;
#40754 = EDGE_CURVE ( 'NONE', #45599, #39737, #23442, .T. ) ;
#40755 = CARTESIAN_POINT ( 'NONE',  ( -12.99507170543344436, 0.000000000000000000, 2.333958040294567660 ) ) ;
#40756 = DIRECTION ( 'NONE',  ( 0.000000000000000000, -1.000000000000000000, 0.000000000000000000 ) ) ;
#40757 = VERTEX_POINT ( 'NONE', #22863 ) ;
#40758 = PLANE ( 'NONE',  #15611 ) ;
#40759 = DIRECTION ( 'NONE',  ( 0.007781995580012663651, 0.000000000000000000, -0.9999697198139515519 ) ) ;
#40760 = FACE_OUTER_BOUND ( 'NONE', #8657, .T. ) ;
#40761 = DIRECTION ( 'NONE',  ( 0.007781995580012663651, -3.146120232559066537E-19, -0.9999697198139514409 ) ) ;
#40762 = ORIENTED_EDGE ( 'NONE', *, *, #18086, .T. ) ;
#40763 = CARTESIAN_POINT ( 'NONE',  ( -12.53462651648692194, 0.000000000000000000, 2.876199414615318251 ) ) ;
#40764 = ORIENTED_EDGE ( 'NONE', *, *, #42407, .T. ) ;
#40765 = LINE ( 'NONE', #8080, #12343 ) ;
#40766 = PLANE ( 'NONE',  #1237 ) ;
#40767 = EDGE_LOOP ( 'NONE', ( #32649, #46343, #56071, #5845 ) ) ;
#40768 = CARTESIAN_POINT ( 'NONE',  ( -13.17065887352947762, -0.1191753592594197858, 12.04635770780929427 ) ) ;
#40769 = VERTEX_POINT ( 'NONE', #36221 ) ;
#40770 = ORIENTED_EDGE ( 'NONE', *, *, #37258, .T. ) ;
#40771 = ORIENTED_EDGE ( 'NONE', *, *, #22422, .F. ) ;
#40772 = DIRECTION ( 'NONE',  ( 0.7660212471507180654, -0.6427876096865404731, 0.005961354470445141482 ) ) ;
#40773 = ORIENTED_EDGE ( 'NONE', *, *, #46152, .F. ) ;
#40774 = ORIENTED_EDGE ( 'NONE', *, *, #40989, .F. ) ;
#40775 = DIRECTION ( 'NONE',  ( 0.007781995580012663651, -3.146120232559066537E-19, -0.9999697198139514409 ) ) ;
#40776 = DIRECTION ( 'NONE',  ( -0.005961354470445682716, -0.6427876096865404731, 0.7660212471507180654 ) ) ;
#40777 = ORIENTED_EDGE ( 'NONE', *, *, #10402, .F. ) ;
#40778 = VERTEX_POINT ( 'NONE', #2859 ) ;
#40779 = LINE ( 'NONE', #37625, #31362 ) ;
#40780 = ORIENTED_EDGE ( 'NONE', *, *, #49333, .F. ) ;
#40781 = EDGE_CURVE ( 'NONE', #47262, #21619, #986, .T. ) ;
#40782 = ORIENTED_EDGE ( 'NONE', *, *, #14757, .T. ) ;
#40783 = B_SPLINE_CURVE_WITH_KNOTS ( 'NONE', 3,
 ( #21794, #25232, #42538, #3629, #17534, #38259, #12717, #26080, #30036, #55583, #51346, #43389, #4485, #25488, #42796, #39110 ),
 .UNSPECIFIED., .F., .F.,
 ( 4, 2, 2, 2, 2, 2, 2, 4 ),
 ( 0.000000000000000000, 0.0002924226556627319796, 0.0005848453113254639592, 0.0008772679669881960473, 0.001169690622650927918, 0.001462113278313660440, 0.001754535933976393179, 0.002339381245301844995 ),
 .UNSPECIFIED. ) ;
#40784 = DIRECTION ( 'NONE',  ( 0.7660212471507180654, -0.6427876096865404731, 0.005961354470445141482 ) ) ;
#40785 = DIRECTION ( 'NONE',  ( 0.000000000000000000, 0.000000000000000000, 1.000000000000000000 ) ) ;
#40786 = CARTESIAN_POINT ( 'NONE',  ( -15.02654820080420706, -4.079838673713164887, 2.587974528106823602 ) ) ;
#40787 = CARTESIAN_POINT ( 'NONE',  ( -20.54126990917373519, -0.1191753592594197858, 4.760553241521720658 ) ) ;
#40788 = VERTEX_POINT ( 'NONE', #50298 ) ;
#40789 = CARTESIAN_POINT ( 'NONE',  ( -21.47263955680318404, 0.000000000000000000, 5.022634149262071190 ) ) ;
#40790 = VERTEX_POINT ( 'NONE', #37237 ) ;
#40791 = EDGE_CURVE ( 'NONE', #36173, #48176, #53278, .T. ) ;
#40792 = ADVANCED_FACE ( 'NONE', ( #11413 ), #54539, .F. ) ;
#40793 = EDGE_CURVE ( 'NONE', #3654, #19401, #46050, .T. ) ;
#40794 = CARTESIAN_POINT ( 'NONE',  ( -17.29326687045830724, -0.1191753592594164690, 4.416497882389668561 ) ) ;
#40795 = EDGE_CURVE ( 'NONE', #52907, #37899, #31682, .T. ) ;
#40796 = CARTESIAN_POINT ( 'NONE',  ( -37.76980095258905124, 10.85187109866503263, -4.935120467404106925 ) ) ;
#40797 = DIRECTION ( 'NONE',  ( 0.9999697198139515519, 0.000000000000000000, 0.007781995580013368816 ) ) ;
#40798 = FACE_OUTER_BOUND ( 'NONE', #16956, .T. ) ;
#40799 = CARTESIAN_POINT ( 'NONE',  ( -18.19747506107908563, 0.000000000000000000, 14.03856424583689311 ) ) ;
#40800 = CARTESIAN_POINT ( 'NONE',  ( -20.09258446552595245, -0.1191753592594195638, 5.872041224812675431 ) ) ;
#40801 = ORIENTED_EDGE ( 'NONE', *, *, #42849, .T. ) ;
#40802 = DIRECTION ( 'NONE',  ( 0.000000000000000000, -1.000000000000000000, 0.000000000000000000 ) ) ;
#40803 = VERTEX_POINT ( 'NONE', #27399 ) ;
#40804 = LINE ( 'NONE', #10722, #5680 ) ;
#40805 = LINE ( 'NONE', #53848, #15128 ) ;
#40806 = LINE ( 'NONE', #14422, #39018 ) ;
#40807 = DIRECTION ( 'NONE',  ( -0.005961354470445682716, -0.6427876096865404731, 0.7660212471507180654 ) ) ;
#40808 = DIRECTION ( 'NONE',  ( 0.000000000000000000, -1.000000000000000000, 0.000000000000000000 ) ) ;
#40809 = CARTESIAN_POINT ( 'NONE',  ( -12.64977195555273148, -0.1191753592594188005, 4.821966703327531079 ) ) ;
#40810 = ORIENTED_EDGE ( 'NONE', *, *, #51310, .T. ) ;
#40811 = EDGE_CURVE ( 'NONE', #43546, #14582, #44721, .T. ) ;
#40812 = LINE ( 'NONE', #6450, #39369 ) ;
#40813 = DIRECTION ( 'NONE',  ( 0.007781995580012662783, 0.000000000000000000, -0.9999697198139514409 ) ) ;
#40814 = DIRECTION ( 'NONE',  ( 0.3583679495452941066, 0.9335804264972041855, -0.000000000000000000 ) ) ;
#40815 = EDGE_CURVE ( 'NONE', #40825, #6164, #24456, .T. ) ;
#40816 = DIRECTION ( 'NONE',  ( 0.007781995580012662783, 0.000000000000000000, -0.9999697198139514409 ) ) ;
#40817 = LINE ( 'NONE', #10733, #51145 ) ;
#40818 = DIRECTION ( 'NONE',  ( 0.7660212471507180654, -0.6427876096865404731, 0.005961354470445141482 ) ) ;
#40819 = FACE_OUTER_BOUND ( 'NONE', #17750, .T. ) ;
#40820 = ADVANCED_FACE ( 'NONE', ( #5839 ), #23161, .F. ) ;
#40821 = DIRECTION ( 'NONE',  ( -0.6427681459581293666, -0.7660444431189770143, -0.005002170337467561935 ) ) ;
#40822 = CARTESIAN_POINT ( 'NONE',  ( -14.81148421494233780, -3.270328918600661439, 2.530263971831323566 ) ) ;
#40823 = ORIENTED_EDGE ( 'NONE', *, *, #9121, .T. ) ;
#40824 = ORIENTED_EDGE ( 'NONE', *, *, #3462, .F. ) ;
#40825 = VERTEX_POINT ( 'NONE', #30471 ) ;
#40826 = ORIENTED_EDGE ( 'NONE', *, *, #44878, .F. ) ;
#40827 = ORIENTED_EDGE ( 'NONE', *, *, #37405, .T. ) ;
#40828 = EDGE_LOOP ( 'NONE', ( #40351, #2824, #48655, #19455 ) ) ;
#40829 = LINE ( 'NONE', #40572, #17862 ) ;
#40830 = DIRECTION ( 'NONE',  ( -0.5449076811759708816, 0.6444004775717707689, 0.5364919789714475140 ) ) ;
#40831 = EDGE_LOOP ( 'NONE', ( #20626, #22572, #38938 ) ) ;
#40832 = ORIENTED_EDGE ( 'NONE', *, *, #39654, .F. ) ;
#40833 = ORIENTED_EDGE ( 'NONE', *, *, #41738, .F. ) ;
#40834 = VECTOR ( 'NONE', #45953, 1000.000000000000227 ) ;
#40835 = DIRECTION ( 'NONE',  ( 0.000000000000000000, 0.000000000000000000, 1.000000000000000000 ) ) ;
#40836 = CARTESIAN_POINT ( 'NONE',  ( -15.50102849149811135, -0.1191753592594197858, 12.95155240711365430 ) ) ;
#40837 = CARTESIAN_POINT ( 'NONE',  ( -19.60834386242827776, 0.000000000000000000, 4.298478389818581213 ) ) ;
#40838 = ORIENTED_EDGE ( 'NONE', *, *, #20107, .F. ) ;
#40839 = DIRECTION ( 'NONE',  ( 0.5449076811759707706, 0.6444004775717708799, -0.5364919789714476250 ) ) ;
#40841 = ORIENTED_EDGE ( 'NONE', *, *, #5091, .T. ) ;
#40840 = EDGE_CURVE ( 'NONE', #6678, #37427, #8894, .T. ) ;
#40842 = FACE_OUTER_BOUND ( 'NONE', #7368, .T. ) ;
#40843 = DIRECTION ( 'NONE',  ( -0.005961354470445682716, -0.6427876096865404731, 0.7660212471507180654 ) ) ;
#40844 = EDGE_CURVE ( 'NONE', #55993, #32241, #52020, .T. ) ;
#40845 = EDGE_CURVE ( 'NONE', #23263, #34917, #892, .T. ) ;
#40846 = CARTESIAN_POINT ( 'NONE',  ( -28.92982233430281980, 0.000000000000000000, 7.919257187036034651 ) ) ;
#40847 = DIRECTION ( 'NONE',  ( 0.5364919789714477361, 0.6444004775717706579, 0.5449076811759711036 ) ) ;
#40848 = LINE ( 'NONE', #44832, #19518 ) ;
#40849 = DIRECTION ( 'NONE',  ( 0.007781995580012663651, 0.000000000000000000, -0.9999697198139515519 ) ) ;
#40850 = LINE ( 'NONE', #20084, #24841 ) ;
#40851 = CARTESIAN_POINT ( 'NONE',  ( -29.86274838104827367, -0.1191753592594197858, 8.381332038739175871 ) ) ;
#40852 = ORIENTED_EDGE ( 'NONE', *, *, #27192, .T. ) ;
#40853 = LINE ( 'NONE', #44289, #23776 ) ;
#40854 = ORIENTED_EDGE ( 'NONE', *, *, #40390, .F. ) ;
#40855 = DIRECTION ( 'NONE',  ( 0.9999697198139515519, 0.000000000000000000, 0.007781995580013368816 ) ) ;
#40856 = DIRECTION ( 'NONE',  ( -0.6427681459581293666, -0.7660444431189770143, -0.005002170337467561935 ) ) ;
#40857 = DIRECTION ( 'NONE',  ( 0.9999697198139515519, 0.000000000000000000, 0.007781995580013368816 ) ) ;
#40858 = CARTESIAN_POINT ( 'NONE',  ( -19.60834386242827776, 0.000000000000000000, 4.298478389818581213 ) ) ;
#40859 = DIRECTION ( 'NONE',  ( 0.000000000000000000, 0.000000000000000000, 1.000000000000000000 ) ) ;
#40860 = CARTESIAN_POINT ( 'NONE',  ( -22.12471055240100881, 3.362543313726509719, 10.99381648943753476 ) ) ;
#40861 = LINE ( 'NONE', #27240, #5323 ) ;
#40862 = CARTESIAN_POINT ( 'NONE',  ( -8.609916609573598834, 0.000000000000000000, 10.23519010964256637 ) ) ;
#40863 =( NAMED_UNIT ( * ) PLANE_ANGLE_UNIT ( ) SI_UNIT ( $, .RADIAN. ) );
#40864 = CARTESIAN_POINT ( 'NONE',  ( -24.26908309836554878, 0.000000000000000000, 6.108867788427308376 ) ) ;
#40865 = VERTEX_POINT ( 'NONE', #18212 ) ;
#40866 = DIRECTION ( 'NONE',  ( 0.5449076811759707706, 0.6444004775717708799, -0.5364919789714476250 ) ) ;
#40867 = DIRECTION ( 'NONE',  ( -0.5449076811759708816, 0.6444004775717707689, 0.5364919789714475140 ) ) ;
#40868 = CARTESIAN_POINT ( 'NONE',  ( -67.56320601492518563, -0.9999999999999978906, -2.442027903730110250 ) ) ;
#40869 = DIRECTION ( 'NONE',  ( -0.5364919789714478471, 0.6444004775717705469, -0.5449076811759709926 ) ) ;
#40870 = AXIS2_PLACEMENT_3D ( 'NONE', #17364, #39541, #17108 ) ;
#40871 = DIRECTION ( 'NONE',  ( -0.005002170337468016433, -0.7660444431189770143, 0.6427681459581293666 ) ) ;
#40872 = DIRECTION ( 'NONE',  ( 0.005961354470445682716, -0.6427876096865404731, -0.7660212471507180654 ) ) ;
#40873 = EDGE_CURVE ( 'NONE', #41466, #49575, #26198, .T. ) ;
#40874 = LINE ( 'NONE', #1952, #42325 ) ;
#40875 = PLANE ( 'NONE',  #29247 ) ;
#40876 = ORIENTED_EDGE ( 'NONE', *, *, #15880, .F. ) ;
#40877 = VECTOR ( 'NONE', #11104, 1000.000000000000227 ) ;
#40878 = VERTEX_POINT ( 'NONE', #26748 ) ;
#40879 = EDGE_CURVE ( 'NONE', #32990, #34138, #22214, .T. ) ;
#40880 = CARTESIAN_POINT ( 'NONE',  ( -24.26908309836554878, 0.000000000000000000, 6.108867788427308376 ) ) ;
#40881 = LINE ( 'NONE', #20115, #35914 ) ;
#40882 = ORIENTED_EDGE ( 'NONE', *, *, #25075, .F. ) ;
#40883 = DIRECTION ( 'NONE',  ( -0.005961354470445682716, -0.6427876096865404731, 0.7660212471507180654 ) ) ;
#40884 = EDGE_CURVE ( 'NONE', #9862, #17943, #13136, .T. ) ;
#40885 = ORIENTED_EDGE ( 'NONE', *, *, #14966, .T. ) ;
#40886 = LINE ( 'NONE', #44577, #42911 ) ;
#40887 = ORIENTED_EDGE ( 'NONE', *, *, #10054, .F. ) ;
#40888 = ORIENTED_EDGE ( 'NONE', *, *, #37764, .T. ) ;
#40889 = ORIENTED_EDGE ( 'NONE', *, *, #17035, .F. ) ;
#40890 = DIRECTION ( 'NONE',  ( -0.6427681459581293666, -0.7660444431189770143, -0.005002170337467561935 ) ) ;
#40891 = DIRECTION ( 'NONE',  ( -0.5364919789714478471, 0.6444004775717705469, -0.5449076811759709926 ) ) ;
#40892 = PLANE ( 'NONE',  #5799 ) ;
#40893 = VECTOR ( 'NONE', #21279, 999.9999999999998863 ) ;
#40894 = ORIENTED_EDGE ( 'NONE', *, *, #32819, .T. ) ;
#40895 = ORIENTED_EDGE ( 'NONE', *, *, #11219, .T. ) ;
#40896 = FACE_OUTER_BOUND ( 'NONE', #41717, .T. ) ;
#40897 = EDGE_LOOP ( 'NONE', ( #13596, #41099, #10943, #30835 ) ) ;
#40898 = LINE ( 'NONE', #7118, #32759 ) ;
#40899 = EDGE_CURVE ( 'NONE', #34678, #33817, #34701, .T. ) ;
#40900 = EDGE_LOOP ( 'NONE', ( #18012, #25670, #36038, #53267 ) ) ;
#40901 = LINE ( 'NONE', #41186, #32122 ) ;
#40902 = CARTESIAN_POINT ( 'NONE',  ( -11.20636620717317378, 0.000000000000000000, 11.32298014792380414 ) ) ;
#40903 = ORIENTED_EDGE ( 'NONE', *, *, #19542, .T. ) ;
#40904 = VECTOR ( 'NONE', #23529, 1000.000000000000000 ) ;
#40905 = DIRECTION ( 'NONE',  ( 0.007781995580012663651, 0.000000000000000000, -0.9999697198139515519 ) ) ;
#40906 = EDGE_CURVE ( 'NONE', #51780, #50886, #4351, .T. ) ;
#40907 = VECTOR ( 'NONE', #23555, 999.9999999999998863 ) ;
#40908 = CARTESIAN_POINT ( 'NONE',  ( -19.18251504283423259, 1.581621852479005774, 4.082609997287097947 ) ) ;
#40909 = ORIENTED_EDGE ( 'NONE', *, *, #53041, .T. ) ;
#40910 = DIRECTION ( 'NONE',  ( 0.9999697198139515519, 0.000000000000000000, 0.007781995580013368816 ) ) ;
#40911 = CARTESIAN_POINT ( 'NONE',  ( -18.99737516508532309, 0.000000000000000000, 8.735217927174451447 ) ) ;
#40912 = CARTESIAN_POINT ( 'NONE',  ( -8.509919637592204822, -0.1191753592594197858, 10.23596830920056711 ) ) ;
#40913 = VERTEX_POINT ( 'NONE', #45131 ) ;
#40914 = CARTESIAN_POINT ( 'NONE',  ( 2.072287782118878319, 0.000000000000000000, -2.950529333540147015 ) ) ;
#40915 = FACE_OUTER_BOUND ( 'NONE', #15472, .T. ) ;
#40916 = LINE ( 'NONE', #1997, #37597 ) ;
#40917 = DIRECTION ( 'NONE',  ( -0.005002170337468016433, -0.7660444431189770143, 0.6427681459581293666 ) ) ;
#40918 = LINE ( 'NONE', #40081, #43968 ) ;
#40919 = DIRECTION ( 'NONE',  ( 0.005961354470445682716, -0.6427876096865404731, -0.7660212471507180654 ) ) ;
#40920 = ADVANCED_FACE ( 'NONE', ( #637 ), #39240, .F. ) ;
#40921 = CARTESIAN_POINT ( 'NONE',  ( -69.49740922963668766, -9.798021964684151541, 7.577667541101590132 ) ) ;
#40922 = ORIENTED_EDGE ( 'NONE', *, *, #4687, .T. ) ;
#40923 = DIRECTION ( 'NONE',  ( -0.8531650599175527594, 0.4028455766673922356, 0.3313982828793700652 ) ) ;
#40924 = LINE ( 'NONE', #16210, #52172 ) ;
#40925 = CARTESIAN_POINT ( 'NONE',  ( -69.23745231081454676, -0.5995258673811661998, -7.041125024142530719 ) ) ;
#40926 = VERTEX_POINT ( 'NONE', #23534 ) ;
#40927 = DIRECTION ( 'NONE',  ( -0.1139275668495183524, 0.9934890585767659488, 4.694855797473114533E-16 ) ) ;
#40928 = CARTESIAN_POINT ( 'NONE',  ( -29.86197018149027116, 0.000000000000000000, 8.281335066757780083 ) ) ;
#40929 = VECTOR ( 'NONE', #28664, 999.9999999999998863 ) ;
#40930 = AXIS2_PLACEMENT_3D ( 'NONE', #2565, #37480, #33252 ) ;
#40931 = DIRECTION ( 'NONE',  ( 0.007781995580012662783, 0.000000000000000000, -0.9999697198139514409 ) ) ;
#40932 = LINE ( 'NONE', #31861, #4277 ) ;
#40933 = CARTESIAN_POINT ( 'NONE',  ( 2.072287782118878319, 0.000000000000000000, -2.950529333540147015 ) ) ;
#40934 = VERTEX_POINT ( 'NONE', #39813 ) ;
#40935 = ORIENTED_EDGE ( 'NONE', *, *, #15645, .T. ) ;
#40936 = LINE ( 'NONE', #15131, #7766 ) ;
#40937 = DIRECTION ( 'NONE',  ( 0.7660212471507180654, -0.6427876096865404731, 0.005961354470445141482 ) ) ;
#40938 = CARTESIAN_POINT ( 'NONE',  ( -25.20278734466900517, 0.000000000000000000, 6.670939612111840944 ) ) ;
#40939 = EDGE_LOOP ( 'NONE', ( #25902, #4026, #13395, #15743 ) ) ;
#40940 = PLANE ( 'NONE',  #19499 ) ;
#40941 = EDGE_CURVE ( 'NONE', #37781, #30111, #332, .T. ) ;
#40942 = ORIENTED_EDGE ( 'NONE', *, *, #10407, .T. ) ;
#40943 = CARTESIAN_POINT ( 'NONE',  ( -18.58021353734938685, 1.419719901456505617, 3.853821158198948993 ) ) ;
#40944 = AXIS2_PLACEMENT_3D ( 'NONE', #38310, #43427, #38611 ) ;
#40945 = ORIENTED_EDGE ( 'NONE', *, *, #28292, .T. ) ;
#40946 = ORIENTED_EDGE ( 'NONE', *, *, #31371, .T. ) ;
#40947 = PLANE ( 'NONE',  #22943 ) ;
#40948 = CARTESIAN_POINT ( 'NONE',  ( -25.20278734466900517, 0.000000000000000000, 6.670939612111840944 ) ) ;
#40949 = CARTESIAN_POINT ( 'NONE',  ( -26.13415699229845757, -0.1191753592594197858, 6.933020519852192365 ) ) ;
#40950 = EDGE_CURVE ( 'NONE', #5490, #25102, #17673, .T. ) ;
#40951 = VERTEX_POINT ( 'NONE', #39 ) ;
#40952 = DIRECTION ( 'NONE',  ( 0.000000000000000000, 0.000000000000000000, -1.000000000000000000 ) ) ;
#40953 = VERTEX_POINT ( 'NONE', #52852 ) ;
#40954 = EDGE_CURVE ( 'NONE', #14910, #15700, #35013, .T. ) ;
#40955 = ADVANCED_FACE ( 'NONE', ( #31291 ), #48618, .F. ) ;
#40956 = EDGE_LOOP ( 'NONE', ( #2966, #48667, #45630, #26773 ) ) ;
#40957 = VERTEX_POINT ( 'NONE', #12845 ) ;
#40958 = CARTESIAN_POINT ( 'NONE',  ( -18.39746900504187010, 0.000000000000000000, 14.03700784672088808 ) ) ;
#40959 = VERTEX_POINT ( 'NONE', #30743 ) ;
#40960 = FACE_OUTER_BOUND ( 'NONE', #14233, .T. ) ;
#40961 = PRODUCT_DEFINITION_SHAPE ( 'NONE', 'NONE',  #18048 ) ;
#40962 = ADVANCED_FACE ( 'NONE', ( #48043 ), #4888, .F. ) ;
#40963 = EDGE_LOOP ( 'NONE', ( #42025, #11523, #39342, #40235 ) ) ;
#40964 = CARTESIAN_POINT ( 'NONE',  ( -19.05391333978853652, 0.000000000000000000, 4.672125166152008013 ) ) ;
#40965 = LINE ( 'NONE', #28184, #2288 ) ;
#40966 = VECTOR ( 'NONE', #44498, 1000.000000000000227 ) ;
#40967 = AXIS2_PLACEMENT_3D ( 'NONE', #21524, #55878, #12706 ) ;
#40968 = VERTEX_POINT ( 'NONE', #48307 ) ;
#40969 = EDGE_CURVE ( 'NONE', #3673, #44736, #9422, .T. ) ;
#40970 = CARTESIAN_POINT ( 'NONE',  ( -61.56892328330737740, 6.937430383826150404, -3.000000000000006661 ) ) ;
#40971 = ORIENTED_EDGE ( 'NONE', *, *, #26573, .T. ) ;
#40972 = EDGE_CURVE ( 'NONE', #16295, #6087, #43255, .T. ) ;
#40973 = DIRECTION ( 'NONE',  ( 0.5449076811759707706, 0.6444004775717708799, -0.5364919789714476250 ) ) ;
#40974 = CARTESIAN_POINT ( 'NONE',  ( -22.40556560354864146, -0.1191753592594197858, 5.484709000965211523 ) ) ;
#40975 = VECTOR ( 'NONE', #22831, 1000.000000000000227 ) ;
#40976 = DIRECTION ( 'NONE',  ( -0.5449076811759708816, 0.6444004775717707689, 0.5364919789714475140 ) ) ;
#40977 = FACE_OUTER_BOUND ( 'NONE', #12579, .T. ) ;
#40978 = CARTESIAN_POINT ( 'NONE',  ( -9.075990533167328067, 0.000000000000000000, 10.41622904950343909 ) ) ;
#40979 = CARTESIAN_POINT ( 'NONE',  ( -32.65997012216863737, 0.000000000000000000, 9.567562649885804404 ) ) ;
#40980 = ORIENTED_EDGE ( 'NONE', *, *, #544, .F. ) ;
#40981 = ADVANCED_FACE ( 'NONE', ( #42257 ), #11309, .F. ) ;
#40982 = ORIENTED_EDGE ( 'NONE', *, *, #44838, .T. ) ;
#40983 = FACE_OUTER_BOUND ( 'NONE', #2067, .T. ) ;
#40984 = CARTESIAN_POINT ( 'NONE',  ( -67.27849890436391433, -9.409707134521932304, 7.454917401049827141 ) ) ;
#40985 = VECTOR ( 'NONE', #54439, 999.9999999999998863 ) ;
#40986 = LINE ( 'NONE', #17529, #15795 ) ;
#40987 = VECTOR ( 'NONE', #40973, 1000.000000000000114 ) ;
#40988 = DIRECTION ( 'NONE',  ( 0.5364919789714477361, 0.6444004775717706579, 0.5449076811759711036 ) ) ;
#40989 = EDGE_CURVE ( 'NONE', #15522, #53467, #37414, .T. ) ;
#40990 = DIRECTION ( 'NONE',  ( 0.007781995580012663651, -3.146120232559066537E-19, -0.9999697198139514409 ) ) ;
#40991 = ORIENTED_EDGE ( 'NONE', *, *, #46205, .F. ) ;
#40992 = DIRECTION ( 'NONE',  ( -0.005002170337468016433, -0.7660444431189770143, 0.6427681459581293666 ) ) ;
#40993 = FACE_OUTER_BOUND ( 'NONE', #32111, .T. ) ;
#40994 = ORIENTED_EDGE ( 'NONE', *, *, #555, .T. ) ;
#40995 = FACE_OUTER_BOUND ( 'NONE', #41849, .T. ) ;
#40996 = DIRECTION ( 'NONE',  ( 0.9999697198139515519, 0.000000000000000000, 0.007781995580013368816 ) ) ;
#40997 = ORIENTED_EDGE ( 'NONE', *, *, #48403, .F. ) ;
#40998 = CARTESIAN_POINT ( 'NONE',  ( -70.38892378062969613, -1.000000000000148992, 7.852029984319922384 ) ) ;
#40999 = DIRECTION ( 'NONE',  ( 0.007781995580012662783, 0.000000000000000000, -0.9999697198139514409 ) ) ;
#41000 = LINE ( 'NONE', #11179, #27744 ) ;
#41001 = DIRECTION ( 'NONE',  ( -0.005961354470445682716, -0.6427876096865404731, 0.7660212471507180654 ) ) ;
#41002 = CARTESIAN_POINT ( 'NONE',  ( -9.110551994824897193, -1.000000000000000000, 3.538847790438064411 ) ) ;
#41003 = ORIENTED_EDGE ( 'NONE', *, *, #51275, .F. ) ;
#41004 = ORIENTED_EDGE ( 'NONE', *, *, #41298, .T. ) ;
#41005 = DIRECTION ( 'NONE',  ( 0.007781995580012663651, 0.000000000000000000, -0.9999697198139515519 ) ) ;
#41006 = DIRECTION ( 'NONE',  ( -0.7660212471507179544, -0.6427876096865405842, -0.005961354470445141482 ) ) ;
#41007 = CIRCLE ( 'NONE', #36599, 2.125000000000000000 ) ;
#41008 = LINE ( 'NONE', #31405, #34259 ) ;
#41009 = VECTOR ( 'NONE', #51766, 1000.000000000000227 ) ;
#41010 = AXIS2_PLACEMENT_3D ( 'NONE', #22444, #53626, #44836 ) ;
#41011 = CARTESIAN_POINT ( 'NONE',  ( -28.93137873341882127, 0.000000000000000000, 8.119251130998824451 ) ) ;
#41012 = DIRECTION ( 'NONE',  ( 0.5364919789714477361, 0.6444004775717706579, 0.5449076811759711036 ) ) ;
#41013 = EDGE_CURVE ( 'NONE', #5645, #40951, #24633, .T. ) ;
#41014 = EDGE_LOOP ( 'NONE', ( #30450, #20139, #11659, #51049 ) ) ;
#41015 = FACE_OUTER_BOUND ( 'NONE', #52381, .T. ) ;
#41016 = CARTESIAN_POINT ( 'NONE',  ( -50.02554558092695913, 3.776013638374815962, 5.000000000000000000 ) ) ;
#41017 = AXIS2_PLACEMENT_3D ( 'NONE', #34529, #4169, #35128 ) ;
#41018 = DIRECTION ( 'NONE',  ( -0.5364919789714478471, 0.6444004775717705469, -0.5449076811759709926 ) ) ;
#41019 = VECTOR ( 'NONE', #36378, 999.9999999999998863 ) ;
#41020 = VERTEX_POINT ( 'NONE', #28918 ) ;
#41021 = LINE ( 'NONE', #54101, #53736 ) ;
#41022 = ORIENTED_EDGE ( 'NONE', *, *, #4454, .T. ) ;
#41023 = DIRECTION ( 'NONE',  ( 0.007781995580012663651, 0.000000000000000000, -0.9999697198139515519 ) ) ;
#41024 = ADVANCED_FACE ( 'NONE', ( #7318 ), #50504, .F. ) ;
#41025 = DIRECTION ( 'NONE',  ( 0.000000000000000000, -1.000000000000000000, 0.000000000000000000 ) ) ;
#41026 = ORIENTED_EDGE ( 'NONE', *, *, #4952, .T. ) ;
#41027 = CARTESIAN_POINT ( 'NONE',  ( -20.93202838136840427, 2.553033558614008047, 4.731187272372491037 ) ) ;
#41028 =( GEOMETRIC_REPRESENTATION_CONTEXT ( 3 ) GLOBAL_UNCERTAINTY_ASSIGNED_CONTEXT ( ( #47265 ) ) GLOBAL_UNIT_ASSIGNED_CONTEXT ( ( #45508, #41273, #27102 ) ) REPRESENTATION_CONTEXT ( 'NONE', 'WORKASPACE' ) );
#41029 = VERTEX_POINT ( 'NONE', #2761 ) ;
#41030 = EDGE_CURVE ( 'NONE', #8484, #30283, #49912, .T. ) ;
#41031 = EDGE_LOOP ( 'NONE', ( #24221, #43034, #47056, #22758 ) ) ;
#41032 = VERTEX_POINT ( 'NONE', #37151 ) ;
#41033 = DIRECTION ( 'NONE',  ( -0.5364919789714478471, 0.6444004775717705469, -0.5449076811759709926 ) ) ;
#41034 = VERTEX_POINT ( 'NONE', #45960 ) ;
#41035 = ORIENTED_EDGE ( 'NONE', *, *, #27339, .F. ) ;
#41036 = LINE ( 'NONE', #1297, #32920 ) ;
#41037 = EDGE_LOOP ( 'NONE', ( #54951, #53555, #15066, #37642 ) ) ;
#41038 = ORIENTED_EDGE ( 'NONE', *, *, #47082, .T. ) ;
#41039 = DIRECTION ( 'NONE',  ( 0.000000000000000000, 0.000000000000000000, -1.000000000000000000 ) ) ;
#41040 = ADVANCED_FACE ( 'NONE', ( #28072 ), #3364, .F. ) ;
#41041 = EDGE_LOOP ( 'NONE', ( #28726, #52104, #24337, #461 ) ) ;
#41042 = VECTOR ( 'NONE', #50518, 1000.000000000000227 ) ;
#41043 = ORIENTED_EDGE ( 'NONE', *, *, #20888, .T. ) ;
#41044 = EDGE_CURVE ( 'NONE', #2953, #20314, #32881, .T. ) ;
#41045 = EDGE_LOOP ( 'NONE', ( #52389, #670, #8956, #2669 ) ) ;
#41046 = CARTESIAN_POINT ( 'NONE',  ( -16.73601541380021374, 1.419719901456506728, 5.712160089342227742 ) ) ;
#41047 = CARTESIAN_POINT ( 'NONE',  ( -6.110905869600904872, 1.712176620043476140E-14, 2.600000000000000089 ) ) ;
#41048 = CARTESIAN_POINT ( 'NONE',  ( -11.79352356370524646, 0.000000000000000000, 1.362631486225394761 ) ) ;
#41049 = LINE ( 'NONE', #40787, #9625 ) ;
#41050 = VECTOR ( 'NONE', #27329, 1000.000000000000227 ) ;
#41051 = ORIENTED_EDGE ( 'NONE', *, *, #45175, .F. ) ;
#41052 = CARTESIAN_POINT ( 'NONE',  ( -10.33808368536842970, -0.1191753592594177180, 6.317285075198634026 ) ) ;
#41053 = ORIENTED_EDGE ( 'NONE', *, *, #18991, .T. ) ;
#41054 = VECTOR ( 'NONE', #4504, 999.9999999999998863 ) ;
#41055 = ADVANCED_FACE ( 'NONE', ( #11016 ), #19555, .F. ) ;
#41056 = VECTOR ( 'NONE', #39045, 999.9999999999998863 ) ;
#41057 = ORIENTED_EDGE ( 'NONE', *, *, #39169, .T. ) ;
#41058 = FACE_OUTER_BOUND ( 'NONE', #45625, .T. ) ;
#41059 = CARTESIAN_POINT ( 'NONE',  ( 1.086233639165236964, 0.000000000000000000, 2.796443541562362078 ) ) ;
#41060 = VECTOR ( 'NONE', #7498, 999.9999999999998863 ) ;
#41061 = AXIS2_PLACEMENT_3D ( 'NONE', #37155, #54453, #2766 ) ;
#41062 = CARTESIAN_POINT ( 'NONE',  ( -12.56779750416103347, 0.000000000000000000, 7.138600094413515507 ) ) ;
#41063 = FACE_OUTER_BOUND ( 'NONE', #19097, .T. ) ;
#41064 = DIRECTION ( 'NONE',  ( -0.5449076811759708816, 0.6444004775717707689, 0.5364919789714475140 ) ) ;
#41065 = VERTEX_POINT ( 'NONE', #37725 ) ;
#41066 = PLANE ( 'NONE',  #23821 ) ;
#41067 = ORIENTED_EDGE ( 'NONE', *, *, #9982, .F. ) ;
#41068 = CARTESIAN_POINT ( 'NONE',  ( -27.99767448711536133, 0.000000000000000000, 7.557179307314289218 ) ) ;
#41069 = DIRECTION ( 'NONE',  ( 0.007781995580012662783, 0.000000000000000000, -0.9999697198139514409 ) ) ;
#41070 = CARTESIAN_POINT ( 'NONE',  ( -18.86354292863559579, 0.000000000000000000, 14.21804678658176080 ) ) ;
#41071 = VECTOR ( 'NONE', #47339, 999.9999999999998863 ) ;
#41072 = DIRECTION ( 'NONE',  ( 0.000000000000000000, 1.000000000000000000, 0.000000000000000000 ) ) ;
#41073 = AXIS2_PLACEMENT_3D ( 'NONE', #20909, #23322, #40639 ) ;
#41074 = LINE ( 'NONE', #36275, #32292 ) ;
#41075 = ORIENTED_EDGE ( 'NONE', *, *, #55532, .T. ) ;
#41076 = DIRECTION ( 'NONE',  ( -0.9999697198139514409, -0.000000000000000000, -0.007781995580013368816 ) ) ;
#41077 = LINE ( 'NONE', #24047, #22187 ) ;
#41078 = DIRECTION ( 'NONE',  ( 0.007781995580012663651, -3.146120232559066537E-19, -0.9999697198139514409 ) ) ;
#41079 = EDGE_CURVE ( 'NONE', #20591, #54534, #10764, .T. ) ;
#41080 = AXIS2_PLACEMENT_3D ( 'NONE', #44402, #31646, #26518 ) ;
#41081 = CARTESIAN_POINT ( 'NONE',  ( -9.758301349461536489, 0.000000000000000000, 4.375133698254432879 ) ) ;
#41082 = CARTESIAN_POINT ( 'NONE',  ( -17.42697428494509282, 0.000000000000000000, 8.747439149943453174 ) ) ;
#41083 = EDGE_CURVE ( 'NONE', #28433, #32707, #24366, .T. ) ;
#41084 = VECTOR ( 'NONE', #45214, 1000.000000000000000 ) ;
#41085 = LINE ( 'NONE', #33139, #43607 ) ;
#41086 = CARTESIAN_POINT ( 'NONE',  ( -27.13182803479460858, 16.99370762638562127, 4.657392947539033656 ) ) ;
#41087 = PLANE ( 'NONE',  #32392 ) ;
#41088 = EDGE_CURVE ( 'NONE', #5802, #20904, #6778, .T. ) ;
#41089 = VECTOR ( 'NONE', #30958, 999.9999999999998863 ) ;
#41090 = LINE ( 'NONE', #10156, #18358 ) ;
#41091 = EDGE_CURVE ( 'NONE', #5706, #661, #20384, .T. ) ;
#41092 = EDGE_CURVE ( 'NONE', #11344, #4466, #19830, .T. ) ;
#41093 = ADVANCED_FACE ( 'NONE', ( #46489 ), #15551, .F. ) ;
#41094 = VECTOR ( 'NONE', #7157, 1000.000000000000227 ) ;
#41095 = VECTOR ( 'NONE', #14603, 1000.000000000000000 ) ;
#41096 = EDGE_LOOP ( 'NONE', ( #18061, #28871, #42944, #46717, #47236 ) ) ;
#41097 = VECTOR ( 'NONE', #4855, 999.9999999999998863 ) ;
#41098 = ORIENTED_EDGE ( 'NONE', *, *, #33018, .F. ) ;
#41099 = ORIENTED_EDGE ( 'NONE', *, *, #12120, .F. ) ;
#41100 = AXIS2_PLACEMENT_3D ( 'NONE', #23612, #31306, #10280 ) ;
#41101 = ORIENTED_EDGE ( 'NONE', *, *, #15688, .F. ) ;
#41102 = ORIENTED_EDGE ( 'NONE', *, *, #17979, .T. ) ;
#41103 = DIRECTION ( 'NONE',  ( 0.5364919789714477361, 0.6444004775717706579, 0.5449076811759711036 ) ) ;
#41104 = CARTESIAN_POINT ( 'NONE',  ( -11.22056963685719211, 0.000000000000000000, 1.239771416285661010 ) ) ;
#41105 = EDGE_LOOP ( 'NONE', ( #31473, #36277, #36698, #81 ) ) ;
#41106 = ORIENTED_EDGE ( 'NONE', *, *, #40097, .T. ) ;
#41107 = ADVANCED_FACE ( 'NONE', ( #50200 ), #20086, .F. ) ;
#41108 = VERTEX_POINT ( 'NONE', #52927 ) ;
#41109 = AXIS2_PLACEMENT_3D ( 'NONE', #37910, #2424, #15746 ) ;
#41110 = ORIENTED_EDGE ( 'NONE', *, *, #28830, .T. ) ;
#41111 = EDGE_CURVE ( 'NONE', #3615, #8086, #1789, .T. ) ;
#41112 = CARTESIAN_POINT ( 'NONE',  ( -67.82503658922976797, -9.472380908384517184, -6.792143739504113320 ) ) ;
#41113 = EDGE_CURVE ( 'NONE', #46706, #13860, #34776, .T. ) ;
#41114 = CARTESIAN_POINT ( 'NONE',  ( -32.65919192261063841, -0.1191753592594197858, 9.467565677904410393 ) ) ;
#41115 = PLANE ( 'NONE',  #44058 ) ;
#41116 = ORIENTED_EDGE ( 'NONE', *, *, #48385, .F. ) ;
#41117 = DIRECTION ( 'NONE',  ( -0.6246952433987893460, -0.7422098413412802076, 0.2426528472758542054 ) ) ;
#41118 = VECTOR ( 'NONE', #37991, 999.9999999999998863 ) ;
#41119 = EDGE_CURVE ( 'NONE', #56078, #42377, #36441, .T. ) ;
#41120 = CARTESIAN_POINT ( 'NONE',  ( -10.00813838035478298, 0.000000000000000000, 10.77830692922518452 ) ) ;
#41122 = VECTOR ( 'NONE', #35046, 1000.000000000000227 ) ;
#41121 = CARTESIAN_POINT ( 'NONE',  ( -13.23242834496490872, 0.000000000000000000, 7.133427783529502797 ) ) ;
#41123 = EDGE_CURVE ( 'NONE', #49125, #8091, #49523, .T. ) ;
#41124 = CARTESIAN_POINT ( 'NONE',  ( -16.81345671998191449, 0.000000000000000000, 3.412238694616132495 ) ) ;
#41125 = DIRECTION ( 'NONE',  ( -0.005961354470445682716, -0.6427876096865404731, 0.7660212471507180654 ) ) ;
#41126 = LINE ( 'NONE', #49667, #9520 ) ;
#41127 = CARTESIAN_POINT ( 'NONE',  ( -11.87243407472968926, 0.000000000000000000, 11.50246268866867361 ) ) ;
#41128 = CARTESIAN_POINT ( 'NONE',  ( -14.66887761629205222, 0.000000000000000000, 12.58869632783390990 ) ) ;
#41129 = VECTOR ( 'NONE', #28526, 1000.000000000000114 ) ;
#41130 = DIRECTION ( 'NONE',  ( -0.005961354470445682716, -0.6427876096865404731, 0.7660212471507180654 ) ) ;
#41131 = ORIENTED_EDGE ( 'NONE', *, *, #1013, .F. ) ;
#41132 = LINE ( 'NONE', #11311, #44700 ) ;
#41133 = VERTEX_POINT ( 'NONE', #32199 ) ;
#41134 = VECTOR ( 'NONE', #9796, 1000.000000000000227 ) ;
#41135 = VECTOR ( 'NONE', #43560, 1000.000000000000227 ) ;
#41136 = CARTESIAN_POINT ( 'NONE',  ( -14.93495759592298988, 0.000000000000000000, 12.77129166681078409 ) ) ;
#41137 = CARTESIAN_POINT ( 'NONE',  ( -12.55917534364518495, 0.000000000000000000, 6.030670984640223331 ) ) ;
#41138 = LINE ( 'NONE', #3567, #39470 ) ;
#41139 = PLANE ( 'NONE',  #25050 ) ;
#41140 = DIRECTION ( 'NONE',  ( 0.6246952433987894571, -0.7422098413412800966, -0.2426528472758541777 ) ) ;
#41141 = DIRECTION ( 'NONE',  ( 0.007781995580012663651, -3.146120232559066537E-19, -0.9999697198139514409 ) ) ;
#41142 = VECTOR ( 'NONE', #52039, 1000.000000000000000 ) ;
#41143 = CARTESIAN_POINT ( 'NONE',  ( 0.09621548157177266247, -1.683565401097097070, -3.964956190634384326E-16 ) ) ;
#41144 = AXIS2_PLACEMENT_3D ( 'NONE', #26093, #20698, #3639 ) ;
#41145 = DIRECTION ( 'NONE',  ( 1.000000000000000000, 0.000000000000000000, 0.000000000000000000 ) ) ;
#41146 = DIRECTION ( 'NONE',  ( -0.9999697198139514409, -0.000000000000000000, -0.007781995580013368816 ) ) ;
#41147 = PLANE ( 'NONE',  #39326 ) ;
#41148 = LINE ( 'NONE', #32080, #47607 ) ;
#41149 = PLANE ( 'NONE',  #50866 ) ;
#41150 = PLANE ( 'NONE',  #11475 ) ;
#41151 = DIRECTION ( 'NONE',  ( 0.9999697198139515519, 0.000000000000000000, 0.007781995580013368816 ) ) ;
#41152 = DIRECTION ( 'NONE',  ( -0.005002170337468016433, -0.7660444431189770143, 0.6427681459581293666 ) ) ;
#41153 = FACE_OUTER_BOUND ( 'NONE', #38294, .T. ) ;
#41154 = CARTESIAN_POINT ( 'NONE',  ( -22.40634380310664397, 0.000000000000000000, 5.584705972946605534 ) ) ;
#41155 = ORIENTED_EDGE ( 'NONE', *, *, #35861, .F. ) ;
#41156 = CARTESIAN_POINT ( 'NONE',  ( -11.77243710274829525, -0.1191753592594197858, 11.50324088822667612 ) ) ;
#41157 = ORIENTED_EDGE ( 'NONE', *, *, #21705, .T. ) ;
#41158 = AXIS2_PLACEMENT_3D ( 'NONE', #52373, #42999, #30225 ) ;
#41159 = DIRECTION ( 'NONE',  ( 0.007781995580012663651, -3.146120232559066537E-19, -0.9999697198139514409 ) ) ;
#41160 = DIRECTION ( 'NONE',  ( -0.7660212471507179544, -0.6427876096865405842, -0.005961354470445141482 ) ) ;
#41161 = AXIS2_PLACEMENT_3D ( 'NONE', #32048, #45125, #18727 ) ;
#41162 = ADVANCED_FACE ( 'NONE', ( #1537 ), #6102, .F. ) ;
#41163 = EDGE_CURVE ( 'NONE', #37134, #45757, #10046, .T. ) ;
#41164 = ORIENTED_EDGE ( 'NONE', *, *, #2743, .T. ) ;
#41165 = DIRECTION ( 'NONE',  ( -0.000000000000000000, -1.000000000000000000, 0.000000000000000000 ) ) ;
#41166 = AXIS2_PLACEMENT_3D ( 'NONE', #46799, #11308, #32880 ) ;
#41167 = VERTEX_POINT ( 'NONE', #40145 ) ;
#41168 = DIRECTION ( 'NONE',  ( -0.005002170337468016433, -0.7660444431189770143, 0.6427681459581293666 ) ) ;
#41169 = EDGE_CURVE ( 'NONE', #33959, #18846, #40449, .T. ) ;
#41170 = ORIENTED_EDGE ( 'NONE', *, *, #40589, .T. ) ;
#41171 = ORIENTED_EDGE ( 'NONE', *, *, #49205, .T. ) ;
#41172 = EDGE_LOOP ( 'NONE', ( #49658, #50439, #17340, #44327 ) ) ;
#41173 = CARTESIAN_POINT ( 'NONE',  ( -23.23471500290295921, 19.24370688441070953, -4.657437592157546824 ) ) ;
#41174 = VECTOR ( 'NONE', #50862, 1000.000000000000227 ) ;
#41175 = DIRECTION ( 'NONE',  ( 0.000000000000000000, -1.000000000000000000, 0.000000000000000000 ) ) ;
#41176 = DIRECTION ( 'NONE',  ( 0.9999697198139515519, 0.000000000000000000, 0.007781995580013368816 ) ) ;
#41177 = AXIS2_PLACEMENT_3D ( 'NONE', #43439, #38056, #8825 ) ;
#41178 = VERTEX_POINT ( 'NONE', #22825 ) ;
#41179 = ORIENTED_EDGE ( 'NONE', *, *, #42511, .T. ) ;
#41180 = VECTOR ( 'NONE', #36854, 1000.000000000000000 ) ;
#41181 = VECTOR ( 'NONE', #10729, 1000.000000000000114 ) ;
#41182 = DIRECTION ( 'NONE',  ( 0.007781995580012663651, -3.146120232559066537E-19, -0.9999697198139514409 ) ) ;
#41183 = ORIENTED_EDGE ( 'NONE', *, *, #30299, .F. ) ;
#41184 = DIRECTION ( 'NONE',  ( -0.005961354470445682716, -0.6427876096865404731, 0.7660212471507180654 ) ) ;
#41185 = ORIENTED_EDGE ( 'NONE', *, *, #43247, .T. ) ;
#41186 = CARTESIAN_POINT ( 'NONE',  ( -28.93137873341882127, 0.000000000000000000, 8.119251130998824451 ) ) ;
#41187 = DIRECTION ( 'NONE',  ( 0.007781995580012663651, -3.146120232559066537E-19, -0.9999697198139514409 ) ) ;
#41188 = EDGE_LOOP ( 'NONE', ( #37289, #9151, #47370 ) ) ;
#41189 = LINE ( 'NONE', #20734, #26415 ) ;
#41190 = EDGE_CURVE ( 'NONE', #47896, #33095, #26819, .T. ) ;
#41191 = AXIS2_PLACEMENT_3D ( 'NONE', #23583, #6013, #10815 ) ;
#41192 = DIRECTION ( 'NONE',  ( -0.6427681459581293666, -0.7660444431189770143, -0.005002170337467561935 ) ) ;
#41194 = ADVANCED_FACE ( 'NONE', ( #13741 ), #1234, .F. ) ;
#41193 = VERTEX_POINT ( 'NONE', #53489 ) ;
#41195 = FACE_OUTER_BOUND ( 'NONE', #26296, .T. ) ;
#41196 = LINE ( 'NONE', #41734, #32109 ) ;
#41197 = DIRECTION ( 'NONE',  ( -0.6427681459581293666, -0.7660444431189770143, -0.005002170337467561935 ) ) ;
#41198 = EDGE_CURVE ( 'NONE', #49377, #8607, #36185, .T. ) ;
#41199 = ORIENTED_EDGE ( 'NONE', *, *, #7927, .T. ) ;
#41200 = AXIS2_PLACEMENT_3D ( 'NONE', #29709, #43020, #17445 ) ;
#41201 = LINE ( 'NONE', #28135, #55527 ) ;
#41202 = DIRECTION ( 'NONE',  ( 0.007781995580012662783, 0.000000000000000000, -0.9999697198139514409 ) ) ;
#41203 = EDGE_CURVE ( 'NONE', #5052, #39740, #27100, .T. ) ;
#41204 = CARTESIAN_POINT ( 'NONE',  ( -10.79697247519895420, -0.1191753592594185784, 5.575049756915096744 ) ) ;
#41205 = CARTESIAN_POINT ( 'NONE',  ( -12.15116108492864377, 0.000000000000000000, 1.401855352044617975 ) ) ;
#41206 = CARTESIAN_POINT ( 'NONE',  ( -23.66772770479517618, 18.99370688441070953, 4.503109509781816122 ) ) ;
#41207 = LINE ( 'NONE', #45734, #12495 ) ;
#41208 = CARTESIAN_POINT ( 'NONE',  ( -9.808144436391993182, 0.000000000000000000, 10.77986332834118777 ) ) ;
#41209 = AXIS2_PLACEMENT_3D ( 'NONE', #29112, #37650, #25420 ) ;
#41210 = VERTEX_POINT ( 'NONE', #35339 ) ;
#41211 = CARTESIAN_POINT ( 'NONE',  ( -16.89925026227929195, -0.1191753592594197858, 13.49466922669627422 ) ) ;
#41212 = LINE ( 'NONE', #36973, #31400 ) ;
#41213 = CARTESIAN_POINT ( 'NONE',  ( -68.53751928918664760, 4.336808689942017736E-15, -8.456585623303165988 ) ) ;
#41214 = ORIENTED_EDGE ( 'NONE', *, *, #35393, .F. ) ;
#41215 = VECTOR ( 'NONE', #31188, 1000.000000000000227 ) ;
#41216 = PLANE ( 'NONE',  #15668 ) ;
#41217 = DIRECTION ( 'NONE',  ( -0.5449076811759708816, 0.6444004775717707689, 0.5364919789714475140 ) ) ;
#41218 = VECTOR ( 'NONE', #49911, 999.9999999999998863 ) ;
#41219 = CARTESIAN_POINT ( 'NONE',  ( -9.542064456761055524, 0.000000000000000000, 10.59726798936431180 ) ) ;
#41220 = DIRECTION ( 'NONE',  ( 0.9997703818010067467, -0.000000000000000000, -0.02142857142857158143 ) ) ;
#41221 = CARTESIAN_POINT ( 'NONE',  ( -55.63114022126601554, 6.713117369705148718, 1.409618983554703719 ) ) ;
#41222 = ORIENTED_EDGE ( 'NONE', *, *, #44122, .F. ) ;
#41223 = AXIS2_PLACEMENT_3D ( 'NONE', #39348, #4702, #437 ) ;
#41224 = VECTOR ( 'NONE', #31017, 999.9999999999998863 ) ;
#41225 = EDGE_LOOP ( 'NONE', ( #5205, #23172, #26970, #33313 ) ) ;
#41226 = FACE_OUTER_BOUND ( 'NONE', #21579, .T. ) ;
#41227 = CARTESIAN_POINT ( 'NONE',  ( -24.54687786003638550, 18.44472464513734522, -4.546935035528026248 ) ) ;
#41228 = EDGE_CURVE ( 'NONE', #11807, #8966, #48386, .T. ) ;
#41229 = VERTEX_POINT ( 'NONE', #23402 ) ;
#41230 = DIRECTION ( 'NONE',  ( 0.007781995580012663651, 0.000000000000000000, -0.9999697198139515519 ) ) ;
#41231 = ORIENTED_EDGE ( 'NONE', *, *, #7980, .T. ) ;
#41232 = LINE ( 'NONE', #23906, #19274 ) ;
#41233 = EDGE_CURVE ( 'NONE', #9162, #48014, #52639, .T. ) ;
#41234 = EDGE_CURVE ( 'NONE', #19170, #8089, #31648, .T. ) ;
#41235 = VECTOR ( 'NONE', #19503, 999.9999999999998863 ) ;
#41236 = EDGE_LOOP ( 'NONE', ( #16040, #32936, #26295, #37080 ) ) ;
#41237 = ORIENTED_EDGE ( 'NONE', *, *, #54619, .T. ) ;
#41238 = VECTOR ( 'NONE', #49964, 1000.000000000000000 ) ;
#41239 = CARTESIAN_POINT ( 'NONE',  ( -17.46397131646373779, 3.362543313726509719, 9.183427090828809369 ) ) ;
#41240 = CARTESIAN_POINT ( 'NONE',  ( -14.66887761629205222, 0.000000000000000000, 12.58869632783390990 ) ) ;
#41241 = AXIS2_PLACEMENT_3D ( 'NONE', #21381, #30473, #30170 ) ;
#41242 = DIRECTION ( 'NONE',  ( 0.005961354470445682716, -0.6427876096865404731, -0.7660212471507180654 ) ) ;
#41243 = VERTEX_POINT ( 'NONE', #18018 ) ;
#41244 = DIRECTION ( 'NONE',  ( 0.5364919789714477361, 0.6444004775717706579, 0.5449076811759711036 ) ) ;
#41245 = AXIS2_PLACEMENT_3D ( 'NONE', #36665, #3422, #55650 ) ;
#41246 = ORIENTED_EDGE ( 'NONE', *, *, #19176, .T. ) ;
#41247 = EDGE_CURVE ( 'NONE', #3660, #41644, #44146, .T. ) ;
#41248 = ORIENTED_EDGE ( 'NONE', *, *, #29596, .T. ) ;
#41249 = ORIENTED_EDGE ( 'NONE', *, *, #25328, .F. ) ;
#41250 = AXIS2_PLACEMENT_3D ( 'NONE', #15162, #5790, #49214 ) ;
#41251 = LINE ( 'NONE', #50023, #35894 ) ;
#41252 = AXIS2_PLACEMENT_3D ( 'NONE', #28492, #2073, #2375 ) ;
#41253 = VERTEX_POINT ( 'NONE', #22562 ) ;
#41254 = AXIS2_PLACEMENT_3D ( 'NONE', #20302, #12057, #29394 ) ;
#41255 = VECTOR ( 'NONE', #52694, 1000.000000000000227 ) ;
#41256 = PLANE ( 'NONE',  #48413 ) ;
#41257 = MANIFOLD_SOLID_BREP ( 'Fillet5', #13160 ) ;
#41258 = ORIENTED_EDGE ( 'NONE', *, *, #38818, .T. ) ;
#41259 = LINE ( 'NONE', #44975, #46723 ) ;
#41260 = PLANE ( 'NONE',  #15915 ) ;
#41261 = VECTOR ( 'NONE', #15361, 999.9999999999998863 ) ;
#41262 = ORIENTED_EDGE ( 'NONE', *, *, #34292, .F. ) ;
#41263 = FACE_OUTER_BOUND ( 'NONE', #46109, .T. ) ;
#41264 = ORIENTED_EDGE ( 'NONE', *, *, #5579, .T. ) ;
#41265 = CIRCLE ( 'NONE', #43971, 6.999999999999999112 ) ;
#41266 = CARTESIAN_POINT ( 'NONE',  ( -19.61438316718806973, -0.1166911823299058987, 4.400518953728226990 ) ) ;
#41267 = VECTOR ( 'NONE', #21157, 1000.000000000000000 ) ;
#41268 = CARTESIAN_POINT ( 'NONE',  ( -11.14243809316658052, -10.74105472484483670, 1.109727778512525687 ) ) ;
#41269 = CARTESIAN_POINT ( 'NONE',  ( -11.20636620717317378, 0.000000000000000000, 11.32298014792380414 ) ) ;
#41270 = DIRECTION ( 'NONE',  ( 0.9999697198139515519, 0.000000000000000000, 0.007781995580013368816 ) ) ;
#41271 = PLANE ( 'NONE',  #12381 ) ;
#41272 = LINE ( 'NONE', #489, #4700 ) ;
#41273 =( NAMED_UNIT ( * ) PLANE_ANGLE_UNIT ( ) SI_UNIT ( $, .RADIAN. ) );
#41274 = EDGE_LOOP ( 'NONE', ( #29152, #42901, #34026, #13332 ) ) ;
#41275 = EDGE_LOOP ( 'NONE', ( #16494, #15946, #2957, #19777 ) ) ;
#41276 = LINE ( 'NONE', #41553, #37324 ) ;
#41277 = ADVANCED_FACE ( 'NONE', ( #24776 ), #39872, .F. ) ;
#41278 = DIRECTION ( 'NONE',  ( 0.000000000000000000, -1.000000000000000000, 0.000000000000000000 ) ) ;
#41279 = LINE ( 'NONE', #10891, #4050 ) ;
#41280 = DIRECTION ( 'NONE',  ( -0.7660212471507179544, -0.6427876096865405842, -0.005961354470445141482 ) ) ;
#41281 = VECTOR ( 'NONE', #43343, 1000.000000000000227 ) ;
#41282 = DIRECTION ( 'NONE',  ( -1.000000000000000000, 0.000000000000000000, 0.000000000000000000 ) ) ;
#41283 = ORIENTED_EDGE ( 'NONE', *, *, #15032, .F. ) ;
#41284 = VECTOR ( 'NONE', #21772, 1000.000000000000227 ) ;
#41285 = DIRECTION ( 'NONE',  ( 0.007781995580012662783, 0.000000000000000000, -0.9999697198139514409 ) ) ;
#41286 = CARTESIAN_POINT ( 'NONE',  ( -22.40634380310664397, 0.000000000000000000, 5.584705972946605534 ) ) ;
#41287 = ORIENTED_EDGE ( 'NONE', *, *, #5860, .T. ) ;
#41288 = LINE ( 'NONE', #36456, #55602 ) ;
#41289 = DIRECTION ( 'NONE',  ( 0.9999697198139515519, 0.000000000000000000, 0.007781995580013368816 ) ) ;
#41290 = VECTOR ( 'NONE', #26537, 1000.000000000000114 ) ;
#41291 = VERTEX_POINT ( 'NONE', #23939 ) ;
#41292 = EDGE_CURVE ( 'NONE', #37937, #53290, #29037, .T. ) ;
#41293 = CARTESIAN_POINT ( 'NONE',  ( -71.01620612404938981, -1.000000000000001332, -8.550077602493738382 ) ) ;
#41294 = DIRECTION ( 'NONE',  ( 0.7660212471507180654, -0.6427876096865404731, 0.005961354470445141482 ) ) ;
#41295 = VECTOR ( 'NONE', #19257, 1000.000000000000227 ) ;
#41296 = CARTESIAN_POINT ( 'NONE',  ( -13.94865558154716112, 0.000000000000000000, 5.450519602115640794 ) ) ;
#41297 = EDGE_CURVE ( 'NONE', #43180, #43341, #46082, .T. ) ;
#41298 = EDGE_CURVE ( 'NONE', #39217, #39457, #42091, .T. ) ;
#41299 = FACE_OUTER_BOUND ( 'NONE', #32447, .T. ) ;
#41300 = ORIENTED_EDGE ( 'NONE', *, *, #30659, .T. ) ;
#41301 = VECTOR ( 'NONE', #44336, 999.9999999999998863 ) ;
#41302 = VECTOR ( 'NONE', #21606, 999.9999999999998863 ) ;
#41303 = ORIENTED_EDGE ( 'NONE', *, *, #17724, .F. ) ;
#41304 = DIRECTION ( 'NONE',  ( 0.9999697198139515519, 0.000000000000000000, 0.007781995580013368816 ) ) ;
#41305 = CARTESIAN_POINT ( 'NONE',  ( -12.23851102634202448, -0.1191753592594197858, 11.68427982808754884 ) ) ;
#41306 = CARTESIAN_POINT ( 'NONE',  ( -20.26176469941677993, 0.000000000000000000, 14.76116360616437895 ) ) ;
#41307 = EDGE_CURVE ( 'NONE', #42825, #10301, #45799, .T. ) ;
#41308 = VECTOR ( 'NONE', #30331, 1000.000000000000000 ) ;
#41309 = CARTESIAN_POINT ( 'NONE',  ( -23.66772770479517618, 18.99370688441070953, -4.657437592157546824 ) ) ;
#41311 = DIRECTION ( 'NONE',  ( -0.5364919789714478471, 0.6444004775717705469, -0.5449076811759709926 ) ) ;
#41310 = VECTOR ( 'NONE', #28762, 1000.000000000000114 ) ;
#41312 = EDGE_CURVE ( 'NONE', #35388, #48977, #54319, .T. ) ;
#41313 = DIRECTION ( 'NONE',  ( 0.9999697198139515519, 0.000000000000000000, 0.007781995580013368816 ) ) ;
#41314 = ORIENTED_EDGE ( 'NONE', *, *, #44317, .T. ) ;
#41315 = CARTESIAN_POINT ( 'NONE',  ( -21.47419595591918906, 0.000000000000000000, 5.222628093224860102 ) ) ;
#41316 = ADVANCED_FACE ( 'NONE', ( #2361 ), #11721, .F. ) ;
#41317 = VECTOR ( 'NONE', #12883, 1000.000000000000227 ) ;
#41318 = DIRECTION ( 'NONE',  ( 0.7660212471507180654, -0.6427876096865404731, 0.005961354470445141482 ) ) ;
#41319 = VECTOR ( 'NONE', #30047, 999.9999999999998863 ) ;
#41320 = CARTESIAN_POINT ( 'NONE',  ( -20.44406847140967187, 20.85488741058141571, -4.316516078624408337 ) ) ;
#41321 = ORIENTED_EDGE ( 'NONE', *, *, #51283, .T. ) ;
#41322 = CARTESIAN_POINT ( 'NONE',  ( -10.74029228357944987, 0.000000000000000000, 11.14194120806293320 ) ) ;
#41323 = CARTESIAN_POINT ( 'NONE',  ( -12.60458797795435615, 0.000000000000000000, 11.86609696750642229 ) ) ;
#41324 = CARTESIAN_POINT ( 'NONE',  ( -16.83725213413307031, -0.1191753592594191197, 5.528042903930973750 ) ) ;
#41325 = ADVANCED_FACE ( 'NONE', ( #37019 ), #50883, .F. ) ;
#41326 = ORIENTED_EDGE ( 'NONE', *, *, #4209, .F. ) ;
#41327 = DIRECTION ( 'NONE',  ( 0.007781995580012662783, 0.000000000000000000, -0.9999697198139514409 ) ) ;
#41328 = ORIENTED_EDGE ( 'NONE', *, *, #50258, .F. ) ;
#41329 = VECTOR ( 'NONE', #38738, 999.9999999999998863 ) ;
#41330 = ADVANCED_FACE ( 'NONE', ( #32485 ), #19952, .F. ) ;
#41331 = VERTEX_POINT ( 'NONE', #7188 ) ;
#41332 = VERTEX_POINT ( 'NONE', #24488 ) ;
#41333 = EDGE_LOOP ( 'NONE', ( #6877, #52010, #38083, #38997 ) ) ;
#41334 = AXIS2_PLACEMENT_3D ( 'NONE', #48002, #5987, #14493 ) ;
#41335 = EDGE_LOOP ( 'NONE', ( #18300, #41688, #55418, #49076 ) ) ;
#41336 = CARTESIAN_POINT ( 'NONE',  ( -23.33693525117809386, 0.000000000000000000, 5.746789908705562944 ) ) ;
#41337 = AXIS2_PLACEMENT_3D ( 'NONE', #20932, #12457, #30034 ) ;
#41338 = VERTEX_POINT ( 'NONE', #37271 ) ;
#41339 = ORIENTED_EDGE ( 'NONE', *, *, #30736, .T. ) ;
#41340 = FACE_OUTER_BOUND ( 'NONE', #32470, .T. ) ;
#41341 = ORIENTED_EDGE ( 'NONE', *, *, #41669, .T. ) ;
#41342 = AXIS2_PLACEMENT_3D ( 'NONE', #17057, #55962, #21007 ) ;
#41343 = ORIENTED_EDGE ( 'NONE', *, *, #45917, .T. ) ;
#41344 = EDGE_LOOP ( 'NONE', ( #11653, #32264, #3097, #18413 ) ) ;
#41345 = DIRECTION ( 'NONE',  ( -0.5364919789714478471, 0.6444004775717705469, -0.5449076811759709926 ) ) ;
#41346 = CARTESIAN_POINT ( 'NONE',  ( -18.67619601524082285, 0.000000000000000000, 3.936400510096834893 ) ) ;
#41347 = LINE ( 'NONE', #37338, #10559 ) ;
#41348 = DIRECTION ( 'NONE',  ( -0.9999697198139514409, -0.000000000000000000, -0.007781995580013368816 ) ) ;
#41349 = VECTOR ( 'NONE', #18089, 1000.000000000000114 ) ;
#41350 = ORIENTED_EDGE ( 'NONE', *, *, #48541, .F. ) ;
#41351 = FACE_OUTER_BOUND ( 'NONE', #44390, .T. ) ;
#41352 = ORIENTED_EDGE ( 'NONE', *, *, #48568, .F. ) ;
#41353 = AXIS2_PLACEMENT_3D ( 'NONE', #13378, #46660, #55187 ) ;
#41354 = ORIENTED_EDGE ( 'NONE', *, *, #26987, .T. ) ;
#41355 = AXIS2_PLACEMENT_3D ( 'NONE', #10479, #22428, #40283 ) ;
#41356 = CARTESIAN_POINT ( 'NONE',  ( -18.07819366188567400, 3.038739411681509850, 3.607164391028207628 ) ) ;
#41357 = EDGE_CURVE ( 'NONE', #5052, #22227, #33022, .T. ) ;
#41358 = PLANE ( 'NONE',  #14906 ) ;
#41359 = AXIS2_PLACEMENT_3D ( 'NONE', #24146, #23574, #23318 ) ;
#41360 = CARTESIAN_POINT ( 'NONE',  ( -28.92727693918987342, 15.95710471811680264, -4.722836279463598075 ) ) ;
#41361 = VECTOR ( 'NONE', #25715, 1000.000000000000000 ) ;
#41362 = DIRECTION ( 'NONE',  ( -0.3620778797217461542, -0.000000000000000000, -0.9321478471874538041 ) ) ;
#41363 = CARTESIAN_POINT ( 'NONE',  ( 4.848100717410754434, 0.000000000000000000, -2.061810099490656079 ) ) ;
#41364 = CARTESIAN_POINT ( 'NONE',  ( -11.70900194784942805, -0.1191753592594185784, 3.351959713832490362 ) ) ;
#41365 = ORIENTED_EDGE ( 'NONE', *, *, #51624, .T. ) ;
#41366 = CARTESIAN_POINT ( 'NONE',  ( -24.27063949748155380, 0.000000000000000000, 6.308861732390097288 ) ) ;
#41367 = ORIENTED_EDGE ( 'NONE', *, *, #17618, .T. ) ;
#41368 = EDGE_CURVE ( 'NONE', #49949, #33064, #2896, .T. ) ;
#41369 = CARTESIAN_POINT ( 'NONE',  ( -9.542064456761055524, 0.000000000000000000, 10.59726798936431180 ) ) ;
#41370 = FACE_OUTER_BOUND ( 'NONE', #49813, .T. ) ;
#41371 = DIRECTION ( 'NONE',  ( 0.007781995580012663651, 0.000000000000000000, -0.9999697198139515519 ) ) ;
#41372 = PLANE ( 'NONE',  #29518 ) ;
#41373 = EDGE_CURVE ( 'NONE', #42922, #13439, #50628, .T. ) ;
#41374 = CARTESIAN_POINT ( 'NONE',  ( -15.99857495235844418, 0.000000000000000000, 4.326570446154306637 ) ) ;
#41375 = AXIS2_PLACEMENT_3D ( 'NONE', #3585, #19593, #4165 ) ;
#41376 = ORIENTED_EDGE ( 'NONE', *, *, #31629, .F. ) ;
#41377 = LINE ( 'NONE', #2166, #41181 ) ;
#41378 = CARTESIAN_POINT ( 'NONE',  ( -11.35508003745286310, 0.000000000000000000, 4.732039267092165602 ) ) ;
#41379 = LINE ( 'NONE', #23229, #14612 ) ;
#41380 = AXIS2_PLACEMENT_3D ( 'NONE', #35933, #35626, #13756 ) ;
#41381 = CARTESIAN_POINT ( 'NONE',  ( -15.05936134377114044, 0.000000000000000000, 3.056557400622056608 ) ) ;
#41382 = ADVANCED_FACE ( 'NONE', ( #40977 ), #2062, .F. ) ;
#41383 = FACE_OUTER_BOUND ( 'NONE', #46131, .T. ) ;
#41384 = DIRECTION ( 'NONE',  ( -0.005961354470445682716, -0.6427876096865404731, 0.7660212471507180654 ) ) ;
#41385 = LINE ( 'NONE', #49882, #14754 ) ;
#41386 = EDGE_CURVE ( 'NONE', #41034, #4870, #25616, .T. ) ;
#41387 = AXIS2_PLACEMENT_3D ( 'NONE', #30100, #4288, #22449 ) ;
#41388 = CARTESIAN_POINT ( 'NONE',  ( -70.57153585115312922, -8.780779913117140012, -8.550077602493740159 ) ) ;
#41389 = DIRECTION ( 'NONE',  ( 0.005961354470445682716, -0.6427876096865404731, -0.7660212471507180654 ) ) ;
#41390 = VECTOR ( 'NONE', #14485, 1000.000000000000227 ) ;
#41391 = EDGE_CURVE ( 'NONE', #27257, #41560, #8891, .T. ) ;
#41392 = ORIENTED_EDGE ( 'NONE', *, *, #49306, .T. ) ;
#41393 = AXIS2_PLACEMENT_3D ( 'NONE', #27101, #5256, #52092 ) ;
#41394 = VECTOR ( 'NONE', #33154, 1000.000000000000227 ) ;
#41395 = EDGE_CURVE ( 'NONE', #3168, #7513, #55429, .T. ) ;
#41396 = VERTEX_POINT ( 'NONE', #51180 ) ;
#41397 = VECTOR ( 'NONE', #48332, 1000.000000000000227 ) ;
#41398 = ORIENTED_EDGE ( 'NONE', *, *, #22648, .T. ) ;
#41399 = ORIENTED_EDGE ( 'NONE', *, *, #28749, .T. ) ;
#41400 = ORIENTED_EDGE ( 'NONE', *, *, #53243, .F. ) ;
#41401 = CARTESIAN_POINT ( 'NONE',  ( -10.84028925556084388, -0.1191753592594197858, 11.14116300850493246 ) ) ;
#41402 = DIRECTION ( 'NONE',  ( -0.7660212471507179544, -0.6427876096865405842, -0.005961354470445141482 ) ) ;
#41403 = ORIENTED_EDGE ( 'NONE', *, *, #52598, .T. ) ;
#41404 = CARTESIAN_POINT ( 'NONE',  ( -16.75880829507524439, 3.686347215771511365, 3.074008228493816386 ) ) ;
#41405 = ORIENTED_EDGE ( 'NONE', *, *, #22722, .F. ) ;
#41406 = ORIENTED_EDGE ( 'NONE', *, *, #45527, .T. ) ;
#41407 = AXIS2_PLACEMENT_3D ( 'NONE', #9354, #4819, #43998 ) ;
#41408 = CARTESIAN_POINT ( 'NONE',  ( -65.08700002776164695, -9.158398745557436271, 0.7610157271824009584 ) ) ;
#41409 = FACE_OUTER_BOUND ( 'NONE', #39794, .T. ) ;
#41410 = CARTESIAN_POINT ( 'NONE',  ( -9.975539614456023330, 0.000000000000000000, 6.589435518685016646 ) ) ;
#41411 = EDGE_LOOP ( 'NONE', ( #13170, #36297, #50675, #48829 ) ) ;
#41412 = LINE ( 'NONE', #36582, #20134 ) ;
#41413 = LINE ( 'NONE', #20077, #8302 ) ;
#41414 = VECTOR ( 'NONE', #37115, 1000.000000000000227 ) ;
#41415 = EDGE_CURVE ( 'NONE', #47873, #7239, #12576, .T. ) ;
#41416 = CARTESIAN_POINT ( 'NONE',  ( -11.73723008791625766, -0.1117717739994089354, 7.777512339822061804 ) ) ;
#41417 = DIRECTION ( 'NONE',  ( 0.9321478471874541372, 0.000000000000000000, -0.3620778797217453771 ) ) ;
#41418 = CARTESIAN_POINT ( 'NONE',  ( -17.73140113748535285, 0.000000000000000000, 13.85752530597602039 ) ) ;
#41419 = VECTOR ( 'NONE', #14965, 1000.000000000000227 ) ;
#41420 = ADVANCED_FACE ( 'NONE', ( #16530 ), #42942, .F. ) ;
#41421 = CARTESIAN_POINT ( 'NONE',  ( -9.342070512798265725, 0.000000000000000000, 10.59882438848031505 ) ) ;
#41422 = DIRECTION ( 'NONE',  ( 0.000000000000000000, -0.000000000000000000, -1.000000000000000000 ) ) ;
#41423 = LINE ( 'NONE', #50502, #54785 ) ;
#41424 = ADVANCED_FACE ( 'NONE', ( #47480 ), #47783, .F. ) ;
#41425 = CARTESIAN_POINT ( 'NONE',  ( -9.115871106642465804, 2.779451633208005923, 3.525154055174515744 ) ) ;
#41426 = ORIENTED_EDGE ( 'NONE', *, *, #29406, .T. ) ;
#41427 = FACE_OUTER_BOUND ( 'NONE', #10163, .T. ) ;
#41428 = ORIENTED_EDGE ( 'NONE', *, *, #27472, .T. ) ;
#41429 = EDGE_CURVE ( 'NONE', #43064, #1437, #29892, .T. ) ;
#41430 = EDGE_CURVE ( 'NONE', #33602, #33755, #4046, .T. ) ;
#41431 = ADVANCED_FACE ( 'NONE', ( #43499 ), #29630, .F. ) ;
#41432 = AXIS2_PLACEMENT_3D ( 'NONE', #4477, #21787, #26321 ) ;
#41433 = FACE_OUTER_BOUND ( 'NONE', #53087, .T. ) ;
#41434 = CARTESIAN_POINT ( 'NONE',  ( -11.77243710274829525, -0.1191753592594197858, 11.50324088822667612 ) ) ;
#41435 = LINE ( 'NONE', #42543, #24154 ) ;
#41436 = DIRECTION ( 'NONE',  ( -0.5364919789714478471, 0.6444004775717705469, -0.5449076811759709926 ) ) ;
#41437 = DIRECTION ( 'NONE',  ( 0.8531650599175529814, -0.4028455766673920135, -0.3313982828793697877 ) ) ;
#41438 = VECTOR ( 'NONE', #17287, 999.9999999999998863 ) ;
#41439 = VECTOR ( 'NONE', #47997, 999.9999999999998863 ) ;
#41440 = FACE_OUTER_BOUND ( 'NONE', #22860, .T. ) ;
#41441 = DIRECTION ( 'NONE',  ( -1.342881288441436668E-15, -1.761067553935943425E-16, 1.000000000000000000 ) ) ;
#41442 = DIRECTION ( 'NONE',  ( -0.005002170337468016433, -0.7660444431189770143, 0.6427681459581293666 ) ) ;
#41443 = CARTESIAN_POINT ( 'NONE',  ( -11.14933798647950880, 0.000000000000000000, 3.994976259692639697 ) ) ;
#41444 = FACE_OUTER_BOUND ( 'NONE', #30708, .T. ) ;
#41445 = DIRECTION ( 'NONE',  ( 0.000000000000000000, -1.000000000000000000, 0.000000000000000000 ) ) ;
#41446 = FACE_OUTER_BOUND ( 'NONE', #22542, .T. ) ;
#41447 = CARTESIAN_POINT ( 'NONE',  ( -18.66354898467281132, 0.000000000000000000, 14.21960318569776582 ) ) ;
#41448 = ADVANCED_FACE ( 'NONE', ( #4347 ), #13421, .F. ) ;
#41449 = CARTESIAN_POINT ( 'NONE',  ( -25.20123094555300369, 0.000000000000000000, 6.470945668149052032 ) ) ;
#41450 = CARTESIAN_POINT ( 'NONE',  ( -18.67775241435682432, 0.000000000000000000, 4.136394454059623804 ) ) ;
#41451 = CARTESIAN_POINT ( 'NONE',  ( -17.74560456716937296, 0.000000000000000000, 3.774316574337878372 ) ) ;
#41452 = ORIENTED_EDGE ( 'NONE', *, *, #17932, .T. ) ;
#41453 = EDGE_CURVE ( 'NONE', #29528, #1645, #25082, .T. ) ;
#41454 = DIRECTION ( 'NONE',  ( -0.7660212471507179544, -0.6427876096865405842, -0.005961354470445141482 ) ) ;
#41455 = VERTEX_POINT ( 'NONE', #4598 ) ;
#41456 = EDGE_CURVE ( 'NONE', #12052, #23033, #34426, .T. ) ;
#41457 = LINE ( 'NONE', #54769, #15811 ) ;
#41458 = DIRECTION ( 'NONE',  ( -0.005002170337468016433, -0.7660444431189770143, 0.6427681459581293666 ) ) ;
#41459 = EDGE_CURVE ( 'NONE', #3819, #26525, #39236, .T. ) ;
#41460 = ORIENTED_EDGE ( 'NONE', *, *, #44499, .F. ) ;
#41461 = VECTOR ( 'NONE', #673, 999.9999999999998863 ) ;
#41462 = EDGE_LOOP ( 'NONE', ( #15389, #24045, #22211, #51136 ) ) ;
#41463 = CARTESIAN_POINT ( 'NONE',  ( -9.945481425013914745, 0.000000000000000000, 2.727022726812396769 ) ) ;
#41464 = VECTOR ( 'NONE', #30561, 1000.000000000000227 ) ;
#41465 = ORIENTED_EDGE ( 'NONE', *, *, #41429, .F. ) ;
#41466 = VERTEX_POINT ( 'NONE', #327 ) ;
#41467 = VERTEX_POINT ( 'NONE', #3487 ) ;
#41468 = DIRECTION ( 'NONE',  ( -0.5364919789714478471, 0.6444004775717705469, -0.5449076811759709926 ) ) ;
#41469 = DIRECTION ( 'NONE',  ( 0.000000000000000000, -0.000000000000000000, -1.000000000000000000 ) ) ;
#41470 = LINE ( 'NONE', #19305, #17581 ) ;
#41471 = VECTOR ( 'NONE', #51265, 999.9999999999998863 ) ;
#41472 = ORIENTED_EDGE ( 'NONE', *, *, #22760, .T. ) ;
#41473 = ORIENTED_EDGE ( 'NONE', *, *, #54763, .T. ) ;
#41474 = CARTESIAN_POINT ( 'NONE',  ( -66.34686992624823176, -1.387778780781445676E-14, 4.515874129472569720 ) ) ;
#41475 = DIRECTION ( 'NONE',  ( 0.007781995580012663651, 0.000000000000000000, -0.9999697198139515519 ) ) ;
#41476 = VERTEX_POINT ( 'NONE', #25925 ) ;
#41477 = CARTESIAN_POINT ( 'NONE',  ( -8.860905869600902207, 1.745854407020028306E-14, -4.599999999999999645 ) ) ;
#41478 = ORIENTED_EDGE ( 'NONE', *, *, #46989, .F. ) ;
#41479 = PLANE ( 'NONE',  #16972 ) ;
#41480 = DIRECTION ( 'NONE',  ( 0.007781995580012662783, 0.000000000000000000, -0.9999697198139514409 ) ) ;
#41481 = ORIENTED_EDGE ( 'NONE', *, *, #46398, .F. ) ;
#41482 = PLANE ( 'NONE',  #40930 ) ;
#41483 = CARTESIAN_POINT ( 'NONE',  ( -17.46532115785441519, 0.000000000000000000, 13.67492996699914265 ) ) ;
#41484 = ORIENTED_EDGE ( 'NONE', *, *, #5208, .F. ) ;
#41485 = DIRECTION ( 'NONE',  ( -0.6427681459581293666, -0.7660444431189770143, -0.005002170337467561935 ) ) ;
#41486 = LINE ( 'NONE', #16195, #6729 ) ;
#41487 = LINE ( 'NONE', #15612, #44608 ) ;
#41488 = VERTEX_POINT ( 'NONE', #51732 ) ;
#41489 = EDGE_CURVE ( 'NONE', #1853, #6537, #38968, .T. ) ;
#41490 = EDGE_CURVE ( 'NONE', #51521, #14570, #25349, .T. ) ;
#41491 = CARTESIAN_POINT ( 'NONE',  ( -21.87999231953709867, -4.403642575758159872, 12.40799148664158125 ) ) ;
#41492 = CARTESIAN_POINT ( 'NONE',  ( -25.20123094555300369, 0.000000000000000000, 6.470945668149052032 ) ) ;
#41493 = CARTESIAN_POINT ( 'NONE',  ( -10.90481340813819600, 0.000000000000000000, 6.582203695148996836 ) ) ;
#41494 = DIRECTION ( 'NONE',  ( 0.005961354470445682716, -0.6427876096865404731, -0.7660212471507180654 ) ) ;
#41495 = ADVANCED_FACE ( 'NONE', ( #36 ), #17367, .F. ) ;
#41496 = PLANE ( 'NONE',  #2255 ) ;
#41497 = DIRECTION ( 'NONE',  ( -0.7660212471507179544, -0.6427876096865405842, -0.005961354470445141482 ) ) ;
#41498 = VECTOR ( 'NONE', #16091, 999.9999999999998863 ) ;
#41499 = DIRECTION ( 'NONE',  ( 0.9999697198139515519, 0.000000000000000000, 0.007781995580013368816 ) ) ;
#41500 = ORIENTED_EDGE ( 'NONE', *, *, #47849, .F. ) ;
#41501 = DIRECTION ( 'NONE',  ( -0.9999697198139514409, -0.000000000000000000, -0.007781995580013368816 ) ) ;
#41502 = PLANE ( 'NONE',  #12345 ) ;
#41503 = CARTESIAN_POINT ( 'NONE',  ( -65.59336848870630376, 4.336808689942017736E-15, -0.3798655365425420150 ) ) ;
#41504 = ORIENTED_EDGE ( 'NONE', *, *, #7641, .F. ) ;
#41505 = CARTESIAN_POINT ( 'NONE',  ( -8.509919637592204822, -0.1191753592594197858, 10.23596830920056711 ) ) ;
#41506 = CARTESIAN_POINT ( 'NONE',  ( -17.74834732018306482, 3.200641362704010451, 3.473875350394609374 ) ) ;
#41507 = AXIS2_PLACEMENT_3D ( 'NONE', #22219, #17380, #9145 ) ;
#41508 = CARTESIAN_POINT ( 'NONE',  ( -18.39746900504187010, 0.000000000000000000, 14.03700784672088808 ) ) ;
#41509 = CARTESIAN_POINT ( 'NONE',  ( -12.70458494993575194, -0.1191753592594197858, 11.86531876794841978 ) ) ;
#41510 = ADVANCED_FACE ( 'NONE', ( #44908 ), #14523, .F. ) ;
#41511 = CARTESIAN_POINT ( 'NONE',  ( -56.75000000000001421, 6.149180203093333574, 2.449489742783260038 ) ) ;
#41512 = ORIENTED_EDGE ( 'NONE', *, *, #33013, .F. ) ;
#41513 = ORIENTED_EDGE ( 'NONE', *, *, #50317, .F. ) ;
#41514 = EDGE_CURVE ( 'NONE', #25391, #27823, #13672, .T. ) ;
#41515 = CARTESIAN_POINT ( 'NONE',  ( -25.83279121425626812, 17.74370688441070953, 4.604227610039242968 ) ) ;
#41516 = CARTESIAN_POINT ( 'NONE',  ( -12.78178805287288178, 0.6102101463440037232, 2.847660476479313640 ) ) ;
#41517 = EDGE_CURVE ( 'NONE', #14924, #3628, #31284, .T. ) ;
#41518 = ORIENTED_EDGE ( 'NONE', *, *, #17610, .T. ) ;
#41519 = PLANE ( 'NONE',  #26756 ) ;
#41520 = B_SPLINE_CURVE_WITH_KNOTS ( 'NONE', 3,
 ( #2450, #28561, #54976, #45890, #41360, #10957, #11537, #32809, #15242, #28855, #19482, #32556, #50127, #45592, #11238, #46415, #40796, #45324, #46154, #41878, #53838, #37647, #6435, #49859 ),
 .UNSPECIFIED., .F., .F.,
 ( 4, 1, 1, 1, 1, 2, 2, 1, 1, 1, 1, 1, 2, 2, 1, 1, 1, 4 ),
 ( 0.4483797419119410210, 0.4828560080424447176, 0.4914750745750705030, 0.4957846078413832847, 0.4979393744745396755, 0.4990167577911179264, 0.5000941411076962329, 0.5173322741729480256, 0.5862848064339559739, 0.7241898709559724256, 0.7414280040212243295, 0.7457375372875375552, 0.7478923039206943901, 0.7500470705538511140, 0.7586661370864771214, 0.7931424032169802629, 0.8620949354779869900, 1.000000000000000000 ),
 .UNSPECIFIED. ) ;
#41521 = ORIENTED_EDGE ( 'NONE', *, *, #15911, .F. ) ;
#41522 = DIRECTION ( 'NONE',  ( 0.007781995580012662783, 0.000000000000000000, -0.9999697198139514409 ) ) ;
#41523 = EDGE_CURVE ( 'NONE', #42201, #49088, #4883, .T. ) ;
#41524 = VERTEX_POINT ( 'NONE', #17956 ) ;
#41525 = ORIENTED_EDGE ( 'NONE', *, *, #25540, .F. ) ;
#41526 = LINE ( 'NONE', #42370, #46470 ) ;
#41527 = PLANE ( 'NONE',  #35053 ) ;
#41528 = CARTESIAN_POINT ( 'NONE',  ( -22.40634380310664397, 0.000000000000000000, 5.584705972946605534 ) ) ;
#41529 = EDGE_LOOP ( 'NONE', ( #36958, #50246, #50167, #22620 ) ) ;
#41530 = DIRECTION ( 'NONE',  ( 0.000000000000000000, -1.000000000000000000, 0.000000000000000000 ) ) ;
#41531 = ORIENTED_EDGE ( 'NONE', *, *, #42925, .T. ) ;
#41532 = ORIENTED_EDGE ( 'NONE', *, *, #39879, .T. ) ;
#41533 = ORIENTED_EDGE ( 'NONE', *, *, #3499, .T. ) ;
#41534 = CARTESIAN_POINT ( 'NONE',  ( -27.99923088623136636, 0.000000000000000000, 7.757173251277078130 ) ) ;
#41535 = ORIENTED_EDGE ( 'NONE', *, *, #24223, .T. ) ;
#41536 = DIRECTION ( 'NONE',  ( 0.007781995580012663651, -3.146120232559066537E-19, -0.9999697198139514409 ) ) ;
#41537 = ORIENTED_EDGE ( 'NONE', *, *, #9586, .T. ) ;
#41538 = LINE ( 'NONE', #45493, #18601 ) ;
#41539 = LINE ( 'NONE', #15984, #33151 ) ;
#41540 = VECTOR ( 'NONE', #32754, 1000.000000000000114 ) ;
#41541 = VERTEX_POINT ( 'NONE', #5186 ) ;
#41542 = PLANE ( 'NONE',  #54022 ) ;
#41543 = ORIENTED_EDGE ( 'NONE', *, *, #1643, .F. ) ;
#41544 = DIRECTION ( 'NONE',  ( -0.9999697198139514409, -0.000000000000000000, -0.007781995580013368816 ) ) ;
#41545 = LINE ( 'NONE', #40974, #33866 ) ;
#41546 = CARTESIAN_POINT ( 'NONE',  ( -18.60807716309514959, 0.000000000000000000, 7.091593241429392513 ) ) ;
#41547 = CARTESIAN_POINT ( 'NONE',  ( -20.43000850590469497, 4.172053068839010947, 4.484530505201751005 ) ) ;
#41548 = DIRECTION ( 'NONE',  ( 0.6427681459581294776, -0.7660444431189769032, 0.005002170337467562802 ) ) ;
#41549 = PLANE ( 'NONE',  #48213 ) ;
#41550 = EDGE_LOOP ( 'NONE', ( #19662, #19314, #51308, #34726 ) ) ;
#41551 = EDGE_CURVE ( 'NONE', #17246, #33621, #52849, .T. ) ;
#41552 = ORIENTED_EDGE ( 'NONE', *, *, #5182, .F. ) ;
#41553 = CARTESIAN_POINT ( 'NONE',  ( -29.86274838104827367, -0.1191753592594197858, 8.381332038739175871 ) ) ;
#41554 = CARTESIAN_POINT ( 'NONE',  ( -15.86710544311044302, 0.000000000000000000, 13.13336954653252953 ) ) ;
#41555 = EDGE_CURVE ( 'NONE', #12878, #14361, #30985, .T. ) ;
#41556 = EDGE_CURVE ( 'NONE', #10765, #12832, #27034, .T. ) ;
#41557 = LINE ( 'NONE', #33584, #32150 ) ;
#41558 = DIRECTION ( 'NONE',  ( -0.5449076811759708816, 0.6444004775717707689, 0.5364919789714475140 ) ) ;
#41559 = DIRECTION ( 'NONE',  ( -0.3620778797217457656, 0.000000000000000000, -0.9321478471874539151 ) ) ;
#41560 = VERTEX_POINT ( 'NONE', #40073 ) ;
#41561 = DIRECTION ( 'NONE',  ( -0.9999697198139514409, -0.000000000000000000, -0.007781995580013368816 ) ) ;
#41562 = CARTESIAN_POINT ( 'NONE',  ( -13.07066190154808361, 0.000000000000000000, 12.04713590736729678 ) ) ;
#41563 = ORIENTED_EDGE ( 'NONE', *, *, #8155, .T. ) ;
#41564 = DIRECTION ( 'NONE',  ( 0.7660212471507180654, -0.6427876096865404731, 0.005961354470445141482 ) ) ;
#41565 = DIRECTION ( 'NONE',  ( 0.005961354470445682716, -0.6427876096865404731, -0.7660212471507180654 ) ) ;
#41566 = EDGE_LOOP ( 'NONE', ( #8822, #31388, #55090, #55570 ) ) ;
#41567 = CARTESIAN_POINT ( 'NONE',  ( -70.12629345720861807, 1.999999999999801048, 7.856885134693458284 ) ) ;
#41568 = CARTESIAN_POINT ( 'NONE',  ( -13.73672976910459909, 0.000000000000000000, 12.22661844811216270 ) ) ;
#41569 = CARTESIAN_POINT ( 'NONE',  ( -19.81657051840181794, -0.3560938001956556742, 4.567388823514338725 ) ) ;
#41570 = LINE ( 'NONE', #11481, #28709 ) ;
#41571 = CARTESIAN_POINT ( 'NONE',  ( -18.67697421479882181, -0.1191753592594197858, 4.036397482078229793 ) ) ;
#41572 = ORIENTED_EDGE ( 'NONE', *, *, #11645, .T. ) ;
#41573 = ORIENTED_EDGE ( 'NONE', *, *, #18813, .T. ) ;
#41574 = CARTESIAN_POINT ( 'NONE',  ( -14.17319835266821393, 0.000000000000000000, 8.603434773024542181 ) ) ;
#41575 = LINE ( 'NONE', #55461, #21339 ) ;
#41576 = CARTESIAN_POINT ( 'NONE',  ( -15.03495456790438389, -0.1191753592594197858, 12.77051346725278158 ) ) ;
#41577 = DIRECTION ( 'NONE',  ( 0.9999697198139515519, 0.000000000000000000, 0.007781995580013368816 ) ) ;
#41578 = AXIS2_PLACEMENT_3D ( 'NONE', #10584, #14284, #27303 ) ;
#41579 = PLANE ( 'NONE',  #26499 ) ;
#41580 = CARTESIAN_POINT ( 'NONE',  ( -13.20239044008653195, 2.229229656569007734, 1.739064436143978432 ) ) ;
#41581 = ORIENTED_EDGE ( 'NONE', *, *, #39309, .F. ) ;
#41582 = DIRECTION ( 'NONE',  ( 0.005002170337468016433, -0.7660444431189770143, -0.6427681459581293666 ) ) ;
#41583 = ADVANCED_FACE ( 'NONE', ( #36375 ), #6027, .F. ) ;
#41584 = CARTESIAN_POINT ( 'NONE',  ( -27.99767448711536133, 0.000000000000000000, 7.557179307314289218 ) ) ;
#41585 = DIRECTION ( 'NONE',  ( -0.005002170337468016433, -0.7660444431189770143, 0.6427681459581293666 ) ) ;
#41586 = ORIENTED_EDGE ( 'NONE', *, *, #13030, .T. ) ;
#41587 = EDGE_CURVE ( 'NONE', #50902, #53298, #5723, .T. ) ;
#41588 = CARTESIAN_POINT ( 'NONE',  ( -11.36804826722767103, 24.91136206679768605, -5.000000000000000888 ) ) ;
#41589 = CARTESIAN_POINT ( 'NONE',  ( -19.45503627000849889, -1.000000000000000000, 7.556996783084074742 ) ) ;
#41590 = LINE ( 'NONE', #27991, #32984 ) ;
#41591 = ORIENTED_EDGE ( 'NONE', *, *, #11075, .F. ) ;
#41592 = DIRECTION ( 'NONE',  ( -0.5449076811759708816, 0.6444004775717707689, 0.5364919789714475140 ) ) ;
#41593 = EDGE_CURVE ( 'NONE', #45628, #1080, #53427, .T. ) ;
#41594 = EDGE_LOOP ( 'NONE', ( #50177, #15857, #3609, #15731 ) ) ;
#41595 = ORIENTED_EDGE ( 'NONE', *, *, #9736, .T. ) ;
#41596 = EDGE_LOOP ( 'NONE', ( #46390, #4330, #16491, #35331 ) ) ;
#41597 = ORIENTED_EDGE ( 'NONE', *, *, #21404, .T. ) ;
#41598 = ORIENTED_EDGE ( 'NONE', *, *, #19929, .F. ) ;
#41599 = CARTESIAN_POINT ( 'NONE',  ( -22.40556560354864146, -0.1191753592594197858, 5.484709000965211523 ) ) ;
#41600 = VERTEX_POINT ( 'NONE', #48304 ) ;
#41601 = ORIENTED_EDGE ( 'NONE', *, *, #55949, .F. ) ;
#41602 = CARTESIAN_POINT ( 'NONE',  ( -16.96273579891908412, -0.8417996532631562001, 3.443365942170054428 ) ) ;
#41603 = ORIENTED_EDGE ( 'NONE', *, *, #15121, .F. ) ;
#41604 = ORIENTED_EDGE ( 'NONE', *, *, #38711, .T. ) ;
#41605 = EDGE_CURVE ( 'NONE', #6097, #4731, #53163, .T. ) ;
#41606 = DIRECTION ( 'NONE',  ( 0.007781995580012663651, -3.146120232559066537E-19, -0.9999697198139514409 ) ) ;
#41607 = PLANE ( 'NONE',  #28505 ) ;
#41608 = FACE_OUTER_BOUND ( 'NONE', #47802, .T. ) ;
#41609 = CARTESIAN_POINT ( 'NONE',  ( -8.837649716295214120, 0.000000000000000000, 5.490294631563745753 ) ) ;
#41610 = EDGE_CURVE ( 'NONE', #19103, #7637, #22500, .T. ) ;
#41611 = FACE_OUTER_BOUND ( 'NONE', #1746, .T. ) ;
#41612 = VERTEX_POINT ( 'NONE', #26446 ) ;
#41613 = ORIENTED_EDGE ( 'NONE', *, *, #37233, .F. ) ;
#41614 = EDGE_CURVE ( 'NONE', #13117, #41065, #22208, .T. ) ;
#41615 = DIRECTION ( 'NONE',  ( 0.007781995580012662783, 0.000000000000000000, -0.9999697198139514409 ) ) ;
#41616 = PLANE ( 'NONE',  #54771 ) ;
#41617 = EDGE_CURVE ( 'NONE', #37343, #42852, #26742, .T. ) ;
#41618 = PLANE ( 'NONE',  #52377 ) ;
#41619 = LINE ( 'NONE', #49860, #28659 ) ;
#41620 = LINE ( 'NONE', #24567, #7706 ) ;
#41621 = FACE_OUTER_BOUND ( 'NONE', #9320, .T. ) ;
#41622 = ORIENTED_EDGE ( 'NONE', *, *, #14012, .T. ) ;
#41623 = CARTESIAN_POINT ( 'NONE',  ( -17.89379923316518273, 2.229229656569005957, 7.490426063039901550 ) ) ;
#41624 = ORIENTED_EDGE ( 'NONE', *, *, #46929, .F. ) ;
#41625 = PLANE ( 'NONE',  #41932 ) ;
#41626 = DIRECTION ( 'NONE',  ( -0.5449076811759708816, 0.6444004775717707689, 0.5364919789714475140 ) ) ;
#41627 = LINE ( 'NONE', #2708, #12747 ) ;
#41628 = LINE ( 'NONE', #7018, #22258 ) ;
#41629 = CARTESIAN_POINT ( 'NONE',  ( -17.26082817053895724, 2.067327705546508021, 3.320664995664557750 ) ) ;
#41630 = ADVANCED_FACE ( 'NONE', ( #14803 ), #48890, .F. ) ;
#41631 = ORIENTED_EDGE ( 'NONE', *, *, #32964, .F. ) ;
#41632 = DIRECTION ( 'NONE',  ( 0.5364919789714477361, 0.6444004775717706579, 0.5449076811759711036 ) ) ;
#41633 = FACE_OUTER_BOUND ( 'NONE', #34838, .T. ) ;
#41634 = PLANE ( 'NONE',  #20633 ) ;
#41635 = DIRECTION ( 'NONE',  ( 0.5449076811759707706, 0.6444004775717708799, -0.5364919789714476250 ) ) ;
#41636 = DIRECTION ( 'NONE',  ( 0.5449076811759707706, 0.6444004775717708799, -0.5364919789714476250 ) ) ;
#41637 = DIRECTION ( 'NONE',  ( 0.007781995580012663651, 0.000000000000000000, -0.9999697198139515519 ) ) ;
#41638 = DIRECTION ( 'NONE',  ( -0.5449076811759708816, 0.6444004775717707689, 0.5364919789714475140 ) ) ;
#41639 = DIRECTION ( 'NONE',  ( 0.5364919789714477361, 0.6444004775717706579, 0.5449076811759711036 ) ) ;
#41640 = CARTESIAN_POINT ( 'NONE',  ( -9.029021499742155399, 0.000000000000000000, 4.380809122674449441 ) ) ;
#41641 = AXIS2_PLACEMENT_3D ( 'NONE', #7620, #36612, #41145 ) ;
#41642 = ORIENTED_EDGE ( 'NONE', *, *, #46255, .F. ) ;
#41643 = EDGE_CURVE ( 'NONE', #25831, #53959, #49149, .T. ) ;
#41644 = VERTEX_POINT ( 'NONE', #53685 ) ;
#41645 = ORIENTED_EDGE ( 'NONE', *, *, #25874, .T. ) ;
#41646 = VERTEX_POINT ( 'NONE', #43768 ) ;
#41647 = VERTEX_POINT ( 'NONE', #52576 ) ;
#41648 = FACE_OUTER_BOUND ( 'NONE', #34798, .T. ) ;
#41649 = LINE ( 'NONE', #20062, #16585 ) ;
#41650 = CARTESIAN_POINT ( 'NONE',  ( -25.20278734466900517, 0.000000000000000000, 6.670939612111840944 ) ) ;
#41651 = EDGE_CURVE ( 'NONE', #41524, #21438, #9418, .T. ) ;
#41652 = ORIENTED_EDGE ( 'NONE', *, *, #42512, .F. ) ;
#41653 = ORIENTED_EDGE ( 'NONE', *, *, #46297, .T. ) ;
#41654 = ORIENTED_EDGE ( 'NONE', *, *, #39709, .T. ) ;
#41655 = CARTESIAN_POINT ( 'NONE',  ( -64.77372111108157071, -11.13558095840576989, -2.612833193081008698 ) ) ;
#41656 = EDGE_CURVE ( 'NONE', #41786, #14819, #54511, .T. ) ;
#41657 = VERTEX_POINT ( 'NONE', #32954 ) ;
#41658 = EDGE_CURVE ( 'NONE', #16476, #50946, #41196, .T. ) ;
#41659 = CARTESIAN_POINT ( 'NONE',  ( -65.38822204059790977, -9.192941140068732864, 3.032081494020515411 ) ) ;
#41660 = DIRECTION ( 'NONE',  ( 0.007781995580012663651, -3.146120232559066537E-19, -0.9999697198139514409 ) ) ;
#41661 = CARTESIAN_POINT ( 'NONE',  ( -15.59709573620632383, 5.629170628041512359, 2.560773380055879844 ) ) ;
#41662 = EDGE_CURVE ( 'NONE', #44744, #30955, #1989, .T. ) ;
#41663 = VERTEX_POINT ( 'NONE', #33258 ) ;
#41664 = CARTESIAN_POINT ( 'NONE',  ( -19.75917934048144531, -0.8417996532631562001, 4.529599581335290281 ) ) ;
#41665 = ORIENTED_EDGE ( 'NONE', *, *, #40253, .T. ) ;
#41666 = LINE ( 'NONE', #11844, #14636 ) ;
#41667 = EDGE_CURVE ( 'NONE', #2799, #43546, #41486, .T. ) ;
#41668 = LINE ( 'NONE', #19823, #33911 ) ;
#41669 = EDGE_CURVE ( 'NONE', #39352, #46530, #2569, .T. ) ;
#41670 = DIRECTION ( 'NONE',  ( 0.9999697198139515519, 0.000000000000000000, 0.007781995580013368816 ) ) ;
#41671 = CARTESIAN_POINT ( 'NONE',  ( -13.44920839603113905, -1.651309408375657206, 2.052764979558574510 ) ) ;
#41672 = CARTESIAN_POINT ( 'NONE',  ( -46.55906441860520317, 5.863990010960497656, 5.000000000000000000 ) ) ;
#41673 = CARTESIAN_POINT ( 'NONE',  ( -11.74061653640753455, -0.1191753592594181482, 7.414366449667899595 ) ) ;
#41674 = DIRECTION ( 'NONE',  ( 0.9321478471874540261, 0.000000000000000000, -0.3620778797217457101 ) ) ;
#41675 = PLANE ( 'NONE',  #33915 ) ;
#41676 = CARTESIAN_POINT ( 'NONE',  ( -14.46888367232926420, 0.000000000000000000, 12.59025272694991315 ) ) ;
#41677 = ORIENTED_EDGE ( 'NONE', *, *, #24596, .T. ) ;
#41678 = DIRECTION ( 'NONE',  ( -0.5364919789714478471, 0.6444004775717705469, -0.5449076811759709926 ) ) ;
#41679 = VERTEX_POINT ( 'NONE', #40911 ) ;
#41680 = EDGE_CURVE ( 'NONE', #47084, #12623, #7381, .T. ) ;
#41681 = CARTESIAN_POINT ( 'NONE',  ( -60.92294909528612834, 7.225036622302103417, -3.000000000000007105 ) ) ;
#41682 = LINE ( 'NONE', #20091, #43220 ) ;
#41683 = DIRECTION ( 'NONE',  ( -0.5449076811759708816, 0.6444004775717707689, 0.5364919789714475140 ) ) ;
#41684 = DIRECTION ( 'NONE',  ( 0.5364919789714477361, 0.6444004775717706579, 0.5449076811759711036 ) ) ;
#41685 = DIRECTION ( 'NONE',  ( 0.6427681459581294776, -0.7660444431189769032, 0.005002170337467562802 ) ) ;
#41686 = EDGE_CURVE ( 'NONE', #30915, #31264, #50565, .T. ) ;
#41687 = DIRECTION ( 'NONE',  ( -0.9999697198139514409, -0.000000000000000000, -0.007781995580013368816 ) ) ;
#41688 = ORIENTED_EDGE ( 'NONE', *, *, #49333, .T. ) ;
#41689 = CARTESIAN_POINT ( 'NONE',  ( -15.53836850813863890, 0.000000000000000000, 4.899490005142868476 ) ) ;
#41690 = FACE_OUTER_BOUND ( 'NONE', #42713, .T. ) ;
#41691 = DIRECTION ( 'NONE',  ( 0.005961354470445682716, -0.6427876096865404731, -0.7660212471507180654 ) ) ;
#41692 = CARTESIAN_POINT ( 'NONE',  ( -13.27065584551087163, 0.000000000000000000, 12.04557950825129176 ) ) ;
#41693 = FACE_OUTER_BOUND ( 'NONE', #27756, .T. ) ;
#41694 = DIRECTION ( 'NONE',  ( -0.005002170337468016433, -0.7660444431189770143, 0.6427681459581293666 ) ) ;
#41695 = CARTESIAN_POINT ( 'NONE',  ( -11.61265722893131525, 0.000000000000000000, 3.822044588629654349 ) ) ;
#41696 = LINE ( 'NONE', #33214, #9709 ) ;
#41697 = DIRECTION ( 'NONE',  ( 0.007781995580012663651, 0.000000000000000000, -0.9999697198139515519 ) ) ;
#41698 = VERTEX_POINT ( 'NONE', #49449 ) ;
#41699 = CARTESIAN_POINT ( 'NONE',  ( -19.32961685222932147, 0.000000000000000000, 14.39908572644263351 ) ) ;
#41700 = ORIENTED_EDGE ( 'NONE', *, *, #49426, .F. ) ;
#41701 = FACE_OUTER_BOUND ( 'NONE', #24278, .T. ) ;
#41703 = MANIFOLD_SOLID_BREP ( 'Boss-Extrude3', #6831 ) ;
#41702 = PLANE ( 'NONE',  #34643 ) ;
#41704 = EDGE_LOOP ( 'NONE', ( #44965, #34397, #10847, #4881 ) ) ;
#41705 = ADVANCED_FACE ( 'NONE', ( #54258 ), #28131, .F. ) ;
#41706 = ORIENTED_EDGE ( 'NONE', *, *, #21748, .T. ) ;
#41707 = DIRECTION ( 'NONE',  ( 0.9999697198139515519, 0.000000000000000000, 0.007781995580013368816 ) ) ;
#41708 = AXIS2_PLACEMENT_3D ( 'NONE', #48479, #2158, #6444 ) ;
#41709 = EDGE_LOOP ( 'NONE', ( #45695, #6493, #51705, #17028 ) ) ;
#41710 = ORIENTED_EDGE ( 'NONE', *, *, #25278, .T. ) ;
#41711 = VERTEX_POINT ( 'NONE', #32668 ) ;
#41712 = DIRECTION ( 'NONE',  ( 0.6246952433987893460, 0.7422098413412802076, -0.2426528472758539279 ) ) ;
#41713 = LINE ( 'NONE', #3403, #27832 ) ;
#41714 = LINE ( 'NONE', #3948, #14019 ) ;
#41715 = EDGE_CURVE ( 'NONE', #5277, #32587, #20457, .T. ) ;
#41716 = ADVANCED_FACE ( 'NONE', ( #11080 ), #28409, .F. ) ;
#41717 = EDGE_LOOP ( 'NONE', ( #45741, #48966, #23695, #35531 ) ) ;
#41718 = ORIENTED_EDGE ( 'NONE', *, *, #21867, .F. ) ;
#41719 = EDGE_CURVE ( 'NONE', #34036, #2679, #7127, .T. ) ;
#41720 = CARTESIAN_POINT ( 'NONE',  ( 2.072287782118878319, 0.000000000000000000, -2.950529333540147015 ) ) ;
#41721 = CARTESIAN_POINT ( 'NONE',  ( -27.56484202182514665, 16.74370688441070953, -4.657437592157546824 ) ) ;
#41722 = ORIENTED_EDGE ( 'NONE', *, *, #40180, .F. ) ;
#41723 = CARTESIAN_POINT ( 'NONE',  ( -17.93139508144814442, 0.000000000000000000, 13.85596890686001537 ) ) ;
#41724 = ORIENTED_EDGE ( 'NONE', *, *, #34681, .F. ) ;
#41725 = DIRECTION ( 'NONE',  ( -0.005002170337468016433, -0.7660444431189770143, 0.6427681459581293666 ) ) ;
#41726 = DIRECTION ( 'NONE',  ( -0.6427681459581293666, -0.7660444431189770143, -0.005002170337467561935 ) ) ;
#41727 = ORIENTED_EDGE ( 'NONE', *, *, #35222, .F. ) ;
#41728 = DIRECTION ( 'NONE',  ( -0.5449076811759708816, 0.6444004775717707689, 0.5364919789714475140 ) ) ;
#41729 = EDGE_CURVE ( 'NONE', #12359, #2867, #6553, .T. ) ;
#41730 = ADVANCED_FACE ( 'NONE', ( #38907 ), #17049, .F. ) ;
#41731 = DIRECTION ( 'NONE',  ( 0.5449076811759707706, 0.6444004775717708799, -0.5364919789714476250 ) ) ;
#41732 = ORIENTED_EDGE ( 'NONE', *, *, #41234, .F. ) ;
#41733 = DIRECTION ( 'NONE',  ( 0.000000000000000000, -0.000000000000000000, -1.000000000000000000 ) ) ;
#41734 = CARTESIAN_POINT ( 'NONE',  ( -13.64977165607341192, -5.213152330870665097, 2.017029123393386580 ) ) ;
#41735 = EDGE_CURVE ( 'NONE', #37427, #14766, #29556, .T. ) ;
#41736 = DIRECTION ( 'NONE',  ( 0.9999697198139515519, 0.000000000000000000, 0.007781995580013368816 ) ) ;
#41737 = EDGE_LOOP ( 'NONE', ( #10357, #44761, #49944, #48205 ) ) ;
#41738 = EDGE_CURVE ( 'NONE', #4032, #17566, #51939, .T. ) ;
#41739 = CARTESIAN_POINT ( 'NONE',  ( -10.27421835998572064, 0.000000000000000000, 10.96090226820206048 ) ) ;
#41740 = DIRECTION ( 'NONE',  ( 0.005961354470445682716, -0.6427876096865404731, -0.7660212471507180654 ) ) ;
#41741 = DIRECTION ( 'NONE',  ( 0.007781995580012663651, -3.146120232559066537E-19, -0.9999697198139514409 ) ) ;
#41742 = CARTESIAN_POINT ( 'NONE',  ( -8.887694952903760992, -0.1191753592594182315, 4.112579916844113725 ) ) ;
#41743 = LINE ( 'NONE', #28416, #33123 ) ;
#41744 = CARTESIAN_POINT ( 'NONE',  ( -19.77953895519367933, 4.981562823951511731, 12.73995903822415876 ) ) ;
#41745 = AXIS2_PLACEMENT_3D ( 'NONE', #53109, #22155, #38925 ) ;
#41746 = PLANE ( 'NONE',  #12227 ) ;
#41747 = ORIENTED_EDGE ( 'NONE', *, *, #46152, .T. ) ;
#41748 = PLANE ( 'NONE',  #15348 ) ;
#41749 = DIRECTION ( 'NONE',  ( 0.000000000000000000, 0.000000000000000000, -1.000000000000000000 ) ) ;
#41750 = CARTESIAN_POINT ( 'NONE',  ( -68.87570450778353859, -0.6013635744588955445, 6.466593069172607677 ) ) ;
#41751 = ORIENTED_EDGE ( 'NONE', *, *, #15202, .F. ) ;
#41752 = DIRECTION ( 'NONE',  ( -0.005961354470445682716, -0.6427876096865404731, 0.7660212471507180654 ) ) ;
#41753 = DIRECTION ( 'NONE',  ( 2.551063935260010306E-17, -4.081702296416016490E-16, 1.000000000000000000 ) ) ;
#41754 = CARTESIAN_POINT ( 'NONE',  ( -26.13415699229845757, -0.1191753592594197858, 6.933020519852192365 ) ) ;
#41755 = PLANE ( 'NONE',  #37830 ) ;
#41756 = CARTESIAN_POINT ( 'NONE',  ( -12.48602183387798803, -2.137015261443155900, 5.039132754124569402 ) ) ;
#41757 = VERTEX_POINT ( 'NONE', #13062 ) ;
#41758 = ORIENTED_EDGE ( 'NONE', *, *, #19119, .F. ) ;
#41759 = FACE_OUTER_BOUND ( 'NONE', #42961, .T. ) ;
#41760 = EDGE_CURVE ( 'NONE', #54483, #8121, #42864, .T. ) ;
#41761 = FACE_OUTER_BOUND ( 'NONE', #5294, .T. ) ;
#41762 = CARTESIAN_POINT ( 'NONE',  ( -15.59967562208883329, 3.362543313726507499, 8.459271331385316728 ) ) ;
#41763 = AXIS2_PLACEMENT_3D ( 'NONE', #51088, #28964, #50806 ) ;
#41764 = ORIENTED_EDGE ( 'NONE', *, *, #48779, .T. ) ;
#41765 = DIRECTION ( 'NONE',  ( 0.007781995580012663651, 0.000000000000000000, -0.9999697198139515519 ) ) ;
#41766 = EDGE_CURVE ( 'NONE', #460, #30957, #11260, .T. ) ;
#41767 = ORIENTED_EDGE ( 'NONE', *, *, #33640, .T. ) ;
#41769 = EDGE_CURVE ( 'NONE', #30649, #41455, #30387, .T. ) ;
#41768 = PLANE ( 'NONE',  #43800 ) ;
#41770 = VERTEX_POINT ( 'NONE', #55652 ) ;
#41771 = EDGE_LOOP ( 'NONE', ( #22484, #43153, #51843, #10064, #28196 ) ) ;
#41772 = EDGE_CURVE ( 'NONE', #44308, #30922, #34364, .T. ) ;
#41773 = DIRECTION ( 'NONE',  ( -0.3620778797217457101, 0.000000000000000000, -0.9321478471874540261 ) ) ;
#41774 = DIRECTION ( 'NONE',  ( -0.9999697198139514409, -0.000000000000000000, -0.007781995580013368816 ) ) ;
#41775 = FACE_OUTER_BOUND ( 'NONE', #28889, .T. ) ;
#41776 = ADVANCED_FACE ( 'NONE', ( #25548 ), #30094, .F. ) ;
#41777 = EDGE_CURVE ( 'NONE', #55993, #42993, #39166, .T. ) ;
#41778 = EDGE_CURVE ( 'NONE', #2289, #37965, #46563, .T. ) ;
#41779 = ORIENTED_EDGE ( 'NONE', *, *, #42688, .F. ) ;
#41781 = DIRECTION ( 'NONE',  ( 0.5449076811759707706, 0.6444004775717708799, -0.5364919789714476250 ) ) ;
#41780 = VECTOR ( 'NONE', #9980, 1000.000000000000227 ) ;
#41782 = ORIENTED_EDGE ( 'NONE', *, *, #25224, .T. ) ;
#41783 = EDGE_CURVE ( 'NONE', #35736, #2493, #42591, .T. ) ;
#41784 = AXIS2_PLACEMENT_3D ( 'NONE', #49626, #28035, #27465 ) ;
#41785 = EDGE_LOOP ( 'NONE', ( #42087, #39098, #23570, #9961 ) ) ;
#41786 = VERTEX_POINT ( 'NONE', #21843 ) ;
#41787 = CARTESIAN_POINT ( 'NONE',  ( -19.65677579747999459, 21.21320419402548296, -4.265613255889435074 ) ) ;
#41788 = CARTESIAN_POINT ( 'NONE',  ( -18.19747506107908563, 0.000000000000000000, 14.03856424583689311 ) ) ;
#41789 = ORIENTED_EDGE ( 'NONE', *, *, #34113, .F. ) ;
#41790 = LINE ( 'NONE', #42079, #2149 ) ;
#41791 = ORIENTED_EDGE ( 'NONE', *, *, #34153, .F. ) ;
#41792 = LINE ( 'NONE', #24225, #14067 ) ;
#41793 = LINE ( 'NONE', #2885, #524 ) ;
#41794 = ORIENTED_EDGE ( 'NONE', *, *, #54485, .F. ) ;
#41795 = LINE ( 'NONE', #20217, #4136 ) ;
#41796 = ORIENTED_EDGE ( 'NONE', *, *, #18039, .T. ) ;
#41797 = EDGE_CURVE ( 'NONE', #44507, #15829, #3972, .T. ) ;
#41798 = EDGE_CURVE ( 'NONE', #48603, #41838, #16755, .T. ) ;
#41799 = LINE ( 'NONE', #2892, #27368 ) ;
#41800 = DIRECTION ( 'NONE',  ( 0.005961354470445682716, -0.6427876096865404731, -0.7660212471507180654 ) ) ;
#41801 = DIRECTION ( 'NONE',  ( -0.9999697198139514409, -0.000000000000000000, -0.007781995580013368816 ) ) ;
#41802 = CARTESIAN_POINT ( 'NONE',  ( -29.86197018149027116, 0.000000000000000000, 8.281335066757780083 ) ) ;
#41803 = EDGE_CURVE ( 'NONE', #28180, #37125, #21296, .T. ) ;
#41804 = DIRECTION ( 'NONE',  ( -0.5364919789714478471, 0.6444004775717705469, -0.5449076811759709926 ) ) ;
#41805 = LINE ( 'NONE', #51481, #7401 ) ;
#41806 = ORIENTED_EDGE ( 'NONE', *, *, #17300, .F. ) ;
#41807 = AXIS2_PLACEMENT_3D ( 'NONE', #45679, #9947, #27251 ) ;
#41809 = VERTEX_POINT ( 'NONE', #8520 ) ;
#41808 = ADVANCED_FACE ( 'NONE', ( #50818 ), #11918, .F. ) ;
#41810 = AXIS2_PLACEMENT_3D ( 'NONE', #38617, #243, #4273 ) ;
#41811 = FACE_OUTER_BOUND ( 'NONE', #25864, .T. ) ;
#41812 = PLANE ( 'NONE',  #23928 ) ;
#41813 = DIRECTION ( 'NONE',  ( 0.007781995580012663651, 0.000000000000000000, -0.9999697198139515519 ) ) ;
#41814 = CARTESIAN_POINT ( 'NONE',  ( -14.54259203834542902, -0.1159828484229813300, 8.867210191861607527 ) ) ;
#41815 = EDGE_CURVE ( 'NONE', #17943, #33865, #33787, .T. ) ;
#41816 = CARTESIAN_POINT ( 'NONE',  ( -15.98433325582929498, 4.981562823951513508, 2.731851662868523434 ) ) ;
#41817 = CARTESIAN_POINT ( 'NONE',  ( -14.94916102560700821, 0.000000000000000000, 2.688082935172642962 ) ) ;
#41818 = VERTEX_POINT ( 'NONE', #4281 ) ;
#41819 = LINE ( 'NONE', #37876, #4154 ) ;
#41820 = LINE ( 'NONE', #54335, #552 ) ;
#41821 = ORIENTED_EDGE ( 'NONE', *, *, #16398, .T. ) ;
#41822 = CARTESIAN_POINT ( 'NONE',  ( -19.27558205740430353, 0.000000000000000000, 7.455730633803142382 ) ) ;
#41823 = DIRECTION ( 'NONE',  ( -0.5449076811759708816, 0.6444004775717707689, 0.5364919789714475140 ) ) ;
#41824 = ORIENTED_EDGE ( 'NONE', *, *, #24220, .F. ) ;
#41825 = DIRECTION ( 'NONE',  ( 0.005002170337468016433, -0.7660444431189770143, -0.6427681459581293666 ) ) ;
#41826 = CARTESIAN_POINT ( 'NONE',  ( -58.00000000000000711, 2.000000000000000000, 3.000000000000008438 ) ) ;
#41827 = CARTESIAN_POINT ( 'NONE',  ( -67.27849890436391433, -9.409707134521932304, 7.454917401049827141 ) ) ;
#41828 = FACE_OUTER_BOUND ( 'NONE', #49779, .T. ) ;
#41829 = LINE ( 'NONE', #23965, #20146 ) ;
#41830 = VERTEX_POINT ( 'NONE', #12512 ) ;
#41831 = VERTEX_POINT ( 'NONE', #46870 ) ;
#41832 = DIRECTION ( 'NONE',  ( 0.007781995580012663651, -3.146120232559066537E-19, -0.9999697198139514409 ) ) ;
#41833 = PLANE ( 'NONE',  #38568 ) ;
#41834 = CARTESIAN_POINT ( 'NONE',  ( -17.84862895020420481, 4.981562823951512620, 3.456007422312016519 ) ) ;
#41835 = FACE_OUTER_BOUND ( 'NONE', #13195, .T. ) ;
#41836 = LINE ( 'NONE', #11191, #36431 ) ;
#41837 = CARTESIAN_POINT ( 'NONE',  ( -20.54204810873173415, 0.000000000000000000, 4.860550213503115558 ) ) ;
#41838 = VERTEX_POINT ( 'NONE', #29830 ) ;
#41839 = CARTESIAN_POINT ( 'NONE',  ( 5.912796793901486048, -6.204513306124834315, -2.260536671351835558 ) ) ;
#41840 = B_SPLINE_CURVE_WITH_KNOTS ( 'NONE', 1,
 ( #53407, #14780 ),
 .UNSPECIFIED., .F., .F.,
 ( 2, 2 ),
 ( 2.168404344971008627E-19, 0.0006430183911724570312 ),
 .UNSPECIFIED. ) ;
#41841 = CARTESIAN_POINT ( 'NONE',  ( -13.70125694970055541, 0.000000000000000000, 7.668437334314234022 ) ) ;
#41842 = DIRECTION ( 'NONE',  ( 0.007781995580012662783, 0.000000000000000000, -0.9999697198139514409 ) ) ;
#41843 = ORIENTED_EDGE ( 'NONE', *, *, #38025, .T. ) ;
#41844 = CARTESIAN_POINT ( 'NONE',  ( -46.28406441860931153, 5.387676038876692886, -5.000000000000000000 ) ) ;
#41845 = CARTESIAN_POINT ( 'NONE',  ( -15.86710544311044302, 0.000000000000000000, 13.13336954653252953 ) ) ;
#41846 = DIRECTION ( 'NONE',  ( 0.007781995580012663651, -3.146120232559066537E-19, -0.9999697198139514409 ) ) ;
#41847 = EDGE_CURVE ( 'NONE', #12635, #17790, #47130, .T. ) ;
#41848 = EDGE_CURVE ( 'NONE', #55458, #22074, #22691, .T. ) ;
#41849 = EDGE_LOOP ( 'NONE', ( #28004, #20180, #37267, #45931 ) ) ;
#41850 = VECTOR ( 'NONE', #35957, 999.9999999999998863 ) ;
#41851 = AXIS2_PLACEMENT_3D ( 'NONE', #54322, #14874, #45507 ) ;
#41852 = DIRECTION ( 'NONE',  ( -0.9999697198139514409, -0.000000000000000000, -0.007781995580013368816 ) ) ;
#41853 = ORIENTED_EDGE ( 'NONE', *, *, #41456, .T. ) ;
#41854 = ADVANCED_FACE ( 'NONE', ( #10187 ), #39750, .F. ) ;
#41855 = ORIENTED_EDGE ( 'NONE', *, *, #22904, .T. ) ;
#41856 = ORIENTED_EDGE ( 'NONE', *, *, #52056, .F. ) ;
#41857 = ORIENTED_EDGE ( 'NONE', *, *, #13209, .T. ) ;
#41858 = VECTOR ( 'NONE', #43596, 999.9999999999998863 ) ;
#41859 = ORIENTED_EDGE ( 'NONE', *, *, #4635, .T. ) ;
#41860 = LINE ( 'NONE', #38169, #55617 ) ;
#41861 = ORIENTED_EDGE ( 'NONE', *, *, #1932, .F. ) ;
#41862 = ORIENTED_EDGE ( 'NONE', *, *, #31751, .T. ) ;
#41863 = CARTESIAN_POINT ( 'NONE',  ( -30.79411802867772607, 0.000000000000000000, 8.643412946479525516 ) ) ;
#41864 = ORIENTED_EDGE ( 'NONE', *, *, #46237, .T. ) ;
#41865 = VECTOR ( 'NONE', #52238, 999.9999999999998863 ) ;
#41866 = ORIENTED_EDGE ( 'NONE', *, *, #1932, .T. ) ;
#41867 = VECTOR ( 'NONE', #41660, 1000.000000000000227 ) ;
#41868 = CARTESIAN_POINT ( 'NONE',  ( -12.13851405436063047, 0.000000000000000000, 11.68505802764555135 ) ) ;
#41869 = CARTESIAN_POINT ( 'NONE',  ( -22.25877225010755822, -3.756034771668159689, 11.49228773929388581 ) ) ;
#41870 = DIRECTION ( 'NONE',  ( 0.8660254037844380415, 0.5000000000000011102, 0.000000000000000000 ) ) ;
#41871 = PLANE ( 'NONE',  #52253 ) ;
#41872 = CARTESIAN_POINT ( 'NONE',  ( -23.33771345073609638, -0.1191753592594197858, 5.846786880686956955 ) ) ;
#41873 = ORIENTED_EDGE ( 'NONE', *, *, #7725, .T. ) ;
#41874 = VERTEX_POINT ( 'NONE', #48234 ) ;
#41875 = DIRECTION ( 'NONE',  ( 0.007781995580012662783, 0.000000000000000000, -0.9999697198139514409 ) ) ;
#41876 = DIRECTION ( 'NONE',  ( -0.005002170337468016433, -0.7660444431189770143, 0.6427681459581293666 ) ) ;
#41877 = ADVANCED_FACE ( 'NONE', ( #5115 ), #30677, .F. ) ;
#41878 = CARTESIAN_POINT ( 'NONE',  ( -38.41289186640547371, 10.48058238645972651, -4.944624203975902077 ) ) ;
#41879 = CARTESIAN_POINT ( 'NONE',  ( -16.81345671998191449, 0.000000000000000000, 3.412238694616132495 ) ) ;
#41880 = EDGE_CURVE ( 'NONE', #30486, #16959, #13356, .T. ) ;
#41881 = CARTESIAN_POINT ( 'NONE',  ( -13.68688668217414239, 0.000000000000000000, 5.821888818025412249 ) ) ;
#41882 = CARTESIAN_POINT ( 'NONE',  ( -20.54204810873173415, 0.000000000000000000, 4.860550213503115558 ) ) ;
#41883 = EDGE_LOOP ( 'NONE', ( #2480, #50043, #28002, #16877 ) ) ;
#41884 = FACE_OUTER_BOUND ( 'NONE', #51548, .T. ) ;
#41885 = EDGE_CURVE ( 'NONE', #39979, #49529, #40005, .T. ) ;
#41886 = ORIENTED_EDGE ( 'NONE', *, *, #37050, .F. ) ;
#41887 = VECTOR ( 'NONE', #7348, 999.9999999999998863 ) ;
#41888 = AXIS2_PLACEMENT_3D ( 'NONE', #1930, #32059, #15026 ) ;
#41889 = PLANE ( 'NONE',  #17998 ) ;
#41890 = LINE ( 'NONE', #52, #34741 ) ;
#41891 = FACE_OUTER_BOUND ( 'NONE', #25475, .T. ) ;
#41892 = FACE_OUTER_BOUND ( 'NONE', #14574, .T. ) ;
#41893 = ADVANCED_FACE ( 'NONE', ( #53083 ), #27510, .F. ) ;
#41894 = CARTESIAN_POINT ( 'NONE',  ( -27.99923088623136636, 0.000000000000000000, 7.757173251277078130 ) ) ;
#41895 = DIRECTION ( 'NONE',  ( -0.9999697198139514409, -0.000000000000000000, -0.007781995580013368816 ) ) ;
#41896 = EDGE_LOOP ( 'NONE', ( #35022, #32647, #51605, #6609 ) ) ;
#41897 = AXIS2_PLACEMENT_3D ( 'NONE', #16761, #51112, #30392 ) ;
#41898 = ORIENTED_EDGE ( 'NONE', *, *, #13718, .F. ) ;
#41899 = DIRECTION ( 'NONE',  ( -0.9335804264972041855, 0.3583679495452941066, 0.000000000000000000 ) ) ;
#41900 = CARTESIAN_POINT ( 'NONE',  ( -10.27421835998572064, 0.000000000000000000, 10.96090226820206048 ) ) ;
#41901 = DIRECTION ( 'NONE',  ( 0.000000000000000000, 0.000000000000000000, -1.000000000000000000 ) ) ;
#41902 = DIRECTION ( 'NONE',  ( 0.000000000000000000, -1.000000000000000000, 0.000000000000000000 ) ) ;
#41903 = VECTOR ( 'NONE', #46145, 1000.000000000000114 ) ;
#41904 = DIRECTION ( 'NONE',  ( 0.9999697198139515519, 0.000000000000000000, 0.007781995580013368816 ) ) ;
#41905 = CARTESIAN_POINT ( 'NONE',  ( -16.33317936670417225, 0.000000000000000000, 13.31440848639340224 ) ) ;
#41906 = PLANE ( 'NONE',  #11085 ) ;
#41907 = PLANE ( 'NONE',  #8802 ) ;
#41908 = DIRECTION ( 'NONE',  ( 0.9999697198139515519, 0.000000000000000000, 0.007781995580013368816 ) ) ;
#41909 = EDGE_CURVE ( 'NONE', #15326, #44124, #43695, .T. ) ;
#41910 = EDGE_CURVE ( 'NONE', #41600, #36024, #30925, .T. ) ;
#41911 = ORIENTED_EDGE ( 'NONE', *, *, #43531, .F. ) ;
#41912 = VECTOR ( 'NONE', #27243, 1000.000000000000227 ) ;
#41913 = EDGE_CURVE ( 'NONE', #1495, #3681, #9657, .T. ) ;
#41914 = ADVANCED_FACE ( 'NONE', ( #44538 ), #22136, .F. ) ;
#41915 = EDGE_LOOP ( 'NONE', ( #37274, #54059, #44149, #2605 ) ) ;
#41916 = ORIENTED_EDGE ( 'NONE', *, *, #6839, .T. ) ;
#41917 = ORIENTED_EDGE ( 'NONE', *, *, #3593, .F. ) ;
#41918 = VERTEX_POINT ( 'NONE', #9076 ) ;
#41919 = AXIS2_PLACEMENT_3D ( 'NONE', #8926, #31027, #22793 ) ;
#41920 = CARTESIAN_POINT ( 'NONE',  ( -11.27310558606116686, -0.1191753592594168437, 7.048672658178141148 ) ) ;
#41921 = LINE ( 'NONE', #29451, #44719 ) ;
#41922 = DIRECTION ( 'NONE',  ( 0.6246952433987893460, 0.7422098413412802076, -0.2426528472758539279 ) ) ;
#41923 = AXIS2_PLACEMENT_3D ( 'NONE', #29738, #51296, #3584 ) ;
#41924 = VECTOR ( 'NONE', #12999, 1000.000000000000114 ) ;
#41925 = ORIENTED_EDGE ( 'NONE', *, *, #30978, .F. ) ;
#41926 = VERTEX_POINT ( 'NONE', #48828 ) ;
#41927 = ORIENTED_EDGE ( 'NONE', *, *, #24751, .T. ) ;
#41928 = FACE_OUTER_BOUND ( 'NONE', #50857, .T. ) ;
#41929 = ORIENTED_EDGE ( 'NONE', *, *, #29606, .F. ) ;
#41930 = ADVANCED_FACE ( 'NONE', ( #36063 ), #17595, .F. ) ;
#41931 = VECTOR ( 'NONE', #19514, 999.9999999999998863 ) ;
#41932 = AXIS2_PLACEMENT_3D ( 'NONE', #53569, #2706, #15780 ) ;
#41933 = CARTESIAN_POINT ( 'NONE',  ( -67.01030352016741176, -8.774176600361034417, 3.370402386379092619 ) ) ;
#41934 = LINE ( 'NONE', #55032, #40056 ) ;
#41935 = CARTESIAN_POINT ( 'NONE',  ( -21.93882065073936261, -3.432230869623161595, 5.293597968971688772 ) ) ;
#41936 = ORIENTED_EDGE ( 'NONE', *, *, #54416, .F. ) ;
#41937 = LINE ( 'NONE', #7307, #35561 ) ;
#41938 = ORIENTED_EDGE ( 'NONE', *, *, #16749, .F. ) ;
#41939 = DIRECTION ( 'NONE',  ( 0.6427681459581294776, -0.7660444431189769032, 0.005002170337467562802 ) ) ;
#41940 = VECTOR ( 'NONE', #7525, 999.9999999999998863 ) ;
#41941 = LINE ( 'NONE', #3046, #36631 ) ;
#41942 = VECTOR ( 'NONE', #30783, 1000.000000000000227 ) ;
#41943 = LINE ( 'NONE', #3048, #45965 ) ;
#41944 = CARTESIAN_POINT ( 'NONE',  ( -8.377443272075408842, 0.000000000000000000, 6.063214190552308480 ) ) ;
#41945 = CARTESIAN_POINT ( 'NONE',  ( -12.23851102634202448, -0.1191753592594197858, 11.68427982808754884 ) ) ;
#41946 = LINE ( 'NONE', #55045, #48475 ) ;
#41947 = LINE ( 'NONE', #34022, #22968 ) ;
#41948 = CARTESIAN_POINT ( 'NONE',  ( 2.072287782118878319, 0.000000000000000000, -2.950529333540147015 ) ) ;
#41949 = VERTEX_POINT ( 'NONE', #52779 ) ;
#41950 = DIRECTION ( 'NONE',  ( 0.000000000000000000, -1.000000000000000000, 0.000000000000000000 ) ) ;
#41951 = ORIENTED_EDGE ( 'NONE', *, *, #51920, .T. ) ;
#41952 = VECTOR ( 'NONE', #34549, 999.9999999999998863 ) ;
#41953 = CARTESIAN_POINT ( 'NONE',  ( -18.34762591811141164, 0.000000000000000000, 7.632278216634138523 ) ) ;
#41954 = LINE ( 'NONE', #55305, #51397 ) ;
#41955 = CARTESIAN_POINT ( 'NONE',  ( 2.072287782118878319, 0.000000000000000000, -2.950529333540147015 ) ) ;
#41956 = ADVANCED_FACE ( 'NONE', ( #566 ), #26973, .F. ) ;
#41957 = VECTOR ( 'NONE', #24128, 1000.000000000000000 ) ;
#41958 = DIRECTION ( 'NONE',  ( 0.7660212471507180654, -0.6427876096865404731, 0.005961354470445141482 ) ) ;
#41959 = PLANE ( 'NONE',  #55817 ) ;
#41960 = CARTESIAN_POINT ( 'NONE',  ( -18.31051089201068294, -5.213152330870664208, 3.827418522002113299 ) ) ;
#41961 = CARTESIAN_POINT ( 'NONE',  ( -5.940636408542258273, 1.485907485055963928, 7.721872716385612259E-14 ) ) ;
#41962 = ORIENTED_EDGE ( 'NONE', *, *, #8559, .F. ) ;
#41963 = LINE ( 'NONE', #4434, #22889 ) ;
#41964 = VECTOR ( 'NONE', #5418, 1000.000000000000227 ) ;
#41965 = DIRECTION ( 'NONE',  ( 0.000000000000000000, -0.000000000000000000, -1.000000000000000000 ) ) ;
#41966 = CARTESIAN_POINT ( 'NONE',  ( -10.00813838035478298, 0.000000000000000000, 10.77830692922518452 ) ) ;
#41967 = CARTESIAN_POINT ( 'NONE',  ( -6.110905869600904872, 1.712176620043476140E-14, -3.600000000000000089 ) ) ;
#41968 = DIRECTION ( 'NONE',  ( -0.8660254037844380415, -0.5000000000000011102, -0.000000000000000000 ) ) ;
#41969 = ADVANCED_FACE ( 'NONE', ( #23272 ), #34932, .F. ) ;
#41970 = AXIS2_PLACEMENT_3D ( 'NONE', #41948, #32608, #33187 ) ;
#41971 = AXIS2_PLACEMENT_3D ( 'NONE', #52528, #38644, #266 ) ;
#41972 = CARTESIAN_POINT ( 'NONE',  ( -10.89044314061178298, 0.000000000000000000, 4.735655178860175063 ) ) ;
#41973 = CARTESIAN_POINT ( 'NONE',  ( -11.13496771895309756, 0.000000000000000000, 2.148427743403817480 ) ) ;
#41974 = ADVANCED_FACE ( 'NONE', ( #39465 ), #9929, .F. ) ;
#41975 = PLANE ( 'NONE',  #16960 ) ;
#41976 = ADVANCED_FACE ( 'NONE', ( #19259 ), #15297, .F. ) ;
#41977 = FACE_OUTER_BOUND ( 'NONE', #39898, .T. ) ;
#41978 = ORIENTED_EDGE ( 'NONE', *, *, #39409, .T. ) ;
#41979 = AXIS2_PLACEMENT_3D ( 'NONE', #17154, #51774, #30211 ) ;
#41980 = PLANE ( 'NONE',  #32157 ) ;
#41981 = AXIS2_PLACEMENT_3D ( 'NONE', #2588, #46578, #45743 ) ;
#41982 = LINE ( 'NONE', #7941, #6929 ) ;
#41983 = ORIENTED_EDGE ( 'NONE', *, *, #13535, .T. ) ;
#41984 = LINE ( 'NONE', #3087, #43157 ) ;
#41985 = CARTESIAN_POINT ( 'NONE',  ( -17.04466509755329184, -3.108426967578160394, 8.404116713615717771 ) ) ;
#41986 = EDGE_CURVE ( 'NONE', #33755, #8726, #19829, .T. ) ;
#41987 = ORIENTED_EDGE ( 'NONE', *, *, #35503, .F. ) ;
#41988 = EDGE_CURVE ( 'NONE', #10050, #3022, #40850, .T. ) ;
#41989 = VECTOR ( 'NONE', #37149, 1000.000000000000227 ) ;
#41990 = ORIENTED_EDGE ( 'NONE', *, *, #33280, .T. ) ;
#41991 = CARTESIAN_POINT ( 'NONE',  ( -19.99049163959727693, 0.000000000000000000, 5.603506693094304936 ) ) ;
#41992 = AXIS2_PLACEMENT_3D ( 'NONE', #40052, #1141, #36105 ) ;
#41993 = EDGE_CURVE ( 'NONE', #17849, #4586, #1926, .T. ) ;
#41994 = VERTEX_POINT ( 'NONE', #32607 ) ;
#41995 = ORIENTED_EDGE ( 'NONE', *, *, #10844, .F. ) ;
#41996 = ORIENTED_EDGE ( 'NONE', *, *, #8153, .F. ) ;
#41997 = CARTESIAN_POINT ( 'NONE',  ( 2.072287782118878319, 0.000000000000000000, -2.950529333540147015 ) ) ;
#41998 = DIRECTION ( 'NONE',  ( 0.007781995580012663651, 0.000000000000000000, -0.9999697198139515519 ) ) ;
#41999 = CARTESIAN_POINT ( 'NONE',  ( -20.41887202388666012, -0.5179957512181557755, 4.796177662602485903 ) ) ;
#42000 = VECTOR ( 'NONE', #21450, 1000.000000000000227 ) ;
#42001 = ADVANCED_FACE ( 'NONE', ( #53903 ), #53624, .F. ) ;
#42002 = ORIENTED_EDGE ( 'NONE', *, *, #39448, .T. ) ;
#42003 = ORIENTED_EDGE ( 'NONE', *, *, #37841, .T. ) ;
#42004 = VECTOR ( 'NONE', #9758, 1000.000000000000227 ) ;
#42005 = EDGE_CURVE ( 'NONE', #38778, #33081, #24095, .T. ) ;
#42006 = CARTESIAN_POINT ( 'NONE',  ( -13.73672976910459909, 0.000000000000000000, 12.22661844811216270 ) ) ;
#42007 = LINE ( 'NONE', #20439, #22737 ) ;
#42008 = ORIENTED_EDGE ( 'NONE', *, *, #32024, .F. ) ;
#42009 = CIRCLE ( 'NONE', #38417, 2.750000000000001776 ) ;
#42010 = DIRECTION ( 'NONE',  ( 0.005961354470445682716, -0.6427876096865404731, -0.7660212471507180654 ) ) ;
#42011 = ORIENTED_EDGE ( 'NONE', *, *, #23422, .T. ) ;
#42012 = FACE_OUTER_BOUND ( 'NONE', #25255, .T. ) ;
#42013 = DIRECTION ( 'NONE',  ( -0.7660212471507179544, -0.6427876096865405842, -0.005961354470445141482 ) ) ;
#42014 = VECTOR ( 'NONE', #13130, 1000.000000000000227 ) ;
#42015 = AXIS2_PLACEMENT_3D ( 'NONE', #54751, #45672, #3375 ) ;
#42016 = ORIENTED_EDGE ( 'NONE', *, *, #10930, .T. ) ;
#42017 = PLANE ( 'NONE',  #2806 ) ;
#42018 = VECTOR ( 'NONE', #38092, 1000.000000000000227 ) ;
#42019 = CARTESIAN_POINT ( 'NONE',  ( 2.072287782118878319, 0.000000000000000000, -2.950529333540147015 ) ) ;
#42020 = VECTOR ( 'NONE', #22393, 999.9999999999998863 ) ;
#42021 = ORIENTED_EDGE ( 'NONE', *, *, #30730, .T. ) ;
#42022 = DIRECTION ( 'NONE',  ( -0.6427681459581293666, -0.7660444431189770143, -0.005002170337467561935 ) ) ;
#42023 =( NAMED_UNIT ( * ) SI_UNIT ( $, .STERADIAN. ) SOLID_ANGLE_UNIT ( ) );
#42024 = LINE ( 'NONE', #19891, #18354 ) ;
#42025 = ORIENTED_EDGE ( 'NONE', *, *, #14912, .F. ) ;
#42026 = DIRECTION ( 'NONE',  ( -0.000000000000000000, -0.000000000000000000, -1.000000000000000000 ) ) ;
#42027 = PLANE ( 'NONE',  #26023 ) ;
#42028 = CARTESIAN_POINT ( 'NONE',  ( -1.086233639165236964, 0.000000000000000000, -2.796443541562362078 ) ) ;
#42029 = EDGE_CURVE ( 'NONE', #41467, #34435, #36313, .T. ) ;
#42030 = CARTESIAN_POINT ( 'NONE',  ( -12.13851405436063047, 0.000000000000000000, 11.68505802764555135 ) ) ;
#42031 = DIRECTION ( 'NONE',  ( -0.005961354470445682716, -0.6427876096865404731, 0.7660212471507180654 ) ) ;
#42032 = DIRECTION ( 'NONE',  ( 0.000000000000000000, -1.000000000000000000, 0.000000000000000000 ) ) ;
#42033 = CARTESIAN_POINT ( 'NONE',  ( -58.00000000000000711, 2.000000000000000000, 7.102951435054649637E-15 ) ) ;
#42034 = VECTOR ( 'NONE', #40435, 1000.000000000000227 ) ;
#42035 = VERTEX_POINT ( 'NONE', #54733 ) ;
#42036 = DIRECTION ( 'NONE',  ( -0.6427681459581293666, -0.7660444431189770143, -0.005002170337467561935 ) ) ;
#42037 = DIRECTION ( 'NONE',  ( 0.000000000000000000, -1.000000000000000000, 0.000000000000000000 ) ) ;
#42038 = CARTESIAN_POINT ( 'NONE',  ( -15.60102546347950536, 0.000000000000000000, 12.95077420755565356 ) ) ;
#42039 = EDGE_LOOP ( 'NONE', ( #12528, #54525, #42227, #49060 ) ) ;
#42040 = PLANE ( 'NONE',  #45629 ) ;
#42041 = DIRECTION ( 'NONE',  ( 0.9999697198139515519, 0.000000000000000000, 0.007781995580013368816 ) ) ;
#42042 = VECTOR ( 'NONE', #47918, 1000.000000000000000 ) ;
#42043 = CARTESIAN_POINT ( 'NONE',  ( -16.81190032086591302, 0.000000000000000000, 3.212244750653343583 ) ) ;
#42044 = VECTOR ( 'NONE', #13824, 999.9999999999998863 ) ;
#42045 = PLANE ( 'NONE',  #26940 ) ;
#42046 = EDGE_CURVE ( 'NONE', #46955, #47606, #23797, .T. ) ;
#42047 = CARTESIAN_POINT ( 'NONE',  ( -55.84246788140315942, 5.810395100437911076, -3.000000000000007105 ) ) ;
#42048 = ORIENTED_EDGE ( 'NONE', *, *, #46781, .F. ) ;
#42049 = ORIENTED_EDGE ( 'NONE', *, *, #21812, .T. ) ;
#42050 = PLANE ( 'NONE',  #23224 ) ;
#42051 = AXIS2_PLACEMENT_3D ( 'NONE', #20197, #53465, #14566 ) ;
#42052 = AXIS2_PLACEMENT_3D ( 'NONE', #10492, #6777, #37150 ) ;
#42053 = DIRECTION ( 'NONE',  ( -0.5449076811759708816, 0.6444004775717707689, 0.5364919789714475140 ) ) ;
#42054 = EDGE_LOOP ( 'NONE', ( #33763, #16771, #52623, #16161 ) ) ;
#42055 = EDGE_CURVE ( 'NONE', #25116, #235, #28638, .T. ) ;
#42056 = FACE_OUTER_BOUND ( 'NONE', #800, .T. ) ;
#42057 = EDGE_LOOP ( 'NONE', ( #54737, #55252 ) ) ;
#42058 = CARTESIAN_POINT ( 'NONE',  ( -19.06210475032114360, -1.651309408375657428, 6.796380631735580380 ) ) ;
#42059 = EDGE_CURVE ( 'NONE', #34091, #32088, #19552, .T. ) ;
#42060 = VECTOR ( 'NONE', #47807, 1000.000000000000000 ) ;
#42061 = ORIENTED_EDGE ( 'NONE', *, *, #49291, .F. ) ;
#42062 = VECTOR ( 'NONE', #41832, 1000.000000000000227 ) ;
#42063 = ORIENTED_EDGE ( 'NONE', *, *, #6380, .T. ) ;
#42064 = ORIENTED_EDGE ( 'NONE', *, *, #7271, .T. ) ;
#42065 = LINE ( 'NONE', #24744, #4826 ) ;
#42066 = CARTESIAN_POINT ( 'NONE',  ( -24.26908309836554878, 0.000000000000000000, 6.108867788427308376 ) ) ;
#42067 = CARTESIAN_POINT ( 'NONE',  ( -14.66887761629205222, 0.000000000000000000, 12.58869632783390990 ) ) ;
#42068 = EDGE_CURVE ( 'NONE', #37968, #16268, #49669, .T. ) ;
#42069 = PLANE ( 'NONE',  #371 ) ;
#42070 = ORIENTED_EDGE ( 'NONE', *, *, #9501, .F. ) ;
#42071 = ORIENTED_EDGE ( 'NONE', *, *, #33192, .T. ) ;
#42072 = AXIS2_PLACEMENT_3D ( 'NONE', #23857, #54503, #41725 ) ;
#42073 = ADVANCED_FACE ( 'NONE', ( #28071 ), #54198, .F. ) ;
#42074 = ORIENTED_EDGE ( 'NONE', *, *, #48875, .F. ) ;
#42075 = FACE_OUTER_BOUND ( 'NONE', #6289, .T. ) ;
#42076 = AXIS2_PLACEMENT_3D ( 'NONE', #53468, #35895, #10314 ) ;
#42077 = DIRECTION ( 'NONE',  ( -0.7660212471507179544, -0.6427876096865405842, -0.005961354470445141482 ) ) ;
#42078 = EDGE_LOOP ( 'NONE', ( #37286, #14384, #39866, #42973 ) ) ;
#42079 = CARTESIAN_POINT ( 'NONE',  ( -20.54049170961573267, 0.000000000000000000, 4.660556269540326646 ) ) ;
#42080 = ORIENTED_EDGE ( 'NONE', *, *, #11788, .T. ) ;
#42081 = AXIS2_PLACEMENT_3D ( 'NONE', #55503, #21460, #16611 ) ;
#42082 = DIRECTION ( 'NONE',  ( 0.9999697198139515519, 0.000000000000000000, 0.007781995580013368816 ) ) ;
#42083 = CARTESIAN_POINT ( 'NONE',  ( -27.56484202182514665, 16.74370688441070953, -4.657437592157546824 ) ) ;
#42084 = VERTEX_POINT ( 'NONE', #45655 ) ;
#42085 = DIRECTION ( 'NONE',  ( 0.7660212471507180654, -0.6427876096865404731, 0.005961354470445141482 ) ) ;
#42086 = AXIS2_PLACEMENT_3D ( 'NONE', #17820, #3611, #43084 ) ;
#42087 = ORIENTED_EDGE ( 'NONE', *, *, #52736, .T. ) ;
#42088 = CARTESIAN_POINT ( 'NONE',  ( -22.36868959911851462, 19.74370688441071309, 4.433756599430258127 ) ) ;
#42089 = DIRECTION ( 'NONE',  ( 0.9999697198139515519, 0.000000000000000000, 0.007781995580013368816 ) ) ;
#42090 = CARTESIAN_POINT ( 'NONE',  ( -24.26986129792355129, -0.1191753592594197858, 6.208864760408702388 ) ) ;
#42091 = LINE ( 'NONE', #41547, #10294 ) ;
#42092 = DIRECTION ( 'NONE',  ( -0.5449076811759708816, 0.6444004775717707689, 0.5364919789714475140 ) ) ;
#42093 = AXIS2_PLACEMENT_3D ( 'NONE', #16731, #2804, #12494 ) ;
#42094 = CARTESIAN_POINT ( 'NONE',  ( -19.06828360731494953, 0.000000000000000000, 6.518673682440828898 ) ) ;
#42095 = ORIENTED_EDGE ( 'NONE', *, *, #15953, .F. ) ;
#42096 = EDGE_CURVE ( 'NONE', #9862, #37828, #41423, .T. ) ;
#42097 = VECTOR ( 'NONE', #46090, 1000.000000000000227 ) ;
#42098 = ORIENTED_EDGE ( 'NONE', *, *, #20395, .T. ) ;
#42099 = DIRECTION ( 'NONE',  ( 0.9999697198139515519, 0.000000000000000000, 0.007781995580013368816 ) ) ;
#42100 = CARTESIAN_POINT ( 'NONE',  ( -25.20278734466900517, 0.000000000000000000, 6.670939612111840944 ) ) ;
#42101 = ADVANCED_FACE ( 'NONE', ( #14730 ), #11597, .F. ) ;
#42102 = LINE ( 'NONE', #40230, #39475 ) ;
#42103 = LINE ( 'NONE', #25094, #25825 ) ;
#42104 = PLANE ( 'NONE',  #36980 ) ;
#42105 = AXIS2_PLACEMENT_3D ( 'NONE', #44248, #31481, #44500 ) ;
#42106 = VECTOR ( 'NONE', #8919, 999.9999999999998863 ) ;
#42107 = EDGE_CURVE ( 'NONE', #54123, #11442, #15549, .T. ) ;
#42108 = DIRECTION ( 'NONE',  ( -0.7660212471507179544, -0.6427876096865405842, -0.005961354470445141482 ) ) ;
#42109 = ORIENTED_EDGE ( 'NONE', *, *, #53010, .T. ) ;
#42110 = EDGE_CURVE ( 'NONE', #33688, #5158, #11306, .T. ) ;
#42111 = PLANE ( 'NONE',  #28621 ) ;
#42112 = LINE ( 'NONE', #34184, #44088 ) ;
#42113 = ORIENTED_EDGE ( 'NONE', *, *, #45563, .F. ) ;
#42114 = LINE ( 'NONE', #15430, #27678 ) ;
#42115 = ORIENTED_EDGE ( 'NONE', *, *, #30412, .F. ) ;
#42116 = ADVANCED_FACE ( 'NONE', ( #1669 ), #18996, .F. ) ;
#42117 = EDGE_CURVE ( 'NONE', #31264, #40953, #50758, .T. ) ;
#42118 = EDGE_CURVE ( 'NONE', #16969, #27886, #43101, .T. ) ;
#42119 = CARTESIAN_POINT ( 'NONE',  ( -15.86710544311044302, 0.000000000000000000, 13.13336954653252953 ) ) ;
#42120 = DIRECTION ( 'NONE',  ( 0.007781995580012662783, 0.000000000000000000, -0.9999697198139514409 ) ) ;
#42121 = CARTESIAN_POINT ( 'NONE',  ( -21.62239062191499528, 2.229229656569007290, 8.938737581926881504 ) ) ;
#42122 = DIRECTION ( 'NONE',  ( 0.000000000000000000, -0.000000000000000000, -1.000000000000000000 ) ) ;
#42123 = CARTESIAN_POINT ( 'NONE',  ( -69.14139375802285770, 2.000000000002681855, -6.539696485998404363 ) ) ;
#42124 = AXIS2_PLACEMENT_3D ( 'NONE', #47660, #30340, #787 ) ;
#42125 = ORIENTED_EDGE ( 'NONE', *, *, #24140, .F. ) ;
#42126 = ORIENTED_EDGE ( 'NONE', *, *, #55203, .T. ) ;
#42127 = VECTOR ( 'NONE', #55944, 1000.000000000000227 ) ;
#42128 = LINE ( 'NONE', #39270, #39419 ) ;
#42129 = DIRECTION ( 'NONE',  ( 0.7660212471507180654, -0.6427876096865404731, 0.005961354470445141482 ) ) ;
#42130 = CARTESIAN_POINT ( 'NONE',  ( -12.75186478148140523, 0.000000000000000000, 5.090501235045900685 ) ) ;
#42131 = AXIS2_PLACEMENT_3D ( 'NONE', #43773, #48894, #40375 ) ;
#42132 = CARTESIAN_POINT ( 'NONE',  ( -28.93137873341882127, 0.000000000000000000, 8.119251130998824451 ) ) ;
#42133 = CARTESIAN_POINT ( 'NONE',  ( -18.81094516056321808, 0.000000000000000000, 7.459346545571152731 ) ) ;
#42134 = ADVANCED_FACE ( 'NONE', ( #25773 ), #7914, .F. ) ;
#42135 = DIRECTION ( 'NONE',  ( 0.005002170337468016433, -0.7660444431189770143, -0.6427681459581293666 ) ) ;
#42136 = VECTOR ( 'NONE', #9074, 1000.000000000000000 ) ;
#42137 = VERTEX_POINT ( 'NONE', #3362 ) ;
#42138 = CARTESIAN_POINT ( 'NONE',  ( 2.072287782118878319, 0.000000000000000000, -2.950529333540147015 ) ) ;
#42139 = EDGE_CURVE ( 'NONE', #38521, #7991, #25484, .T. ) ;
#42140 = LINE ( 'NONE', #50668, #20575 ) ;
#42141 = CARTESIAN_POINT ( 'NONE',  ( 2.072287782118878319, 0.000000000000000000, -2.950529333540147015 ) ) ;
#42143 = ORIENTED_EDGE ( 'NONE', *, *, #28012, .F. ) ;
#42142 = AXIS2_PLACEMENT_3D ( 'NONE', #41879, #4138, #3562 ) ;
#42144 = EDGE_CURVE ( 'NONE', #27017, #38106, #21532, .T. ) ;
#42145 = AXIS2_PLACEMENT_3D ( 'NONE', #18924, #23463, #24472 ) ;
#42146 = CARTESIAN_POINT ( 'NONE',  ( -68.63426800804415961, -10.92493131198209078, 7.487487041937088250 ) ) ;
#42147 = CARTESIAN_POINT ( 'NONE',  ( -56.75000000000000711, 4.550000000000001599, 2.449489742783185875 ) ) ;
#42148 = DIRECTION ( 'NONE',  ( 0.6427681459581294776, -0.7660444431189769032, 0.005002170337467562802 ) ) ;
#42149 = AXIS2_PLACEMENT_3D ( 'NONE', #14474, #35774, #17907 ) ;
#42150 = ORIENTED_EDGE ( 'NONE', *, *, #47303, .T. ) ;
#42151 = EDGE_CURVE ( 'NONE', #24739, #4654, #7603, .T. ) ;
#42152 = CARTESIAN_POINT ( 'NONE',  ( -16.96676784072528932, 0.000000000000000000, 9.320358708932014125 ) ) ;
#42153 = EDGE_LOOP ( 'NONE', ( #46236, #11717, #22816, #3869 ) ) ;
#42154 = VECTOR ( 'NONE', #44945, 1000.000000000000227 ) ;
#42155 = EDGE_LOOP ( 'NONE', ( #6992, #8010, #30767, #37415 ) ) ;
#42156 = CIRCLE ( 'NONE', #44023, 2.000000000000001776 ) ;
#42157 = ORIENTED_EDGE ( 'NONE', *, *, #32062, .F. ) ;
#42158 = EDGE_LOOP ( 'NONE', ( #13783, #47468, #8098, #22379, #3454 ) ) ;
#42159 = CARTESIAN_POINT ( 'NONE',  ( -20.54126990917373519, -0.1191753592594197858, 4.760553241521720658 ) ) ;
#42160 = EDGE_LOOP ( 'NONE', ( #8451, #3027, #30065, #18507 ) ) ;
#42161 = B_SPLINE_CURVE_WITH_KNOTS ( 'NONE', 3,
 ( #48622, #31294, #18503, #9733, #27040, #35846, #40664, #53169, #14529, #14277 ),
 .UNSPECIFIED., .F., .F.,
 ( 4, 2, 2, 2, 4 ),
 ( 0.000000000000000000, 0.0003339141718491685099, 0.0006678283436983370198, 0.001001742515547505638, 0.001335656687396674040 ),
 .UNSPECIFIED. ) ;
#42162 = EDGE_LOOP ( 'NONE', ( #12340, #24840, #51201, #26127 ) ) ;
#42163 = DIRECTION ( 'NONE',  ( 0.3535533905932752297, -0.6123724356957952475, -0.7071067811865462405 ) ) ;
#42164 = ORIENTED_EDGE ( 'NONE', *, *, #37981, .T. ) ;
#42165 = ORIENTED_EDGE ( 'NONE', *, *, #960, .T. ) ;
#42166 = VECTOR ( 'NONE', #53515, 1000.000000000000227 ) ;
#42167 = CARTESIAN_POINT ( 'NONE',  ( -19.39493078104614909, -2.774784975051975966, 7.711734769794177602 ) ) ;
#42168 = CLOSED_SHELL ( 'NONE', ( #39291, #12705, #3473, #43879, #35343, #10786, #41194, #16831, #48753, #23492, #11426, #39334, #446, #5049 ) ) ;
#42169 = DIRECTION ( 'NONE',  ( -0.000000000000000000, -0.000000000000000000, -1.000000000000000000 ) ) ;
#42170 = DIRECTION ( 'NONE',  ( 0.5000000000000011102, -0.8660254037844380415, 0.000000000000000000 ) ) ;
#42171 = LINE ( 'NONE', #34488, #36864 ) ;
#42172 = SURFACE_STYLE_FILL_AREA ( #12377 ) ;
#42173 = VECTOR ( 'NONE', #51816, 1000.000000000000227 ) ;
#42174 = ORIENTED_EDGE ( 'NONE', *, *, #42192, .F. ) ;
#42175 = ORIENTED_EDGE ( 'NONE', *, *, #37366, .T. ) ;
#42176 = LINE ( 'NONE', #16322, #35850 ) ;
#42177 = FACE_OUTER_BOUND ( 'NONE', #12175, .T. ) ;
#42178 = VECTOR ( 'NONE', #8601, 1000.000000000000227 ) ;
#42179 = UNCERTAINTY_MEASURE_WITH_UNIT (LENGTH_MEASURE( 1.000000000000000082E-05 ), #39762, 'distance_accuracy_value', 'NONE');
#42180 = FACE_OUTER_BOUND ( 'NONE', #45328, .T. ) ;
#42181 = VECTOR ( 'NONE', #21542, 1000.000000000000227 ) ;
#42182 = VECTOR ( 'NONE', #32742, 999.9999999999998863 ) ;
#42183 = CARTESIAN_POINT ( 'NONE',  ( -11.67244013076689946, 0.000000000000000000, 11.50401908778467863 ) ) ;
#42184 = VECTOR ( 'NONE', #36687, 1000.000000000000227 ) ;
#42185 = CARTESIAN_POINT ( 'NONE',  ( -23.33849165029409889, 0.000000000000000000, 5.946783852668351855 ) ) ;
#42186 = DIRECTION ( 'NONE',  ( 0.7660212471507180654, -0.6427876096865404731, 0.005961354470445141482 ) ) ;
#42187 = ORIENTED_EDGE ( 'NONE', *, *, #14705, .T. ) ;
#42188 = DIRECTION ( 'NONE',  ( 0.000000000000000000, 0.000000000000000000, 1.000000000000000000 ) ) ;
#42189 = CARTESIAN_POINT ( 'NONE',  ( -21.57134263578401701, 2.714935509636507316, 9.716034862368092107 ) ) ;
#42190 = ORIENTED_EDGE ( 'NONE', *, *, #44959, .F. ) ;
#42191 = VECTOR ( 'NONE', #22388, 1000.000000000000227 ) ;
#42192 = EDGE_CURVE ( 'NONE', #41253, #52332, #56157, .T. ) ;
#42193 = EDGE_CURVE ( 'NONE', #11442, #49751, #29478, .T. ) ;
#42194 = CARTESIAN_POINT ( 'NONE',  ( -20.26176469941677993, 0.000000000000000000, 14.76116360616437895 ) ) ;
#42195 = DIRECTION ( 'NONE',  ( 0.007781995580012662783, 0.000000000000000000, -0.9999697198139514409 ) ) ;
#42196 = CARTESIAN_POINT ( 'NONE',  ( -14.66887761629205222, 0.000000000000000000, 12.58869632783390990 ) ) ;
#42197 = LINE ( 'NONE', #38795, #50424 ) ;
#42198 = EDGE_CURVE ( 'NONE', #5857, #16502, #3898, .T. ) ;
#42199 = CARTESIAN_POINT ( 'NONE',  ( -16.81190032086591302, 0.000000000000000000, 3.212244750653343583 ) ) ;
#42200 = AXIS2_PLACEMENT_3D ( 'NONE', #1961, #27547, #53126 ) ;
#42201 = VERTEX_POINT ( 'NONE', #12995 ) ;
#42202 = AXIS2_PLACEMENT_3D ( 'NONE', #4613, #43267, #48053 ) ;
#42203 = ORIENTED_EDGE ( 'NONE', *, *, #9094, .F. ) ;
#42204 = FACE_OUTER_BOUND ( 'NONE', #26762, .T. ) ;
#42205 = CARTESIAN_POINT ( 'NONE',  ( -20.42601593468891963, 20.86531004751671148, 4.315323051534361021 ) ) ;
#42206 = PLANE ( 'NONE',  #21529 ) ;
#42207 = LINE ( 'NONE', #50152, #18265 ) ;
#42208 = DIRECTION ( 'NONE',  ( 0.5364919789714477361, 0.6444004775717706579, 0.5449076811759711036 ) ) ;
#42209 = DIRECTION ( 'NONE',  ( 0.005961354470445682716, -0.6427876096865404731, -0.7660212471507180654 ) ) ;
#42210 = LINE ( 'NONE', #29136, #49195 ) ;
#42211 = VECTOR ( 'NONE', #52413, 1000.000000000000227 ) ;
#42212 = LINE ( 'NONE', #49695, #9636 ) ;
#42213 = CARTESIAN_POINT ( 'NONE',  ( -70.57579075201010710, -8.781267840485488918, 8.554889286408839055 ) ) ;
#42214 = VECTOR ( 'NONE', #30705, 1000.000000000000000 ) ;
#42215 = EDGE_CURVE ( 'NONE', #25458, #33250, #12793, .T. ) ;
#42216 = DIRECTION ( 'NONE',  ( -0.005002170337468016433, -0.7660444431189770143, 0.6427681459581293666 ) ) ;
#42217 = ORIENTED_EDGE ( 'NONE', *, *, #1429, .T. ) ;
#42218 = DIRECTION ( 'NONE',  ( 0.000000000000000000, -1.000000000000000000, 0.000000000000000000 ) ) ;
#42219 = VECTOR ( 'NONE', #50363, 1000.000000000000227 ) ;
#42220 = EDGE_LOOP ( 'NONE', ( #45830, #18121, #41222 ) ) ;
#42221 = ADVANCED_FACE ( 'NONE', ( #17241 ), #8175, .F. ) ;
#42222 = VECTOR ( 'NONE', #8527, 999.9999999999998863 ) ;
#42223 = ORIENTED_EDGE ( 'NONE', *, *, #51726, .T. ) ;
#42224 = VERTEX_POINT ( 'NONE', #51877 ) ;
#42225 = AXIS2_PLACEMENT_3D ( 'NONE', #40970, #49784, #28186 ) ;
#42226 = AXIS2_PLACEMENT_3D ( 'NONE', #14023, #8429, #40710 ) ;
#42227 = ORIENTED_EDGE ( 'NONE', *, *, #17435, .F. ) ;
#42228 = ORIENTED_EDGE ( 'NONE', *, *, #53223, .F. ) ;
#42229 = DIRECTION ( 'NONE',  ( 0.5364919789714477361, 0.6444004775717706579, 0.5449076811759711036 ) ) ;
#42230 = DIRECTION ( 'NONE',  ( 0.9999697198139515519, 0.000000000000000000, 0.007781995580013368816 ) ) ;
#42231 = ADVANCED_FACE ( 'NONE', ( #16988 ), #30318, .F. ) ;
#42232 = CARTESIAN_POINT ( 'NONE',  ( -68.45424121227161152, -0.05181598292322161375, 7.468591521940118660 ) ) ;
#42233 = VECTOR ( 'NONE', #45013, 1000.000000000000000 ) ;
#42234 = VECTOR ( 'NONE', #38311, 1000.000000000000227 ) ;
#42235 = ORIENTED_EDGE ( 'NONE', *, *, #14291, .T. ) ;
#42236 = FACE_OUTER_BOUND ( 'NONE', #53611, .T. ) ;
#42237 = VECTOR ( 'NONE', #38869, 1000.000000000000000 ) ;
#42238 = EDGE_LOOP ( 'NONE', ( #12073, #48155, #47182, #23711 ) ) ;
#42239 = CARTESIAN_POINT ( 'NONE',  ( -66.08148974733411762, -11.28554828561908074, -6.315096454939365778 ) ) ;
#42240 = VERTEX_POINT ( 'NONE', #20680 ) ;
#42241 = VECTOR ( 'NONE', #51524, 1000.000000000000227 ) ;
#42242 = VECTOR ( 'NONE', #35425, 1000.000000000000114 ) ;
#42243 = CARTESIAN_POINT ( 'NONE',  ( -65.14865909603261684, -9.165469450123071127, -1.520040349670753743 ) ) ;
#42244 = FACE_OUTER_BOUND ( 'NONE', #42162, .T. ) ;
#42245 = CARTESIAN_POINT ( 'NONE',  ( -18.25702930620386866, -0.1191753592594153865, 8.840982497946823671 ) ) ;
#42246 = VERTEX_POINT ( 'NONE', #8759 ) ;
#42247 = FACE_OUTER_BOUND ( 'NONE', #24609, .T. ) ;
#42248 = ORIENTED_EDGE ( 'NONE', *, *, #13321, .T. ) ;
#42249 = CARTESIAN_POINT ( 'NONE',  ( -22.40478740399063895, 0.000000000000000000, 5.384712028983816623 ) ) ;
#42250 = CARTESIAN_POINT ( 'NONE',  ( -13.10291263837268616, -0.1191753592594188005, 3.341111978528461535 ) ) ;
#42251 = AXIS2_PLACEMENT_3D ( 'NONE', #10291, #32160, #53451 ) ;
#42252 = DIRECTION ( 'NONE',  ( -0.5364919789714478471, 0.6444004775717705469, -0.5449076811759709926 ) ) ;
#42253 = DIRECTION ( 'NONE',  ( -0.005961354470445682716, -0.6427876096865404731, 0.7660212471507180654 ) ) ;
#42254 = PLANE ( 'NONE',  #47581 ) ;
#42255 = LINE ( 'NONE', #34307, #14024 ) ;
#42256 = DIRECTION ( 'NONE',  ( -0.9999697198139514409, -0.000000000000000000, -0.007781995580013368816 ) ) ;
#42257 = FACE_OUTER_BOUND ( 'NONE', #6630, .T. ) ;
#42258 = ORIENTED_EDGE ( 'NONE', *, *, #45773, .T. ) ;
#42259 = FACE_OUTER_BOUND ( 'NONE', #21108, .T. ) ;
#42260 = VERTEX_POINT ( 'NONE', #46798 ) ;
#42261 = VECTOR ( 'NONE', #10060, 999.9999999999998863 ) ;
#42262 = EDGE_CURVE ( 'NONE', #16329, #21409, #41946, .T. ) ;
#42263 = CARTESIAN_POINT ( 'NONE',  ( -19.51337669467617530, -3.270328918600659218, 9.628756819687440682 ) ) ;
#42264 = LINE ( 'NONE', #45967, #48685 ) ;
#42265 = DIRECTION ( 'NONE',  ( -0.6427681459581293666, -0.7660444431189770143, -0.005002170337467561935 ) ) ;
#42266 = VECTOR ( 'NONE', #6500, 1000.000000000000114 ) ;
#42267 = PLANE ( 'NONE',  #50321 ) ;
#42268 = PLANE ( 'NONE',  #24970 ) ;
#42269 = EDGE_CURVE ( 'NONE', #42663, #48737, #3051, .T. ) ;
#42270 = EDGE_CURVE ( 'NONE', #18631, #28691, #42255, .T. ) ;
#42271 = VECTOR ( 'NONE', #45383, 1000.000000000000114 ) ;
#42273 = VECTOR ( 'NONE', #28475, 1000.000000000000227 ) ;
#42272 = DIRECTION ( 'NONE',  ( 0.9999697198139515519, 0.000000000000000000, 0.007781995580013368816 ) ) ;
#42274 = ORIENTED_EDGE ( 'NONE', *, *, #13487, .T. ) ;
#42275 = CARTESIAN_POINT ( 'NONE',  ( -15.92522266148258936, -0.1191753592594200495, 7.751132947013579688 ) ) ;
#42276 = FACE_OUTER_BOUND ( 'NONE', #15097, .T. ) ;
#42277 = DIRECTION ( 'NONE',  ( 0.007781995580012662783, 0.000000000000000000, -0.9999697198139514409 ) ) ;
#42278 = LINE ( 'NONE', #20700, #54475 ) ;
#42279 = VECTOR ( 'NONE', #10210, 1000.000000000000227 ) ;
#42280 = VECTOR ( 'NONE', #54186, 1000.000000000000000 ) ;
#42281 = PLANE ( 'NONE',  #46341 ) ;
#42282 = DIRECTION ( 'NONE',  ( -0.005961354470445682716, -0.6427876096865404731, 0.7660212471507180654 ) ) ;
#42283 = PLANE ( 'NONE',  #39629 ) ;
#42284 = LINE ( 'NONE', #50526, #18353 ) ;
#42285 = EDGE_CURVE ( 'NONE', #4739, #43397, #55297, .T. ) ;
#42286 = VERTEX_POINT ( 'NONE', #51032 ) ;
#42287 = AXIS2_PLACEMENT_3D ( 'NONE', #50016, #54550, #44649 ) ;
#42289 = CARTESIAN_POINT ( 'NONE',  ( -10.82076189722203452, -0.1191753592594203132, 7.421524971165663231 ) ) ;
#42288 = VECTOR ( 'NONE', #35034, 999.9999999999998863 ) ;
#42290 = CARTESIAN_POINT ( 'NONE',  ( -9.968473853056176281, 0.000000000000000000, 5.681500352874511606 ) ) ;
#42291 = ORIENTED_EDGE ( 'NONE', *, *, #43627, .F. ) ;
#42292 = VERTEX_POINT ( 'NONE', #4481 ) ;
#42293 = DIRECTION ( 'NONE',  ( -0.9999697198139514409, -0.000000000000000000, -0.007781995580013368816 ) ) ;
#42294 = VERTEX_POINT ( 'NONE', #26324 ) ;
#42295 = ORIENTED_EDGE ( 'NONE', *, *, #48482, .T. ) ;
#42296 = CARTESIAN_POINT ( 'NONE',  ( -9.938176918887348776, 0.000000000000000000, 1.788409376334078926 ) ) ;
#42297 = EDGE_CURVE ( 'NONE', #32592, #20518, #26912, .T. ) ;
#42298 = VECTOR ( 'NONE', #55539, 1000.000000000000227 ) ;
#42299 = EDGE_LOOP ( 'NONE', ( #55051, #40463, #9699, #41403 ) ) ;
#42300 = ORIENTED_EDGE ( 'NONE', *, *, #14777, .F. ) ;
#42301 = EDGE_LOOP ( 'NONE', ( #11714, #13657, #45923, #5166 ) ) ;
#42302 = EDGE_CURVE ( 'NONE', #24756, #34349, #10650, .T. ) ;
#42303 = LINE ( 'NONE', #47108, #52938 ) ;
#42304 = FACE_OUTER_BOUND ( 'NONE', #30998, .T. ) ;
#42305 = VECTOR ( 'NONE', #20478, 999.9999999999998863 ) ;
#42306 = CARTESIAN_POINT ( 'NONE',  ( -14.94760462649100496, 0.000000000000000000, 2.488088991209854051 ) ) ;
#42307 = VECTOR ( 'NONE', #17267, 1000.000000000000227 ) ;
#42308 = ORIENTED_EDGE ( 'NONE', *, *, #39138, .T. ) ;
#42309 = EDGE_CURVE ( 'NONE', #9132, #35388, #40986, .T. ) ;
#42310 = EDGE_LOOP ( 'NONE', ( #7119, #19689, #12367, #14014 ) ) ;
#42311 = AXIS2_PLACEMENT_3D ( 'NONE', #9027, #4223, #26613 ) ;
#42312 = PLANE ( 'NONE',  #25728 ) ;
#42313 = CARTESIAN_POINT ( 'NONE',  ( -15.48665731996427475, -0.1941918491731561003, 3.016177271524973946 ) ) ;
#42314 = ORIENTED_EDGE ( 'NONE', *, *, #14279, .T. ) ;
#42315 = DIRECTION ( 'NONE',  ( -0.005002170337468016433, -0.7660444431189770143, 0.6427681459581293666 ) ) ;
#42316 = ORIENTED_EDGE ( 'NONE', *, *, #16790, .F. ) ;
#42317 = LINE ( 'NONE', #3413, #38479 ) ;
#42318 = DIRECTION ( 'NONE',  ( -0.5449076811759708816, 0.6444004775717707689, 0.5364919789714475140 ) ) ;
#42319 = ORIENTED_EDGE ( 'NONE', *, *, #3144, .F. ) ;
#42320 = VECTOR ( 'NONE', #2063, 1000.000000000000227 ) ;
#42321 = DIRECTION ( 'NONE',  ( 0.005961354470445682716, -0.6427876096865404731, -0.7660212471507180654 ) ) ;
#42322 = EDGE_CURVE ( 'NONE', #26568, #13781, #19405, .T. ) ;
#42323 = VECTOR ( 'NONE', #31494, 999.9999999999998863 ) ;
#42324 = CARTESIAN_POINT ( 'NONE',  ( -14.59185039342477275, 0.000000000000000000, 2.690863609132300827 ) ) ;
#42325 = VECTOR ( 'NONE', #9375, 999.9999999999998863 ) ;
#42326 = VERTEX_POINT ( 'NONE', #21790 ) ;
#42327 = CARTESIAN_POINT ( 'NONE',  ( -14.00280974873554030, 0.000000000000000000, 12.40921378708904044 ) ) ;
#42328 = DIRECTION ( 'NONE',  ( 0.000000000000000000, -0.000000000000000000, -1.000000000000000000 ) ) ;
#42329 = CARTESIAN_POINT ( 'NONE',  ( -14.37176155590648285, -4.889348428825662118, 10.28866572930882839 ) ) ;
#42330 = LINE ( 'NONE', #37208, #12929 ) ;
#42331 = EDGE_CURVE ( 'NONE', #51378, #55644, #36745, .T. ) ;
#42332 = VERTEX_POINT ( 'NONE', #47923 ) ;
#42333 = EDGE_CURVE ( 'NONE', #21510, #41396, #5328, .T. ) ;
#42334 = DIRECTION ( 'NONE',  ( 0.000000000000000000, -0.000000000000000000, -1.000000000000000000 ) ) ;
#42335 = PLANE ( 'NONE',  #47779 ) ;
#42336 = CARTESIAN_POINT ( 'NONE',  ( -55.47117325737978888, 6.581829179614757663, 1.080525476705103127 ) ) ;
#42337 = CARTESIAN_POINT ( 'NONE',  ( -16.81190032086591302, 0.000000000000000000, 3.212244750653343583 ) ) ;
#42338 = FACE_OUTER_BOUND ( 'NONE', #18780, .T. ) ;
#42339 = EDGE_CURVE ( 'NONE', #3658, #22349, #3349, .T. ) ;
#42340 = LINE ( 'NONE', #20749, #50619 ) ;
#42341 = VECTOR ( 'NONE', #32960, 999.9999999999998863 ) ;
#42342 = CARTESIAN_POINT ( 'NONE',  ( -14.94760462649100496, 0.000000000000000000, 2.488088991209854051 ) ) ;
#42343 = ORIENTED_EDGE ( 'NONE', *, *, #35734, .F. ) ;
#42344 = LINE ( 'NONE', #41211, #28046 ) ;
#42345 = CARTESIAN_POINT ( 'NONE',  ( -68.36985609944017028, -0.6011933878353118432, 5.577208301935089096 ) ) ;
#42346 = EDGE_LOOP ( 'NONE', ( #7583, #2133, #44565, #4785 ) ) ;
#42347 = DIRECTION ( 'NONE',  ( -0.9999697198139514409, -0.000000000000000000, -0.007781995580013368816 ) ) ;
#42348 = DIRECTION ( 'NONE',  ( -0.5449076811759708816, 0.6444004775717707689, 0.5364919789714475140 ) ) ;
#42349 = ADVANCED_FACE ( 'NONE', ( #35414 ), #52175, .F. ) ;
#42350 = VECTOR ( 'NONE', #28520, 999.9999999999998863 ) ;
#42351 = LINE ( 'NONE', #7148, #13176 ) ;
#42352 = DIRECTION ( 'NONE',  ( 0.005961354470445682716, -0.6427876096865404731, -0.7660212471507180654 ) ) ;
#42353 = DIRECTION ( 'NONE',  ( 0.9999697198139515519, 0.000000000000000000, 0.007781995580013368816 ) ) ;
#42354 = EDGE_CURVE ( 'NONE', #38710, #20039, #13291, .T. ) ;
#42355 = ORIENTED_EDGE ( 'NONE', *, *, #16323, .T. ) ;
#42356 = AXIS2_PLACEMENT_3D ( 'NONE', #46735, #25428, #42736 ) ;
#42357 = ORIENTED_EDGE ( 'NONE', *, *, #923, .F. ) ;
#42358 = DIRECTION ( 'NONE',  ( 0.007781995580012663651, -3.146120232559066537E-19, -0.9999697198139514409 ) ) ;
#42359 = DIRECTION ( 'NONE',  ( 0.5364919789714477361, 0.6444004775717706579, 0.5449076811759711036 ) ) ;
#42360 = DIRECTION ( 'NONE',  ( 0.000000000000000000, -1.000000000000000000, 0.000000000000000000 ) ) ;
#42361 = VECTOR ( 'NONE', #49666, 1000.000000000000227 ) ;
#42362 = VERTEX_POINT ( 'NONE', #15178 ) ;
#42363 = DIRECTION ( 'NONE',  ( 0.9999697198139515519, 0.000000000000000000, 0.007781995580013368816 ) ) ;
#42364 = VERTEX_POINT ( 'NONE', #43924 ) ;
#42365 = DIRECTION ( 'NONE',  ( -0.5449076811759708816, 0.6444004775717707689, 0.5364919789714475140 ) ) ;
#42366 = VECTOR ( 'NONE', #50916, 999.9999999999998863 ) ;
#42367 = ORIENTED_EDGE ( 'NONE', *, *, #51587, .F. ) ;
#42368 = VERTEX_POINT ( 'NONE', #30620 ) ;
#42369 = ORIENTED_EDGE ( 'NONE', *, *, #26528, .T. ) ;
#42370 = CARTESIAN_POINT ( 'NONE',  ( -15.05218540864184540, 4.981562823951512620, 2.369773783146779778 ) ) ;
#42371 = DIRECTION ( 'NONE',  ( 0.005002170337468016433, -0.7660444431189770143, -0.6427681459581293666 ) ) ;
#42372 = DIRECTION ( 'NONE',  ( 0.9999697198139515519, 0.000000000000000000, 0.007781995580013368816 ) ) ;
#42373 = LINE ( 'NONE', #46916, #36663 ) ;
#42374 = ADVANCED_FACE ( 'NONE', ( #48772 ), #184, .F. ) ;
#42375 = VERTEX_POINT ( 'NONE', #52715 ) ;
#42376 = ORIENTED_EDGE ( 'NONE', *, *, #32616, .T. ) ;
#42377 = VERTEX_POINT ( 'NONE', #32495 ) ;
#42378 = DIRECTION ( 'NONE',  ( -0.9999697198139514409, 0.000000000000000000, -0.007781995580013368816 ) ) ;
#42379 = PLANE ( 'NONE',  #431 ) ;
#42380 = VERTEX_POINT ( 'NONE', #49797 ) ;
#42381 = DIRECTION ( 'NONE',  ( 0.000000000000000000, -0.000000000000000000, -1.000000000000000000 ) ) ;
#42382 = VERTEX_POINT ( 'NONE', #26076 ) ;
#42383 = CARTESIAN_POINT ( 'NONE',  ( -13.63673279712320507, -0.1191753592594197858, 12.22739664767016521 ) ) ;
#42384 = CARTESIAN_POINT ( 'NONE',  ( -29.86197018149027116, 0.000000000000000000, 8.281335066757780083 ) ) ;
#42385 = ADVANCED_FACE ( 'NONE', ( #13823 ), #47107, .T. ) ;
#42386 = EDGE_LOOP ( 'NONE', ( #43265, #20524, #31127, #31249 ) ) ;
#42387 = CARTESIAN_POINT ( 'NONE',  ( 2.072287782118878319, 0.000000000000000000, -2.950529333540147015 ) ) ;
#42388 = ORIENTED_EDGE ( 'NONE', *, *, #15269, .T. ) ;
#42389 = EDGE_CURVE ( 'NONE', #621, #2726, #35700, .T. ) ;
#42390 = EDGE_CURVE ( 'NONE', #29543, #24756, #50896, .T. ) ;
#42391 = VECTOR ( 'NONE', #15722, 1000.000000000000114 ) ;
#42392 = DIRECTION ( 'NONE',  ( 0.007781995580012662783, 0.000000000000000000, -0.9999697198139514409 ) ) ;
#42393 = CARTESIAN_POINT ( 'NONE',  ( -14.89517369626102195, 0.000000000000000000, 7.659145998126207999 ) ) ;
#42394 = VERTEX_POINT ( 'NONE', #54585 ) ;
#42395 = DIRECTION ( 'NONE',  ( 0.000000000000000000, 5.782411586589354681E-16, -1.000000000000000000 ) ) ;
#42396 = CARTESIAN_POINT ( 'NONE',  ( -20.50465292808819839, -5.051250379848164052, 4.684863322079202419 ) ) ;
#42397 = DIRECTION ( 'NONE',  ( 0.6427681459581294776, -0.7660444431189769032, 0.005002170337467562802 ) ) ;
#42398 = CARTESIAN_POINT ( 'NONE',  ( -12.33850799832341849, 0.000000000000000000, 11.68350162852954632 ) ) ;
#42399 = ORIENTED_EDGE ( 'NONE', *, *, #39993, .T. ) ;
#42400 = ORIENTED_EDGE ( 'NONE', *, *, #51642, .T. ) ;
#42401 = AXIS2_PLACEMENT_3D ( 'NONE', #45260, #16006, #27958 ) ;
#42402 = EDGE_CURVE ( 'NONE', #39510, #42731, #16542, .T. ) ;
#42403 = CARTESIAN_POINT ( 'NONE',  ( -16.89925026227929195, -0.1191753592594197858, 13.49466922669627422 ) ) ;
#42404 = DIRECTION ( 'NONE',  ( -0.9999697198139514409, -0.000000000000000000, -0.007781995580013368816 ) ) ;
#42405 = LINE ( 'NONE', #20806, #3268 ) ;
#42406 = LINE ( 'NONE', #2636, #18562 ) ;
#42407 = EDGE_CURVE ( 'NONE', #17347, #13812, #29333, .T. ) ;
#42408 = DIRECTION ( 'NONE',  ( 0.6427681459581294776, -0.7660444431189769032, 0.005002170337467562802 ) ) ;
#42409 = DIRECTION ( 'NONE',  ( -0.005002170337468016433, -0.7660444431189770143, 0.6427681459581293666 ) ) ;
#42410 = ORIENTED_EDGE ( 'NONE', *, *, #25149, .T. ) ;
#42411 = CARTESIAN_POINT ( 'NONE',  ( -9.001607178914184715, -0.02746274897879631693, 3.819319703528829546 ) ) ;
#42412 = PLANE ( 'NONE',  #6925 ) ;
#42413 = EDGE_LOOP ( 'NONE', ( #51995, #21931, #18851, #4514 ) ) ;
#42414 = PLANE ( 'NONE',  #514 ) ;
#42415 = EDGE_LOOP ( 'NONE', ( #19958, #46319, #42008, #44389 ) ) ;
#42416 = EDGE_CURVE ( 'NONE', #3628, #37763, #28487, .T. ) ;
#42417 = DIRECTION ( 'NONE',  ( 0.005002170337468016433, -0.7660444431189770143, -0.6427681459581293666 ) ) ;
#42418 = LINE ( 'NONE', #23961, #19690 ) ;
#42419 = LINE ( 'NONE', #37585, #48601 ) ;
#42420 = DIRECTION ( 'NONE',  ( 0.000000000000000000, -0.000000000000000000, -1.000000000000000000 ) ) ;
#42421 = CARTESIAN_POINT ( 'NONE',  ( -66.43251979230488757, 1.999999999999989120, -5.460169066007572347 ) ) ;
#42422 = EDGE_CURVE ( 'NONE', #873, #18658, #41557, .T. ) ;
#42423 = ORIENTED_EDGE ( 'NONE', *, *, #13934, .F. ) ;
#42424 = EDGE_LOOP ( 'NONE', ( #23050, #23526, #26498, #24208 ) ) ;
#42425 = CARTESIAN_POINT ( 'NONE',  ( -11.23574289049249231, -0.1191753592594189115, 2.247646515827207647 ) ) ;
#42426 = LINE ( 'NONE', #20568, #29490 ) ;
#42427 = CARTESIAN_POINT ( 'NONE',  ( 1.971453974394196562, 0.000000000000000000, 10.00639841352631088 ) ) ;
#42428 = DIRECTION ( 'NONE',  ( 0.6427681459581294776, -0.7660444431189769032, 0.005002170337467562802 ) ) ;
#42429 = DIRECTION ( 'NONE',  ( 0.9999697198139515519, 0.000000000000000000, 0.007781995580013368816 ) ) ;
#42430 = CARTESIAN_POINT ( 'NONE',  ( -19.61647402266476803, -0.1191753592594171213, 4.401331113001130113 ) ) ;
#42431 = ORIENTED_EDGE ( 'NONE', *, *, #41909, .T. ) ;
#42432 = LINE ( 'NONE', #38152, #22897 ) ;
#42433 = LINE ( 'NONE', #46974, #55923 ) ;
#42434 = DIRECTION ( 'NONE',  ( -0.005961354470445682716, -0.6427876096865404731, 0.7660212471507180654 ) ) ;
#42435 = ORIENTED_EDGE ( 'NONE', *, *, #40399, .T. ) ;
#42436 = CARTESIAN_POINT ( 'NONE',  ( 2.072287782118878319, 0.000000000000000000, -2.950529333540147015 ) ) ;
#42437 = DIRECTION ( 'NONE',  ( 0.000000000000000000, -1.000000000000000000, 0.000000000000000000 ) ) ;
#42438 = CARTESIAN_POINT ( 'NONE',  ( -8.875996589204540044, 0.000000000000000000, 10.41778544861944233 ) ) ;
#42439 = ORIENTED_EDGE ( 'NONE', *, *, #1583, .F. ) ;
#42440 = VECTOR ( 'NONE', #27892, 999.9999999999998863 ) ;
#42441 = CARTESIAN_POINT ( 'NONE',  ( 2.072287782118878319, 0.000000000000000000, -2.950529333540147015 ) ) ;
#42442 = EDGE_CURVE ( 'NONE', #13455, #18918, #7764, .T. ) ;
#42443 = ORIENTED_EDGE ( 'NONE', *, *, #20107, .T. ) ;
#42444 = ORIENTED_EDGE ( 'NONE', *, *, #43595, .F. ) ;
#42445 = EDGE_CURVE ( 'NONE', #19751, #46912, #41279, .T. ) ;
#42446 = EDGE_LOOP ( 'NONE', ( #43136, #7353, #47113, #29087 ) ) ;
#42447 = VERTEX_POINT ( 'NONE', #55439 ) ;
#42448 = LINE ( 'NONE', #24839, #9374 ) ;
#42450 = EDGE_CURVE ( 'NONE', #3308, #56226, #42103, .T. ) ;
#42449 = ORIENTED_EDGE ( 'NONE', *, *, #32861, .F. ) ;
#42451 = LINE ( 'NONE', #55486, #30401 ) ;
#42452 = EDGE_CURVE ( 'NONE', #16370, #22478, #42406, .T. ) ;
#42453 = EDGE_CURVE ( 'NONE', #49004, #51932, #3497, .T. ) ;
#42454 = ORIENTED_EDGE ( 'NONE', *, *, #44960, .F. ) ;
#42455 = DIRECTION ( 'NONE',  ( -0.000000000000000000, -0.000000000000000000, -1.000000000000000000 ) ) ;
#42456 = ORIENTED_EDGE ( 'NONE', *, *, #9761, .F. ) ;
#42457 = ORIENTED_EDGE ( 'NONE', *, *, #106, .F. ) ;
#42458 = ADVANCED_FACE ( 'NONE', ( #20807 ), #15696, .F. ) ;
#42459 = CARTESIAN_POINT ( 'NONE',  ( -19.60990026154428278, 0.000000000000000000, 4.498472333781370125 ) ) ;
#42460 = DIRECTION ( 'NONE',  ( -0.5449076811759708816, 0.6444004775717707689, 0.5364919789714475140 ) ) ;
#42461 = DIRECTION ( 'NONE',  ( 0.6427681459581294776, -0.7660444431189769032, 0.005002170337467562802 ) ) ;
#42462 = LINE ( 'NONE', #3277, #44104 ) ;
#42463 = SURFACE_STYLE_USAGE ( .BOTH. , #46714 ) ;
#42464 = ORIENTED_EDGE ( 'NONE', *, *, #2381, .T. ) ;
#42465 = EDGE_LOOP ( 'NONE', ( #8581, #42761, #22926, #54030 ) ) ;
#42466 = EDGE_CURVE ( 'NONE', #37629, #39029, #38125, .T. ) ;
#42467 = CYLINDRICAL_SURFACE ( 'NONE', #5856, 2.125000000000000000 ) ;
#42468 = LINE ( 'NONE', #15486, #37546 ) ;
#42469 = EDGE_CURVE ( 'NONE', #35036, #4830, #54329, .T. ) ;
#42470 = DIRECTION ( 'NONE',  ( 0.000000000000000000, -0.000000000000000000, -1.000000000000000000 ) ) ;
#42471 = CARTESIAN_POINT ( 'NONE',  ( -11.32823801451301726, -1.327505506330656893, 3.260866780426896483 ) ) ;
#42472 = EDGE_CURVE ( 'NONE', #56189, #27265, #15422, .T. ) ;
#42473 = DIRECTION ( 'NONE',  ( -0.3620778797217456546, 0.000000000000000000, -0.9321478471874540261 ) ) ;
#42474 = CARTESIAN_POINT ( 'NONE',  ( -16.28710523641237273, -4.403642575758160760, 10.23552420831110865 ) ) ;
#42475 = ORIENTED_EDGE ( 'NONE', *, *, #54140, .F. ) ;
#42476 = CARTESIAN_POINT ( 'NONE',  ( -19.94369481285463408, 1.574118978153236093, 6.298974588870400737 ) ) ;
#42477 = CARTESIAN_POINT ( 'NONE',  ( -15.86710544311044302, 0.000000000000000000, 13.13336954653252953 ) ) ;
#42478 = ORIENTED_EDGE ( 'NONE', *, *, #34149, .T. ) ;
#42479 = EDGE_CURVE ( 'NONE', #10688, #17567, #28205, .T. ) ;
#42480 = VECTOR ( 'NONE', #13897, 1000.000000000000114 ) ;
#42481 = FACE_OUTER_BOUND ( 'NONE', #30058, .T. ) ;
#42482 = DIRECTION ( 'NONE',  ( -0.6427681459581293666, -0.7660444431189770143, -0.005002170337467561935 ) ) ;
#42483 = PLANE ( 'NONE',  #25432 ) ;
#42484 = CARTESIAN_POINT ( 'NONE',  ( 2.072287782118878319, 0.000000000000000000, -2.950529333540147015 ) ) ;
#42485 = CARTESIAN_POINT ( 'NONE',  ( -11.30636317915456779, -0.1191753592594197858, 11.32220194836580340 ) ) ;
#42486 = ORIENTED_EDGE ( 'NONE', *, *, #50106, .T. ) ;
#42487 = ORIENTED_EDGE ( 'NONE', *, *, #20903, .T. ) ;
#42488 = LINE ( 'NONE', #8130, #50212 ) ;
#42489 = DIRECTION ( 'NONE',  ( 0.9999697198139515519, 0.000000000000000000, 0.007781995580013368816 ) ) ;
#42490 = DIRECTION ( 'NONE',  ( -0.5449076811759708816, 0.6444004775717707689, 0.5364919789714475140 ) ) ;
#42491 = CARTESIAN_POINT ( 'NONE',  ( -15.88130887279446490, 0.000000000000000000, 3.050160814894388839 ) ) ;
#42492 = DIRECTION ( 'NONE',  ( -0.6246952433987893460, -0.7422098413412802076, 0.2426528472758542054 ) ) ;
#42493 = PLANE ( 'NONE',  #50002 ) ;
#42494 = LINE ( 'NONE', #11816, #51055 ) ;
#42495 = LINE ( 'NONE', #10792, #27801 ) ;
#42496 = CARTESIAN_POINT ( 'NONE',  ( -70.26988861484534254, -8.746188756442855095, 8.208045577613539479 ) ) ;
#42497 = LINE ( 'NONE', #3013, #15625 ) ;
#42498 = VERTEX_POINT ( 'NONE', #45515 ) ;
#42499 = FACE_OUTER_BOUND ( 'NONE', #52230, .T. ) ;
#42500 = EDGE_CURVE ( 'NONE', #6162, #56100, #7463, .T. ) ;
#42501 = ORIENTED_EDGE ( 'NONE', *, *, #33434, .F. ) ;
#42502 = EDGE_CURVE ( 'NONE', #34236, #25655, #19961, .T. ) ;
#42503 = ORIENTED_EDGE ( 'NONE', *, *, #46840, .T. ) ;
#42504 = VERTEX_POINT ( 'NONE', #41814 ) ;
#42505 = ORIENTED_EDGE ( 'NONE', *, *, #47303, .F. ) ;
#42506 = ORIENTED_EDGE ( 'NONE', *, *, #29966, .T. ) ;
#42507 = ORIENTED_EDGE ( 'NONE', *, *, #54541, .F. ) ;
#42508 = CARTESIAN_POINT ( 'NONE',  ( -19.02759475333626327, -4.403642575758163424, 4.131785845448357364 ) ) ;
#42509 = DIRECTION ( 'NONE',  ( 0.007781995580012663651, -3.146120232559066537E-19, -0.9999697198139514409 ) ) ;
#42510 = DIRECTION ( 'NONE',  ( -0.6427681459581293666, -0.7660444431189770143, -0.005002170337467561935 ) ) ;
#42511 = EDGE_CURVE ( 'NONE', #46187, #28751, #37871, .T. ) ;
#42512 = EDGE_CURVE ( 'NONE', #38880, #5158, #54893, .T. ) ;
#42513 = ADVANCED_FACE ( 'NONE', ( #8602 ), #46946, .F. ) ;
#42514 = AXIS2_PLACEMENT_3D ( 'NONE', #11476, #10662, #24507 ) ;
#42515 = ORIENTED_EDGE ( 'NONE', *, *, #45403, .T. ) ;
#42516 = DIRECTION ( 'NONE',  ( 0.8531650599175527594, 0.4028455766673922356, -0.3313982828793700652 ) ) ;
#42517 = ORIENTED_EDGE ( 'NONE', *, *, #50726, .T. ) ;
#42518 = CARTESIAN_POINT ( 'NONE',  ( -65.31815034969253020, -11.19801294790904578, -4.498572511313247979 ) ) ;
#42519 = ADVANCED_FACE ( 'NONE', ( #30475 ), #43260, .F. ) ;
#42520 = ORIENTED_EDGE ( 'NONE', *, *, #13029, .F. ) ;
#42521 = CARTESIAN_POINT ( 'NONE',  ( -67.14859018435215887, -9.394809955489860087, 5.522897687430004865 ) ) ;
#42522 = DIRECTION ( 'NONE',  ( -0.005961354470445682716, -0.6427876096865404731, 0.7660212471507180654 ) ) ;
#42523 = CARTESIAN_POINT ( 'NONE',  ( -28.93137873341882127, 0.000000000000000000, 8.119251130998824451 ) ) ;
#42524 = ORIENTED_EDGE ( 'NONE', *, *, #22730, .T. ) ;
#42525 = DIRECTION ( 'NONE',  ( -0.6427681459581293666, -0.7660444431189770143, -0.005002170337467561935 ) ) ;
#42526 = ORIENTED_EDGE ( 'NONE', *, *, #32921, .F. ) ;
#42527 = DIRECTION ( 'NONE',  ( -0.005961354470445682716, -0.6427876096865404731, 0.7660212471507180654 ) ) ;
#42528 = CARTESIAN_POINT ( 'NONE',  ( -20.54204810873173415, 0.000000000000000000, 4.860550213503115558 ) ) ;
#42529 = EDGE_CURVE ( 'NONE', #3673, #36934, #25934, .T. ) ;
#42530 = LINE ( 'NONE', #12451, #29659 ) ;
#42531 = CARTESIAN_POINT ( 'NONE',  ( -13.08486533123210194, 0.000000000000000000, 1.963927175729152541 ) ) ;
#42532 = CARTESIAN_POINT ( 'NONE',  ( -16.89925026227929195, -0.1191753592594197858, 13.49466922669627422 ) ) ;
#42533 = CARTESIAN_POINT ( 'NONE',  ( -69.06076127825900812, -0.2533158072296424201, -7.481591365497656021 ) ) ;
#42534 = ADVANCED_FACE ( 'NONE', ( #9144 ), #30173, .F. ) ;
#42535 = CARTESIAN_POINT ( 'NONE',  ( -18.66354898467281132, 0.000000000000000000, 14.21960318569776582 ) ) ;
#42536 = CARTESIAN_POINT ( 'NONE',  ( -67.41690247247410639, -11.43868567671724890, 4.989023737097910249 ) ) ;
#42537 = EDGE_LOOP ( 'NONE', ( #37620, #19231, #37030, #19616 ) ) ;
#42538 = CARTESIAN_POINT ( 'NONE',  ( -56.73021393513262467, 6.246123507023290777, -2.439641667270313619 ) ) ;
#42539 = ORIENTED_EDGE ( 'NONE', *, *, #53904, .F. ) ;
#42540 = ADVANCED_FACE ( 'NONE', ( #21383 ), #52328, .F. ) ;
#42541 = CARTESIAN_POINT ( 'NONE',  ( -23.33849165029409889, 0.000000000000000000, 5.946783852668351855 ) ) ;
#42542 = CARTESIAN_POINT ( 'NONE',  ( -14.99479423072147455, 5.467268677019013978, 2.331984540967731334 ) ) ;
#42543 = CARTESIAN_POINT ( 'NONE',  ( -14.00280974873554030, 0.000000000000000000, 12.40921378708904044 ) ) ;
#42544 = LINE ( 'NONE', #11861, #42181 ) ;
#42545 = CARTESIAN_POINT ( 'NONE',  ( -12.83240616472669338, -4.241740624735664156, 1.730529728029736036 ) ) ;
#42546 = EDGE_CURVE ( 'NONE', #43321, #26517, #38716, .T. ) ;
#42547 = CARTESIAN_POINT ( 'NONE',  ( -11.21979143729918960, -0.1191753592594197858, 1.139774444304266554 ) ) ;
#42548 = ORIENTED_EDGE ( 'NONE', *, *, #50856, .F. ) ;
#42549 = CARTESIAN_POINT ( 'NONE',  ( -17.85712253972278418, 0.000000000000000000, 4.312106799082268793 ) ) ;
#42550 = CARTESIAN_POINT ( 'NONE',  ( -19.67731969574463236, 19.56551921504356883, 4.315409177132068841 ) ) ;
#42551 = LINE ( 'NONE', #7933, #7672 ) ;
#42552 = DIRECTION ( 'NONE',  ( 0.5449076811759707706, 0.6444004775717708799, -0.5364919789714476250 ) ) ;
#42553 = DIRECTION ( 'NONE',  ( 0.000000000000000000, -0.000000000000000000, -1.000000000000000000 ) ) ;
#42554 = CARTESIAN_POINT ( 'NONE',  ( -16.06709938707323460, 0.000000000000000000, 13.13181314741652628 ) ) ;
#42555 = DIRECTION ( 'NONE',  ( -0.9999697198139514409, -0.000000000000000000, -0.007781995580013368816 ) ) ;
#42556 = LINE ( 'NONE', #46235, #55555 ) ;
#42557 = ORIENTED_EDGE ( 'NONE', *, *, #35791, .F. ) ;
#42558 = DIRECTION ( 'NONE',  ( 0.000000000000000000, -1.000000000000000000, 0.000000000000000000 ) ) ;
#42559 = DIRECTION ( 'NONE',  ( -0.5364919789714478471, 0.6444004775717705469, -0.5449076811759709926 ) ) ;
#42560 = ORIENTED_EDGE ( 'NONE', *, *, #22172, .T. ) ;
#42561 = ORIENTED_EDGE ( 'NONE', *, *, #40713, .F. ) ;
#42562 = LINE ( 'NONE', #24662, #7440 ) ;
#42563 = ORIENTED_EDGE ( 'NONE', *, *, #34302, .T. ) ;
#42564 = LINE ( 'NONE', #50795, #17498 ) ;
#42565 = VERTEX_POINT ( 'NONE', #42660 ) ;
#42566 = ORIENTED_EDGE ( 'NONE', *, *, #27915, .T. ) ;
#42567 = VERTEX_POINT ( 'NONE', #29901 ) ;
#42568 = DIRECTION ( 'NONE',  ( -0.005961354470445682716, -0.6427876096865404731, 0.7660212471507180654 ) ) ;
#42569 = CARTESIAN_POINT ( 'NONE',  ( -65.44866277073604977, -9.199872132678805770, 3.266248677641420350 ) ) ;
#42570 = DIRECTION ( 'NONE',  ( 0.5364919789714477361, 0.6444004775717706579, 0.5449076811759711036 ) ) ;
#42571 = EDGE_CURVE ( 'NONE', #33755, #11370, #55731, .T. ) ;
#42572 = ORIENTED_EDGE ( 'NONE', *, *, #7329, .F. ) ;
#42573 = ORIENTED_EDGE ( 'NONE', *, *, #12836, .T. ) ;
#42574 = ADVANCED_FACE ( 'NONE', ( #34177 ), #52025, .F. ) ;
#42575 = EDGE_CURVE ( 'NONE', #44124, #38604, #16846, .T. ) ;
#42576 = DIRECTION ( 'NONE',  ( 0.000000000000000000, -0.000000000000000000, -1.000000000000000000 ) ) ;
#42577 = DIRECTION ( 'NONE',  ( 0.000000000000000000, -0.000000000000000000, -1.000000000000000000 ) ) ;
#42578 = ORIENTED_EDGE ( 'NONE', *, *, #52422, .T. ) ;
#42579 = PLANE ( 'NONE',  #40944 ) ;
#42580 = CARTESIAN_POINT ( 'NONE',  ( -8.975993561185934055, -0.1191753592594197858, 10.41700724906143982 ) ) ;
#42581 = EDGE_LOOP ( 'NONE', ( #56024, #44381, #7129, #47769 ) ) ;
#42582 = DIRECTION ( 'NONE',  ( 0.000000000000000000, -1.000000000000000000, 0.000000000000000000 ) ) ;
#42583 = CARTESIAN_POINT ( 'NONE',  ( -12.73174640694442772, 0.000000000000000000, 2.505333312241550647 ) ) ;
#42584 = AXIS2_PLACEMENT_3D ( 'NONE', #32375, #50516, #11611 ) ;
#42585 = ORIENTED_EDGE ( 'NONE', *, *, #19840, .F. ) ;
#42586 = CARTESIAN_POINT ( 'NONE',  ( -15.96710241509184058, -0.1191753592594218814, 13.13259134697452879 ) ) ;
#42587 = LINE ( 'NONE', #34928, #70 ) ;
#42588 = ORIENTED_EDGE ( 'NONE', *, *, #14681, .F. ) ;
#42589 = CARTESIAN_POINT ( 'NONE',  ( -21.47419595591918906, 0.000000000000000000, 5.222628093224860102 ) ) ;
#42590 = DIRECTION ( 'NONE',  ( -0.5364919789714478471, 0.6444004775717705469, -0.5449076811759709926 ) ) ;
#42591 = LINE ( 'NONE', #26130, #54740 ) ;
#42592 = CARTESIAN_POINT ( 'NONE',  ( -26.13493519185646008, 0.000000000000000000, 7.033017491833586377 ) ) ;
#42593 = ORIENTED_EDGE ( 'NONE', *, *, #44122, .T. ) ;
#42594 = CARTESIAN_POINT ( 'NONE',  ( -69.76593803006062444, -0.7338954340007644017, -7.496705766434927476 ) ) ;
#42595 = CARTESIAN_POINT ( 'NONE',  ( -20.06177075545399191, 0.000000000000000000, 14.76272000528038220 ) ) ;
#42596 = DIRECTION ( 'NONE',  ( 0.005961354470445682716, -0.6427876096865404731, -0.7660212471507180654 ) ) ;
#42597 = PLANE ( 'NONE',  #41342 ) ;
#42598 = EDGE_CURVE ( 'NONE', #36178, #29020, #17119, .T. ) ;
#42599 = CARTESIAN_POINT ( 'NONE',  ( -17.26532721389163072, 0.000000000000000000, 13.67648636611514590 ) ) ;
#42600 = DIRECTION ( 'NONE',  ( 0.000000000000000000, -0.000000000000000000, -1.000000000000000000 ) ) ;
#42601 = CARTESIAN_POINT ( 'NONE',  ( -21.60897430903675698, -3.594132820645662196, 5.160308928338091405 ) ) ;
#42602 = ORIENTED_EDGE ( 'NONE', *, *, #55119, .T. ) ;
#42603 = EDGE_CURVE ( 'NONE', #3706, #46700, #4357, .T. ) ;
#42604 = CARTESIAN_POINT ( 'NONE',  ( -68.19194133488814202, 5.005647646799308669E-13, 6.473804834635568994 ) ) ;
#42605 = EDGE_LOOP ( 'NONE', ( #41350, #50997, #34595, #25943 ) ) ;
#42606 = DIRECTION ( 'NONE',  ( -0.6427681459581293666, -0.7660444431189770143, -0.005002170337467561935 ) ) ;
#42607 = DIRECTION ( 'NONE',  ( -0.4165485852472824990, -0.02380568209675230223, 0.9088017196442774726 ) ) ;
#42608 = EDGE_CURVE ( 'NONE', #329, #3917, #38976, .T. ) ;
#42609 = CARTESIAN_POINT ( 'NONE',  ( -27.99767448711536133, 0.000000000000000000, 7.557179307314289218 ) ) ;
#42610 = PLANE ( 'NONE',  #31485 ) ;
#42611 = DIRECTION ( 'NONE',  ( -0.5449076811759708816, 0.6444004775717707689, 0.5364919789714475140 ) ) ;
#42612 = EDGE_LOOP ( 'NONE', ( #39570, #14938, #54556, #874 ) ) ;
#42613 = VECTOR ( 'NONE', #44487, 1000.000000000000227 ) ;
#42614 = EDGE_LOOP ( 'NONE', ( #26244, #36345, #10217, #25613, #27618 ) ) ;
#42615 = CARTESIAN_POINT ( 'NONE',  ( -14.01623497886155256, -0.1191753592594197858, 2.226008083469502630 ) ) ;
#42616 = DIRECTION ( 'NONE',  ( 0.5449076811759707706, 0.6444004775717708799, -0.5364919789714476250 ) ) ;
#42617 = ORIENTED_EDGE ( 'NONE', *, *, #50262, .T. ) ;
#42618 = CARTESIAN_POINT ( 'NONE',  ( -23.33849165029409889, 0.000000000000000000, 5.946783852668351855 ) ) ;
#42619 = ORIENTED_EDGE ( 'NONE', *, *, #7955, .T. ) ;
#42620 = DIRECTION ( 'NONE',  ( 0.005002170337468016433, -0.7660444431189770143, -0.6427681459581293666 ) ) ;
#42621 = ORIENTED_EDGE ( 'NONE', *, *, #14260, .T. ) ;
#42622 = LINE ( 'NONE', #42058, #11170 ) ;
#42623 = ORIENTED_EDGE ( 'NONE', *, *, #25404, .T. ) ;
#42624 = VERTEX_POINT ( 'NONE', #30747 ) ;
#42625 = ORIENTED_EDGE ( 'NONE', *, *, #4792, .F. ) ;
#42626 = CARTESIAN_POINT ( 'NONE',  ( 0.000000000000000000, -1.000000000000000000, 2.125000000000000000 ) ) ;
#42627 = ADVANCED_FACE ( 'NONE', ( #643 ), #17378, .F. ) ;
#42628 = CARTESIAN_POINT ( 'NONE',  ( 2.072287782118878319, 0.000000000000000000, -2.950529333540147015 ) ) ;
#42629 = CARTESIAN_POINT ( 'NONE',  ( -23.33849165029409889, 0.000000000000000000, 5.946783852668351855 ) ) ;
#42630 = ADVANCED_FACE ( 'NONE', ( #43777 ), #21919, .F. ) ;
#42631 = PLANE ( 'NONE',  #7638 ) ;
#42632 = VERTEX_POINT ( 'NONE', #17677 ) ;
#42633 = EDGE_CURVE ( 'NONE', #40102, #10235, #337, .T. ) ;
#42634 = ORIENTED_EDGE ( 'NONE', *, *, #1060, .F. ) ;
#42635 = ORIENTED_EDGE ( 'NONE', *, *, #55593, .F. ) ;
#42636 = CARTESIAN_POINT ( 'NONE',  ( -19.39010111284826365, -0.1191753592594167188, 7.724168461730136492 ) ) ;
#42637 = LINE ( 'NONE', #7736, #52118 ) ;
#42638 = ORIENTED_EDGE ( 'NONE', *, *, #9306, .F. ) ;
#42639 = DIRECTION ( 'NONE',  ( -0.6427681459581293666, -0.7660444431189770143, -0.005002170337467561935 ) ) ;
#42640 = ORIENTED_EDGE ( 'NONE', *, *, #21168, .T. ) ;
#42641 = PLANE ( 'NONE',  #39642 ) ;
#42642 = LINE ( 'NONE', #8584, #5872 ) ;
#42643 = ORIENTED_EDGE ( 'NONE', *, *, #55028, .F. ) ;
#42644 = FACE_OUTER_BOUND ( 'NONE', #17220, .T. ) ;
#42645 = ORIENTED_EDGE ( 'NONE', *, *, #23052, .F. ) ;
#42646 = ADVANCED_FACE ( 'NONE', ( #29642 ), #35547, .F. ) ;
#42647 = VECTOR ( 'NONE', #20481, 1000.000000000000000 ) ;
#42648 = CARTESIAN_POINT ( 'NONE',  ( -17.74560456716937296, 0.000000000000000000, 3.774316574337878372 ) ) ;
#42649 = FACE_OUTER_BOUND ( 'NONE', #20769, .T. ) ;
#42650 = EDGE_LOOP ( 'NONE', ( #7740, #54794, #7621, #20852 ) ) ;
#42651 = DIRECTION ( 'NONE',  ( -0.7660212471507179544, -0.6427876096865405842, -0.005961354470445141482 ) ) ;
#42652 = CARTESIAN_POINT ( 'NONE',  ( -28.93137873341882127, 0.000000000000000000, 8.119251130998824451 ) ) ;
#42653 = CARTESIAN_POINT ( 'NONE',  ( -10.47421230394850866, 0.000000000000000000, 10.95934586908605723 ) ) ;
#42654 = FACE_OUTER_BOUND ( 'NONE', #31054, .T. ) ;
#42655 = ORIENTED_EDGE ( 'NONE', *, *, #1045, .F. ) ;
#42656 = VERTEX_POINT ( 'NONE', #36133 ) ;
#42657 = DIRECTION ( 'NONE',  ( -0.9999697198139514409, -0.000000000000000000, -0.007781995580013368816 ) ) ;
#42658 = CARTESIAN_POINT ( 'NONE',  ( -67.79361442428482576, 2.000000000000000000, 7.454431982338135754 ) ) ;
#42659 = CARTESIAN_POINT ( 'NONE',  ( -16.33317936670417225, 0.000000000000000000, 13.31440848639340224 ) ) ;
#42660 = CARTESIAN_POINT ( 'NONE',  ( -13.02956034749683667, 0.000000000000000000, 6.765674479387740803 ) ) ;
#42661 = CARTESIAN_POINT ( 'NONE',  ( -13.53673582514181106, 0.000000000000000000, 12.22817484722816772 ) ) ;
#42662 = LINE ( 'NONE', #38127, #5921 ) ;
#42663 = VERTEX_POINT ( 'NONE', #53434 ) ;
#42664 = CARTESIAN_POINT ( 'NONE',  ( 0.1285714285714296967, 2.000000000000000000, -5.998622290806041590 ) ) ;
#42665 = DIRECTION ( 'NONE',  ( -0.005002170337468016433, -0.7660444431189770143, 0.6427681459581293666 ) ) ;
#42666 = CARTESIAN_POINT ( 'NONE',  ( -9.908141408373387193, -0.1191753592594197858, 10.77908512878318703 ) ) ;
#42667 = VERTEX_POINT ( 'NONE', #40666 ) ;
#42668 = DIRECTION ( 'NONE',  ( 0.7660212471507180654, -0.6427876096865404731, 0.005961354470445141482 ) ) ;
#42669 = VERTEX_POINT ( 'NONE', #36383 ) ;
#42670 = CARTESIAN_POINT ( 'NONE',  ( -12.60458797795435615, 0.000000000000000000, 11.86609696750642229 ) ) ;
#42671 = CARTESIAN_POINT ( 'NONE',  ( -15.86710544311044302, 0.000000000000000000, 13.13336954653252953 ) ) ;
#42672 = ADVANCED_FACE ( 'NONE', ( #52858 ), #23602, .F. ) ;
#42673 = DIRECTION ( 'NONE',  ( 0.007781995580012663651, 0.000000000000000000, -0.9999697198139515519 ) ) ;
#42674 = CARTESIAN_POINT ( 'NONE',  ( -66.45493427417522980, 1.999999999999980460, 5.466724623769072977 ) ) ;
#42675 = ORIENTED_EDGE ( 'NONE', *, *, #4907, .T. ) ;
#42676 = ORIENTED_EDGE ( 'NONE', *, *, #13986, .T. ) ;
#42677 = PLANE ( 'NONE',  #27617 ) ;
#42678 = CARTESIAN_POINT ( 'NONE',  ( -26.13493519185646008, 0.000000000000000000, 7.033017491833586377 ) ) ;
#42679 = LINE ( 'NONE', #17986, #1615 ) ;
#42680 = ADVANCED_FACE ( 'NONE', ( #49158 ), #1737, .F. ) ;
#42681 = DIRECTION ( 'NONE',  ( 1.007958083594381472E-15, -3.869188571150965639E-16, 1.000000000000000000 ) ) ;
#42682 = CARTESIAN_POINT ( 'NONE',  ( -9.873446788527346030, -0.1191753592594185784, 6.320900986966644375 ) ) ;
#42683 = CIRCLE ( 'NONE', #40870, 0.5000000000000004441 ) ;
#42684 = CARTESIAN_POINT ( 'NONE',  ( -8.470622023031074477, -0.1191753592594188838, 5.186309231652734830 ) ) ;
#42686 = EDGE_CURVE ( 'NONE', #55206, #49405, #53695, .T. ) ;
#42685 = ORIENTED_EDGE ( 'NONE', *, *, #37235, .T. ) ;
#42687 = LINE ( 'NONE', #55764, #55551 ) ;
#42688 = EDGE_CURVE ( 'NONE', #48572, #308, #31295, .T. ) ;
#42689 = VECTOR ( 'NONE', #26095, 1000.000000000000227 ) ;
#42690 = CARTESIAN_POINT ( 'NONE',  ( -26.13337879274045505, 0.000000000000000000, 6.833023547870798353 ) ) ;
#42691 = DIRECTION ( 'NONE',  ( -0.9999697198139514409, -0.000000000000000000, -0.007781995580013368816 ) ) ;
#42692 = ORIENTED_EDGE ( 'NONE', *, *, #31628, .F. ) ;
#42693 = FACE_OUTER_BOUND ( 'NONE', #45424, .T. ) ;
#42694 = EDGE_CURVE ( 'NONE', #37130, #44870, #40918, .T. ) ;
#42695 = CARTESIAN_POINT ( 'NONE',  ( -32.65997012216863737, 0.000000000000000000, 9.567562649885804404 ) ) ;
#42696 = PLANE ( 'NONE',  #13011 ) ;
#42697 = ORIENTED_EDGE ( 'NONE', *, *, #40954, .F. ) ;
#42698 = PLANE ( 'NONE',  #32124 ) ;
#42699 = ADVANCED_FACE ( 'NONE', ( #32139 ), #30994, .F. ) ;
#42700 = ORIENTED_EDGE ( 'NONE', *, *, #8487, .F. ) ;
#42701 = EDGE_CURVE ( 'NONE', #7637, #38457, #10272, .T. ) ;
#42702 = ORIENTED_EDGE ( 'NONE', *, *, #26869, .T. ) ;
#42703 = EDGE_LOOP ( 'NONE', ( #35589, #55854, #52878, #2454 ) ) ;
#42704 = ORIENTED_EDGE ( 'NONE', *, *, #30602, .F. ) ;
#42705 = CARTESIAN_POINT ( 'NONE',  ( -26.13493519185646008, 0.000000000000000000, 7.033017491833586377 ) ) ;
#42706 = ORIENTED_EDGE ( 'NONE', *, *, #29211, .T. ) ;
#42707 = CARTESIAN_POINT ( 'NONE',  ( -11.13054826722767032, 24.50000000000006395, -3.146497629411399100 ) ) ;
#42708 = EDGE_CURVE ( 'NONE', #883, #22818, #10579, .T. ) ;
#42709 = VECTOR ( 'NONE', #9038, 1000.000000000000227 ) ;
#42710 = VECTOR ( 'NONE', #33845, 1000.000000000000227 ) ;
#42711 = VERTEX_POINT ( 'NONE', #9427 ) ;
#42712 = DIRECTION ( 'NONE',  ( -0.005961354470445682716, -0.6427876096865404731, 0.7660212471507180654 ) ) ;
#42713 = EDGE_LOOP ( 'NONE', ( #8883, #24255, #33390, #13261 ) ) ;
#42714 = EDGE_LOOP ( 'NONE', ( #46554, #46854, #40691, #38473 ) ) ;
#42715 = ADVANCED_FACE ( 'NONE', ( #14278 ), #26753, .F. ) ;
#42716 = DIRECTION ( 'NONE',  ( 0.9321478471874541372, 0.000000000000000000, -0.3620778797217453771 ) ) ;
#42717 = DIRECTION ( 'NONE',  ( 0.9999697198139515519, 0.000000000000000000, 0.007781995580013368816 ) ) ;
#42718 = CARTESIAN_POINT ( 'NONE',  ( -14.10280672071693431, -0.1191753592594197858, 12.40843558753103792 ) ) ;
#42719 = DIRECTION ( 'NONE',  ( -0.9999697198139514409, -0.000000000000000000, -0.007781995580013368816 ) ) ;
#42720 = EDGE_LOOP ( 'NONE', ( #27175, #47450, #14177, #39787 ) ) ;
#42721 = ORIENTED_EDGE ( 'NONE', *, *, #47202, .T. ) ;
#42722 = VECTOR ( 'NONE', #48823, 999.9999999999998863 ) ;
#42723 = DIRECTION ( 'NONE',  ( 0.05705673239519650636, -0.9983709377222390602, -2.328121953249066419E-16 ) ) ;
#42724 = CARTESIAN_POINT ( 'NONE',  ( -24.53375310857961367, 18.49370688441070953, -4.657437592157546824 ) ) ;
#42725 = PRODUCT_DEFINITION_CONTEXT ( 'detailed design', #17331, 'design' ) ;
#42726 = VECTOR ( 'NONE', #810, 1000.000000000000227 ) ;
#42727 = CARTESIAN_POINT ( 'NONE',  ( -18.15912818816975616, 0.000000000000000000, 9.111073428781198302 ) ) ;
#42728 = FACE_OUTER_BOUND ( 'NONE', #39167, .T. ) ;
#42729 = LINE ( 'NONE', #34249, #2263 ) ;
#42730 = CARTESIAN_POINT ( 'NONE',  ( -20.05622291350217523, 5.305366725996512045, 13.37884985175888097 ) ) ;
#42731 = VERTEX_POINT ( 'NONE', #5731 ) ;
#42732 = LINE ( 'NONE', #33949, #6599 ) ;
#42733 = FACE_OUTER_BOUND ( 'NONE', #51289, .T. ) ;
#42734 = VERTEX_POINT ( 'NONE', #9991 ) ;
#42735 = DIRECTION ( 'NONE',  ( 0.6427681459581294776, -0.7660444431189769032, 0.005002170337467562802 ) ) ;
#42736 = DIRECTION ( 'NONE',  ( 0.000000000000000000, -0.000000000000000000, -1.000000000000000000 ) ) ;
#42737 = ADVANCED_FACE ( 'NONE', ( #27299 ), #27595, .F. ) ;
#42738 = PLANE ( 'NONE',  #34997 ) ;
#42739 = CARTESIAN_POINT ( 'NONE',  ( -13.27065584551087163, 0.000000000000000000, 12.04557950825129176 ) ) ;
#42740 = VERTEX_POINT ( 'NONE', #40377 ) ;
#42741 = ORIENTED_EDGE ( 'NONE', *, *, #53268, .F. ) ;
#42742 = CARTESIAN_POINT ( 'NONE',  ( -13.61183992779837304, 1.581621852479004442, 4.764332917083475394 ) ) ;
#42743 = CARTESIAN_POINT ( 'NONE',  ( -20.63663879154963965, 20.74370688441071664, 4.329123301634322907 ) ) ;
#42744 = LINE ( 'NONE', #17200, #35159 ) ;
#42745 = ADVANCED_FACE ( 'NONE', ( #44613 ), #5194, .F. ) ;
#42746 = VECTOR ( 'NONE', #11560, 1000.000000000000227 ) ;
#42747 = VECTOR ( 'NONE', #2502, 999.9999999999998863 ) ;
#42748 = DIRECTION ( 'NONE',  ( 0.007781995580012662783, 0.000000000000000000, -0.9999697198139514409 ) ) ;
#42749 = DIRECTION ( 'NONE',  ( -0.005961354470445682716, -0.6427876096865404731, 0.7660212471507180654 ) ) ;
#42750 = LINE ( 'NONE', #139, #19206 ) ;
#42751 = LINE ( 'NONE', #3856, #27476 ) ;
#42752 = EDGE_CURVE ( 'NONE', #51326, #12359, #2000, .T. ) ;
#42753 = LINE ( 'NONE', #3858, #43207 ) ;
#42754 = DIRECTION ( 'NONE',  ( 0.007781995580012662783, 0.000000000000000000, -0.9999697198139514409 ) ) ;
#42755 = VECTOR ( 'NONE', #16001, 999.9999999999998863 ) ;
#42756 = LINE ( 'NONE', #2723, #47378 ) ;
#42757 = EDGE_LOOP ( 'NONE', ( #48693, #31041, #25396, #48819 ) ) ;
#42758 = LINE ( 'NONE', #49945, #20425 ) ;
#42759 = ORIENTED_EDGE ( 'NONE', *, *, #50126, .T. ) ;
#42760 = EDGE_CURVE ( 'NONE', #54234, #26894, #52583, .T. ) ;
#42761 = ORIENTED_EDGE ( 'NONE', *, *, #26611, .T. ) ;
#42762 = VECTOR ( 'NONE', #22959, 1000.000000000000227 ) ;
#42763 = ADVANCED_FACE ( 'NONE', ( #897 ), #55114, .F. ) ;
#42764 = ORIENTED_EDGE ( 'NONE', *, *, #52400, .F. ) ;
#42765 = ORIENTED_EDGE ( 'NONE', *, *, #53265, .T. ) ;
#42766 = ORIENTED_EDGE ( 'NONE', *, *, #43866, .T. ) ;
#42767 = VERTEX_POINT ( 'NONE', #37214 ) ;
#42768 = CARTESIAN_POINT ( 'NONE',  ( -19.41128072241421165, -4.241740624735661491, 11.18335138056985834 ) ) ;
#42769 = FACE_OUTER_BOUND ( 'NONE', #13923, .T. ) ;
#42770 = CARTESIAN_POINT ( 'NONE',  ( -20.54049170961573267, 0.000000000000000000, 4.660556269540326646 ) ) ;
#42771 = ADVANCED_FACE ( 'NONE', ( #36967 ), #15928, .F. ) ;
#42772 = ORIENTED_EDGE ( 'NONE', *, *, #19666, .F. ) ;
#42773 = DIRECTION ( 'NONE',  ( 0.9999697198139515519, 0.000000000000000000, 0.007781995580013368816 ) ) ;
#42774 = EDGE_LOOP ( 'NONE', ( #39876, #21912, #54844, #53492 ) ) ;
#42775 = DIRECTION ( 'NONE',  ( 0.005961354470445682716, -0.6427876096865404731, -0.7660212471507180654 ) ) ;
#42776 = ORIENTED_EDGE ( 'NONE', *, *, #44688, .T. ) ;
#42777 = EDGE_CURVE ( 'NONE', #21762, #17219, #10831, .T. ) ;
#42778 = CARTESIAN_POINT ( 'NONE',  ( -69.17557446582597436, -9.021883352441653514, 7.567125991932351248 ) ) ;
#42779 = PLANE ( 'NONE',  #50824 ) ;
#42780 = CARTESIAN_POINT ( 'NONE',  ( -19.60990026154428278, 0.000000000000000000, 4.498472333781370125 ) ) ;
#42781 = ORIENTED_EDGE ( 'NONE', *, *, #47577, .F. ) ;
#42782 = PLANE ( 'NONE',  #54582 ) ;
#42783 = ORIENTED_EDGE ( 'NONE', *, *, #6754, .T. ) ;
#42784 = VECTOR ( 'NONE', #13453, 999.9999999999998863 ) ;
#42785 = VECTOR ( 'NONE', #10824, 999.9999999999998863 ) ;
#42786 = CARTESIAN_POINT ( 'NONE',  ( -18.67619601524082285, 0.000000000000000000, 3.936400510096834893 ) ) ;
#42787 = FACE_OUTER_BOUND ( 'NONE', #16171, .T. ) ;
#42788 = CARTESIAN_POINT ( 'NONE',  ( -18.39746900504187010, 0.000000000000000000, 14.03700784672088808 ) ) ;
#42789 = AXIS2_PLACEMENT_3D ( 'NONE', #4285, #42870, #42334 ) ;
#42790 = CARTESIAN_POINT ( 'NONE',  ( -18.25128119919330416, -0.1191753592594153865, 8.102363091431291409 ) ) ;
#42791 = CARTESIAN_POINT ( 'NONE',  ( -10.89619124762234392, 0.000000000000000000, 5.474274585375703772 ) ) ;
#42792 = CARTESIAN_POINT ( 'NONE',  ( -10.27421835998572064, 0.000000000000000000, 10.96090226820206048 ) ) ;
#42793 = CARTESIAN_POINT ( 'NONE',  ( -14.87505532172404443, 0.000000000000000000, 5.073978075321856629 ) ) ;
#42794 = CARTESIAN_POINT ( 'NONE',  ( -68.87050791938486327, -8.585715889274700530, -6.450409451741323075 ) ) ;
#42795 = ORIENTED_EDGE ( 'NONE', *, *, #26993, .F. ) ;
#42796 = CARTESIAN_POINT ( 'NONE',  ( -55.54282512360118318, 6.653076535853754692, -1.248217177980195380 ) ) ;
#42797 = ORIENTED_EDGE ( 'NONE', *, *, #20200, .F. ) ;
#42798 = ADVANCED_FACE ( 'NONE', ( #19898 ), #29254, .F. ) ;
#42799 = CARTESIAN_POINT ( 'NONE',  ( -15.13495153988577968, 0.000000000000000000, 12.76973526769478084 ) ) ;
#42800 = LINE ( 'NONE', #46495, #16008 ) ;
#42801 = PLANE ( 'NONE',  #54405 ) ;
#42802 = VECTOR ( 'NONE', #5577, 1000.000000000000227 ) ;
#42803 = EDGE_CURVE ( 'NONE', #45114, #26051, #46281, .T. ) ;
#42804 = CARTESIAN_POINT ( 'NONE',  ( -18.68432617547731311, -0.1191753592594153865, 4.039253233279383792 ) ) ;
#42805 = CARTESIAN_POINT ( 'NONE',  ( 2.072287782118878319, 0.000000000000000000, -2.950529333540147015 ) ) ;
#42806 = AXIS2_PLACEMENT_3D ( 'NONE', #33442, #35336, #38834 ) ;
#42807 = LINE ( 'NONE', #43650, #45663 ) ;
#42808 = APPLICATION_PROTOCOL_DEFINITION ( 'draft international standard', 'automotive_design', 1998, #1749 ) ;
#42809 = ORIENTED_EDGE ( 'NONE', *, *, #47724, .F. ) ;
#42810 = ADVANCED_FACE ( 'NONE', ( #54519 ), #41496, .F. ) ;
#42811 = CARTESIAN_POINT ( 'NONE',  ( -11.64271541837342028, 0.000000000000000000, 7.684457380502274226 ) ) ;
#42812 = DIRECTION ( 'NONE',  ( 0.5364919789714477361, 0.6444004775717706579, 0.5449076811759711036 ) ) ;
#42813 = LINE ( 'NONE', #41692, #49939 ) ;
#42814 = EDGE_CURVE ( 'NONE', #45339, #46146, #16205, .T. ) ;
#42815 = EDGE_CURVE ( 'NONE', #53717, #37763, #32676, .T. ) ;
#42816 = EDGE_CURVE ( 'NONE', #3505, #22811, #20469, .T. ) ;
#42817 = DIRECTION ( 'NONE',  ( 0.3535533905932738974, -0.6123724356957929160, -0.7071067811865487940 ) ) ;
#42818 = PLANE ( 'NONE',  #29352 ) ;
#42819 = VECTOR ( 'NONE', #7622, 999.9999999999998863 ) ;
#42820 = FACE_OUTER_BOUND ( 'NONE', #40195, .T. ) ;
#42821 = CARTESIAN_POINT ( 'NONE',  ( 5.057731014323089802, -1.114607557371862567, -2.289010529401726224 ) ) ;
#42822 = EDGE_LOOP ( 'NONE', ( #54496, #19118, #32658, #12594 ) ) ;
#42823 = CARTESIAN_POINT ( 'NONE',  ( -26.13493519185646008, 0.000000000000000000, 7.033017491833586377 ) ) ;
#42824 = PLANE ( 'NONE',  #4224 ) ;
#42825 = VERTEX_POINT ( 'NONE', #6563 ) ;
#42826 = VECTOR ( 'NONE', #7802, 1000.000000000000227 ) ;
#42827 = ORIENTED_EDGE ( 'NONE', *, *, #16103, .F. ) ;
#42828 = DIRECTION ( 'NONE',  ( 0.005002170337468016433, -0.7660444431189770143, -0.6427681459581293666 ) ) ;
#42829 = VECTOR ( 'NONE', #25802, 999.9999999999998863 ) ;
#42830 = B_SPLINE_CURVE_WITH_KNOTS ( 'NONE', 3,
 ( #53255, #27111, #44416, #22302, #709, #5813, #1554 ),
 .UNSPECIFIED., .F., .F.,
 ( 4, 3, 4 ),
 ( 0.000000000000000000, 0.0007529153636991639358, 0.001137651663043191038 ),
 .UNSPECIFIED. ) ;
#42831 = AXIS2_PLACEMENT_3D ( 'NONE', #28714, #6850, #7128 ) ;
#42832 = ORIENTED_EDGE ( 'NONE', *, *, #12093, .F. ) ;
#42833 = ADVANCED_FACE ( 'NONE', ( #42338 ), #23877, .F. ) ;
#42834 = EDGE_CURVE ( 'NONE', #41663, #15067, #36674, .T. ) ;
#42835 = VECTOR ( 'NONE', #20710, 1000.000000000000227 ) ;
#42836 = VERTEX_POINT ( 'NONE', #11669 ) ;
#42837 = VERTEX_POINT ( 'NONE', #32963 ) ;
#42838 = VECTOR ( 'NONE', #17537, 1000.000000000000227 ) ;
#42839 = ORIENTED_EDGE ( 'NONE', *, *, #33593, .F. ) ;
#42840 = EDGE_CURVE ( 'NONE', #30427, #54774, #32432, .T. ) ;
#42841 = CARTESIAN_POINT ( 'NONE',  ( -16.46071592345537127, -2.460819163488160655, 3.196709174999311731 ) ) ;
#42842 = VERTEX_POINT ( 'NONE', #2833 ) ;
#42843 = DIRECTION ( 'NONE',  ( -0.005961354470445682716, -0.6427876096865404731, 0.7660212471507180654 ) ) ;
#42844 = CARTESIAN_POINT ( 'NONE',  ( -22.40634380310664397, 0.000000000000000000, 5.584705972946605534 ) ) ;
#42845 = EDGE_CURVE ( 'NONE', #21631, #16580, #40574, .T. ) ;
#42846 = ORIENTED_EDGE ( 'NONE', *, *, #40665, .T. ) ;
#42847 = AXIS2_PLACEMENT_3D ( 'NONE', #4125, #48383, #17176 ) ;
#42848 = ORIENTED_EDGE ( 'NONE', *, *, #18039, .F. ) ;
#42849 = EDGE_CURVE ( 'NONE', #15326, #18261, #41743, .T. ) ;
#42850 = CARTESIAN_POINT ( 'NONE',  ( -65.60662997296927301, -1.821459649775648396E-14, 0.6641167203969936539 ) ) ;
#42851 = CARTESIAN_POINT ( 'NONE',  ( -17.86419527468779123, 5.467268677019012202, 12.79310055922187495 ) ) ;
#42852 = VERTEX_POINT ( 'NONE', #20161 ) ;
#42853 = LINE ( 'NONE', #30083, #14654 ) ;
#42854 = LINE ( 'NONE', #17040, #34058 ) ;
#42855 = EDGE_LOOP ( 'NONE', ( #38756, #14011, #12514, #26153 ) ) ;
#42856 = LINE ( 'NONE', #20992, #4031 ) ;
#42857 = ORIENTED_EDGE ( 'NONE', *, *, #10154, .T. ) ;
#42858 = CARTESIAN_POINT ( 'NONE',  ( -14.20280369269832832, 0.000000000000000000, 12.40765738797303719 ) ) ;
#42859 = VECTOR ( 'NONE', #47738, 1000.000000000000114 ) ;
#42860 = DIRECTION ( 'NONE',  ( -0.5449076811759708816, 0.6444004775717707689, 0.5364919789714475140 ) ) ;
#42861 = EDGE_LOOP ( 'NONE', ( #36749, #35274, #27059, #46110 ) ) ;
#42862 = CARTESIAN_POINT ( 'NONE',  ( -12.13851405436063047, 0.000000000000000000, 11.68505802764555135 ) ) ;
#42863 = CARTESIAN_POINT ( 'NONE',  ( -13.08408713167409942, -0.1191753592594197858, 1.863930203747758085 ) ) ;
#42864 = LINE ( 'NONE', #12773, #52977 ) ;
#42865 = VECTOR ( 'NONE', #35881, 1000.000000000000227 ) ;
#42866 = CARTESIAN_POINT ( 'NONE',  ( -13.59275766711197519, -3.432230869623159819, 7.594696008263455589 ) ) ;
#42867 = ORIENTED_EDGE ( 'NONE', *, *, #37079, .T. ) ;
#42868 = VECTOR ( 'NONE', #52323, 1000.000000000000227 ) ;
#42869 = VECTOR ( 'NONE', #34311, 999.9999999999998863 ) ;
#42870 = DIRECTION ( 'NONE',  ( 0.000000000000000000, -1.000000000000000000, 0.000000000000000000 ) ) ;
#42871 = DIRECTION ( 'NONE',  ( 0.7660212471507180654, -0.6427876096865404731, 0.005961354470445141482 ) ) ;
#42872 = CARTESIAN_POINT ( 'NONE',  ( -12.28182988935405895, -4.079838673713161334, 8.148321875889408261 ) ) ;
#42873 = DIRECTION ( 'NONE',  ( 0.5449076811759707706, 0.6444004775717708799, -0.5364919789714476250 ) ) ;
#42874 = LINE ( 'NONE', #3983, #4100 ) ;
#42875 = CARTESIAN_POINT ( 'NONE',  ( 2.072287782118878319, 0.000000000000000000, -2.950529333540147015 ) ) ;
#42876 = VECTOR ( 'NONE', #15210, 1000.000000000000000 ) ;
#42877 = DIRECTION ( 'NONE',  ( -0.5449076811759708816, 0.6444004775717707689, 0.5364919789714475140 ) ) ;
#42878 = DIRECTION ( 'NONE',  ( 0.007781995580012663651, 0.000000000000000000, -0.9999697198139515519 ) ) ;
#42879 = VECTOR ( 'NONE', #19906, 1000.000000000000227 ) ;
#42880 = EDGE_LOOP ( 'NONE', ( #14599, #8426, #774, #20179 ) ) ;
#42881 = FILL_AREA_STYLE ('',( #43710 ) ) ;
#42882 = LINE ( 'NONE', #7396, #20536 ) ;
#42883 = EDGE_LOOP ( 'NONE', ( #7827, #28891, #34136, #42894 ) ) ;
#42884 = LINE ( 'NONE', #25302, #14800 ) ;
#42885 = CARTESIAN_POINT ( 'NONE',  ( -12.77198315601838630, 0.000000000000000000, 7.675669157850252944 ) ) ;
#42886 = EDGE_CURVE ( 'NONE', #34831, #26641, #50275, .T. ) ;
#42887 = EDGE_CURVE ( 'NONE', #29025, #1604, #50574, .T. ) ;
#42888 = DIRECTION ( 'NONE',  ( 0.005961354470445682716, -0.6427876096865404731, -0.7660212471507180654 ) ) ;
#42889 = VECTOR ( 'NONE', #49668, 999.9999999999998863 ) ;
#42890 = ADVANCED_FACE ( 'NONE', ( #55963 ), #34374, .F. ) ;
#42891 = AXIS2_PLACEMENT_3D ( 'NONE', #51317, #11576, #37384 ) ;
#42892 = DIRECTION ( 'NONE',  ( -0.005961354470445682716, -0.6427876096865404731, 0.7660212471507180654 ) ) ;
#42893 = FACE_OUTER_BOUND ( 'NONE', #50812, .T. ) ;
#42894 = ORIENTED_EDGE ( 'NONE', *, *, #34388, .T. ) ;
#42895 = ORIENTED_EDGE ( 'NONE', *, *, #45115, .F. ) ;
#42896 = LINE ( 'NONE', #21331, #54007 ) ;
#42897 = FACE_OUTER_BOUND ( 'NONE', #52265, .T. ) ;
#42898 = EDGE_LOOP ( 'NONE', ( #21198, #46129, #53658, #48731 ) ) ;
#42899 = VECTOR ( 'NONE', #41606, 1000.000000000000227 ) ;
#42900 = DIRECTION ( 'NONE',  ( 0.007781995580012663651, 0.000000000000000000, -0.9999697198139515519 ) ) ;
#42901 = ORIENTED_EDGE ( 'NONE', *, *, #16202, .F. ) ;
#42902 = PLANE ( 'NONE',  #15886 ) ;
#42903 = AXIS2_PLACEMENT_3D ( 'NONE', #45219, #49181, #49486 ) ;
#42904 = EDGE_LOOP ( 'NONE', ( #32609, #6473, #53711, #6224 ) ) ;
#42905 = CARTESIAN_POINT ( 'NONE',  ( -3.360905869600907092, 1.712176620043476140E-14, -4.599999999999999645 ) ) ;
#42906 = EDGE_CURVE ( 'NONE', #30294, #35325, #29840, .T. ) ;
#42907 = ORIENTED_EDGE ( 'NONE', *, *, #49440, .F. ) ;
#42908 = VERTEX_POINT ( 'NONE', #26139 ) ;
#42909 = VERTEX_POINT ( 'NONE', #29567 ) ;
#42910 = LINE ( 'NONE', #34139, #35684 ) ;
#42911 = VECTOR ( 'NONE', #23013, 1000.000000000000000 ) ;
#42912 = DIRECTION ( 'NONE',  ( 0.000000000000000000, -1.000000000000000000, 0.000000000000000000 ) ) ;
#42913 = CARTESIAN_POINT ( 'NONE',  ( -16.43317633868556626, -0.1191753592594197858, 13.31363028683540151 ) ) ;
#42914 = VECTOR ( 'NONE', #32987, 999.9999999999998863 ) ;
#42915 = AXIS2_PLACEMENT_3D ( 'NONE', #12925, #21468, #21160 ) ;
#42916 = EDGE_CURVE ( 'NONE', #14453, #38228, #43448, .T. ) ;
#42917 = FACE_OUTER_BOUND ( 'NONE', #1794, .T. ) ;
#42918 = VERTEX_POINT ( 'NONE', #8528 ) ;
#42919 = VERTEX_POINT ( 'NONE', #51678 ) ;
#42920 = EDGE_CURVE ( 'NONE', #11836, #54577, #21008, .T. ) ;
#42921 = AXIS2_PLACEMENT_3D ( 'NONE', #5424, #22734, #18469 ) ;
#42922 = VERTEX_POINT ( 'NONE', #7985 ) ;
#42923 = DIRECTION ( 'NONE',  ( 0.007781995580012663651, -3.146120232559066537E-19, -0.9999697198139514409 ) ) ;
#42924 = AXIS2_PLACEMENT_3D ( 'NONE', #11615, #28934, #46504 ) ;
#42925 = EDGE_CURVE ( 'NONE', #23586, #6615, #38546, .T. ) ;
#42926 = DIRECTION ( 'NONE',  ( -0.6427681459581293666, -0.7660444431189770143, -0.005002170337467561935 ) ) ;
#42927 = VERTEX_POINT ( 'NONE', #12782 ) ;
#42928 = DIRECTION ( 'NONE',  ( 0.005961354470445682716, -0.6427876096865404731, -0.7660212471507180654 ) ) ;
#42929 = ADVANCED_FACE ( 'NONE', ( #8240 ), #47986, .F. ) ;
#42930 = ORIENTED_EDGE ( 'NONE', *, *, #4194, .F. ) ;
#42931 = CARTESIAN_POINT ( 'NONE',  ( -18.28212116572951373, -0.1941918491731542684, 3.976522104704446114 ) ) ;
#42932 = PLANE ( 'NONE',  #13114 ) ;
#42933 = ORIENTED_EDGE ( 'NONE', *, *, #11182, .F. ) ;
#42934 = EDGE_CURVE ( 'NONE', #19674, #44901, #17309, .T. ) ;
#42935 = DIRECTION ( 'NONE',  ( 0.5449076811759707706, 0.6444004775717708799, -0.5364919789714476250 ) ) ;
#42936 = EDGE_LOOP ( 'NONE', ( #27653, #14395, #42839, #44260, #43576, #53346 ) ) ;
#42937 = FACE_OUTER_BOUND ( 'NONE', #2921, .T. ) ;
#42938 = LINE ( 'NONE', #26967, #21175 ) ;
#42939 = VECTOR ( 'NONE', #39219, 1000.000000000000114 ) ;
#42940 = ORIENTED_EDGE ( 'NONE', *, *, #45776, .T. ) ;
#42941 = CARTESIAN_POINT ( 'NONE',  ( -18.69774841163365764, -4.565544526780663581, 3.998496804814759109 ) ) ;
#42942 = PLANE ( 'NONE',  #40209 ) ;
#42943 = DIRECTION ( 'NONE',  ( 0.007781995580012662783, 0.000000000000000000, -0.9999697198139514409 ) ) ;
#42944 = ORIENTED_EDGE ( 'NONE', *, *, #2818, .F. ) ;
#42945 = VECTOR ( 'NONE', #1084, 1000.000000000000227 ) ;
#42946 = DIRECTION ( 'NONE',  ( -0.7660212471507179544, -0.6427876096865405842, -0.005961354470445141482 ) ) ;
#42947 = CARTESIAN_POINT ( 'NONE',  ( -68.47885788718261324, 1.837926688830805233, 7.469119143268239114 ) ) ;
#42948 = VECTOR ( 'NONE', #18833, 1000.000000000000000 ) ;
#42949 = CARTESIAN_POINT ( 'NONE',  ( -36.91819796696599099, -1.000000000000000000, 21.84982018086542155 ) ) ;
#42950 = CARTESIAN_POINT ( 'NONE',  ( -17.74404816805336793, 0.000000000000000000, 3.574322630375089460 ) ) ;
#42951 = LINE ( 'NONE', #7765, #48780 ) ;
#42952 = LINE ( 'NONE', #9430, #10462 ) ;
#42953 = VERTEX_POINT ( 'NONE', #43189 ) ;
#42954 = DIRECTION ( 'NONE',  ( 0.007781995580012663651, 0.000000000000000000, -0.9999697198139515519 ) ) ;
#42955 = FACE_OUTER_BOUND ( 'NONE', #1190, .T. ) ;
#42956 = DIRECTION ( 'NONE',  ( -0.6427681459581293666, -0.7660444431189770143, -0.005002170337467561935 ) ) ;
#42957 = ORIENTED_EDGE ( 'NONE', *, *, #39971, .F. ) ;
#42958 = VECTOR ( 'NONE', #50537, 1000.000000000000227 ) ;
#42959 = CARTESIAN_POINT ( 'NONE',  ( -9.951229532024482793, 0.000000000000000000, 3.465642133327924146 ) ) ;
#42960 = DIRECTION ( 'NONE',  ( 0.000000000000000000, -1.000000000000000000, 0.000000000000000000 ) ) ;
#42961 = EDGE_LOOP ( 'NONE', ( #23148, #50996, #55285, #55283 ) ) ;
#42962 = VECTOR ( 'NONE', #21658, 1000.000000000000000 ) ;
#42963 = EDGE_CURVE ( 'NONE', #22414, #50687, #17605, .T. ) ;
#42964 = DIRECTION ( 'NONE',  ( -0.000000000000000000, -1.000000000000000000, -0.000000000000000000 ) ) ;
#42965 = DIRECTION ( 'NONE',  ( 0.005961354470445682716, -0.6427876096865404731, -0.7660212471507180654 ) ) ;
#42966 = EDGE_CURVE ( 'NONE', #41657, #53717, #42874, .T. ) ;
#42967 = ADVANCED_FACE ( 'NONE', ( #13370 ), #47418, .F. ) ;
#42968 = DIRECTION ( 'NONE',  ( 0.7660212471507180654, -0.6427876096865404731, 0.005961354470445141482 ) ) ;
#42969 = CARTESIAN_POINT ( 'NONE',  ( -67.27285806668032819, 2.000000000017658319, 1.402349447196803434 ) ) ;
#42970 = ORIENTED_EDGE ( 'NONE', *, *, #24806, .F. ) ;
#42971 = VECTOR ( 'NONE', #7339, 1000.000000000000227 ) ;
#42972 = VECTOR ( 'NONE', #7623, 999.9999999999998863 ) ;
#42973 = ORIENTED_EDGE ( 'NONE', *, *, #37010, .F. ) ;
#42974 = CARTESIAN_POINT ( 'NONE',  ( -67.03575697379285714, -0.6010133368208401272, -0.6652792357935631840 ) ) ;
#42975 = PLANE ( 'NONE',  #32258 ) ;
#42976 = DIRECTION ( 'NONE',  ( 0.7660212471507180654, -0.6427876096865404731, 0.005961354470445141482 ) ) ;
#42977 = DIRECTION ( 'NONE',  ( -0.7660212471507179544, -0.6427876096865405842, -0.005961354470445141482 ) ) ;
#42978 = CARTESIAN_POINT ( 'NONE',  ( -22.40478740399063895, 0.000000000000000000, 5.384712028983816623 ) ) ;
#42979 = CARTESIAN_POINT ( 'NONE',  ( -13.46964841717965911, 0.000000000000000000, 3.607586997594828038 ) ) ;
#42980 = ORIENTED_EDGE ( 'NONE', *, *, #18388, .T. ) ;
#42981 = PLANE ( 'NONE',  #5667 ) ;
#42982 = EDGE_CURVE ( 'NONE', #25199, #6556, #38917, .T. ) ;
#42983 = CARTESIAN_POINT ( 'NONE',  ( -17.46139143058123011, 5.629170628041515023, 3.284929139499369377 ) ) ;
#42984 = ORIENTED_EDGE ( 'NONE', *, *, #28483, .F. ) ;
#42985 = VECTOR ( 'NONE', #51157, 999.9999999999998863 ) ;
#42986 = FACE_OUTER_BOUND ( 'NONE', #47248, .T. ) ;
#42987 = DIRECTION ( 'NONE',  ( 0.2113248654051873565, 0.7886751345948123104, 0.5773502691896265082 ) ) ;
#42988 = AXIS2_PLACEMENT_3D ( 'NONE', #18024, #35346, #52645 ) ;
#42989 = DIRECTION ( 'NONE',  ( 0.007781995580012663651, 0.000000000000000000, -0.9999697198139515519 ) ) ;
#42990 = ORIENTED_EDGE ( 'NONE', *, *, #51483, .F. ) ;
#42991 = CARTESIAN_POINT ( 'NONE',  ( -10.23443446032375270, 0.000000000000000000, 5.848756599517480836 ) ) ;
#42992 = VECTOR ( 'NONE', #21791, 1000.000000000000114 ) ;
#42993 = VERTEX_POINT ( 'NONE', #52259 ) ;
#42994 = ADVANCED_FACE ( 'NONE', ( #3692 ), #8835, .F. ) ;
#42995 = EDGE_LOOP ( 'NONE', ( #27409, #37670, #29813, #50631 ) ) ;
#42996 = EDGE_LOOP ( 'NONE', ( #3536, #7695, #28572, #26176 ) ) ;
#42997 = ORIENTED_EDGE ( 'NONE', *, *, #17056, .F. ) ;
#42998 = AXIS2_PLACEMENT_3D ( 'NONE', #37247, #41242, #32461 ) ;
#42999 = DIRECTION ( 'NONE',  ( -0.005961354470445682716, -0.6427876096865404731, 0.7660212471507180654 ) ) ;
#43000 = ORIENTED_EDGE ( 'NONE', *, *, #23298, .F. ) ;
#43001 = CARTESIAN_POINT ( 'NONE',  ( -14.91381621359531984, 22.31572923274821463, -3.910276045922330912 ) ) ;
#43002 = STYLED_ITEM ( 'NONE', ( #20150 ), #41703 ) ;
#43003 = ORIENTED_EDGE ( 'NONE', *, *, #9277, .T. ) ;
#43004 = LINE ( 'NONE', #38767, #34077 ) ;
#43005 = ADVANCED_FACE ( 'NONE', ( #20748 ), #38064, .F. ) ;
#43006 = ORIENTED_EDGE ( 'NONE', *, *, #32491, .T. ) ;
#43007 = CARTESIAN_POINT ( 'NONE',  ( -11.20636620717317378, 0.000000000000000000, 11.32298014792380414 ) ) ;
#43008 = ORIENTED_EDGE ( 'NONE', *, *, #5494, .T. ) ;
#43009 = AXIS2_PLACEMENT_3D ( 'NONE', #29198, #12166, #29503 ) ;
#43010 = VECTOR ( 'NONE', #50448, 1000.000000000000227 ) ;
#43011 = DIRECTION ( 'NONE',  ( 0.2426528472758542054, 0.7422098413412800966, 0.6246952433987894571 ) ) ;
#43012 = CARTESIAN_POINT ( 'NONE',  ( -15.34831437908097840, 0.000000000000000000, 6.178291273327141120 ) ) ;
#43013 = CARTESIAN_POINT ( 'NONE',  ( -25.92429756520238016, 17.40220053346460105, -4.407437592157546824 ) ) ;
#43014 = CARTESIAN_POINT ( 'NONE',  ( 2.072287782118878319, 0.000000000000000000, -2.950529333540147015 ) ) ;
#43015 = CARTESIAN_POINT ( 'NONE',  ( -9.342070512798265725, 0.000000000000000000, 10.59882438848031505 ) ) ;
#43016 = ORIENTED_EDGE ( 'NONE', *, *, #44966, .T. ) ;
#43017 = EDGE_CURVE ( 'NONE', #2042, #2367, #25295, .T. ) ;
#43018 = ORIENTED_EDGE ( 'NONE', *, *, #38217, .F. ) ;
#43019 = LINE ( 'NONE', #48107, #4107 ) ;
#43020 = DIRECTION ( 'NONE',  ( 0.005961354470445682716, -0.6427876096865404731, -0.7660212471507180654 ) ) ;
#43021 = EDGE_CURVE ( 'NONE', #294, #26160, #16766, .T. ) ;
#43022 = ADVANCED_FACE ( 'NONE', ( #12522 ), #49386, .F. ) ;
#43023 = DIRECTION ( 'NONE',  ( 0.5449076811759707706, 0.6444004775717708799, -0.5364919789714476250 ) ) ;
#43024 = VECTOR ( 'NONE', #3815, 1000.000000000000114 ) ;
#43025 = CARTESIAN_POINT ( 'NONE',  ( -15.52818994850678891, 0.000000000000000000, 3.591566951406786057 ) ) ;
#43026 = AXIS2_PLACEMENT_3D ( 'NONE', #13050, #8224, #38615 ) ;
#43027 = CARTESIAN_POINT ( 'NONE',  ( -17.74482636761137044, -0.1191753592594197858, 3.674319602356483916 ) ) ;
#43028 = CARTESIAN_POINT ( 'NONE',  ( -14.77973024485960529, 4.657758921906512306, 2.274273984692230410 ) ) ;
#43029 = ORIENTED_EDGE ( 'NONE', *, *, #27384, .F. ) ;
#43030 = FACE_OUTER_BOUND ( 'NONE', #44300, .T. ) ;
#43031 = ADVANCED_FACE ( 'NONE', ( #14213 ), #13896, .F. ) ;
#43032 = CARTESIAN_POINT ( 'NONE',  ( 5.454592090961234874, -6.230699628392517120, -2.061810099490657411 ) ) ;
#43033 = VECTOR ( 'NONE', #26453, 1000.000000000000227 ) ;
#43034 = ORIENTED_EDGE ( 'NONE', *, *, #18897, .T. ) ;
#43035 = LINE ( 'NONE', #55518, #19778 ) ;
#43036 = DIRECTION ( 'NONE',  ( 0.5449076811759707706, 0.6444004775717708799, -0.5364919789714476250 ) ) ;
#43037 = ADVANCED_FACE ( 'NONE', ( #48839 ), #14741, .F. ) ;
#43038 = DIRECTION ( 'NONE',  ( 0.007781995580012663651, 0.000000000000000000, -0.9999697198139515519 ) ) ;
#43039 = EDGE_CURVE ( 'NONE', #47891, #36269, #53633, .T. ) ;
#43040 = CARTESIAN_POINT ( 'NONE',  ( -11.50282600055954951, -2.622721114510657703, 5.454352154844033684 ) ) ;
#43041 = ORIENTED_EDGE ( 'NONE', *, *, #8680, .F. ) ;
#43042 = VECTOR ( 'NONE', #43326, 999.9999999999998863 ) ;
#43043 = ORIENTED_EDGE ( 'NONE', *, *, #34523, .T. ) ;
#43044 = VECTOR ( 'NONE', #37129, 1000.000000000000227 ) ;
#43045 = PLANE ( 'NONE',  #45708 ) ;
#43046 = DIRECTION ( 'NONE',  ( 0.000000000000000000, -1.000000000000000000, 0.000000000000000000 ) ) ;
#43047 = DIRECTION ( 'NONE',  ( 0.007781995580012663651, 0.000000000000000000, -0.9999697198139515519 ) ) ;
#43048 = VECTOR ( 'NONE', #6364, 1000.000000000000227 ) ;
#43049 = EDGE_CURVE ( 'NONE', #19374, #48095, #27239, .T. ) ;
#43050 = DIRECTION ( 'NONE',  ( 0.9999697198139515519, 0.000000000000000000, 0.007781995580013368816 ) ) ;
#43051 = FACE_OUTER_BOUND ( 'NONE', #37068, .T. ) ;
#43052 = CARTESIAN_POINT ( 'NONE',  ( -19.72849096906270105, 5.467268677019012202, 13.51725631866536759 ) ) ;
#43053 = FACE_OUTER_BOUND ( 'NONE', #23518, .T. ) ;
#43054 = ORIENTED_EDGE ( 'NONE', *, *, #41656, .T. ) ;
#43055 = EDGE_CURVE ( 'NONE', #42382, #2545, #32071, .T. ) ;
#43056 = AXIS2_PLACEMENT_3D ( 'NONE', #9457, #52052, #52891 ) ;
#43057 = DIRECTION ( 'NONE',  ( 0.6427681459581294776, -0.7660444431189769032, 0.005002170337467562802 ) ) ;
#43058 = AXIS2_PLACEMENT_3D ( 'NONE', #4505, #42558, #47945 ) ;
#43059 = FACE_OUTER_BOUND ( 'NONE', #30724, .T. ) ;
#43060 = CARTESIAN_POINT ( 'NONE',  ( -14.98365774870343969, -1.813211359398158029, 2.643631698368467564 ) ) ;
#43061 = VERTEX_POINT ( 'NONE', #4823 ) ;
#43062 = DIRECTION ( 'NONE',  ( 0.5364919789714477361, 0.6444004775717706579, 0.5449076811759711036 ) ) ;
#43063 = ORIENTED_EDGE ( 'NONE', *, *, #41556, .F. ) ;
#43064 = VERTEX_POINT ( 'NONE', #23283 ) ;
#43065 = AXIS2_PLACEMENT_3D ( 'NONE', #19846, #45147, #7087 ) ;
#43066 = ORIENTED_EDGE ( 'NONE', *, *, #27602, .F. ) ;
#43067 = ORIENTED_EDGE ( 'NONE', *, *, #35806, .F. ) ;
#43068 = ORIENTED_EDGE ( 'NONE', *, *, #1850, .F. ) ;
#43069 = VECTOR ( 'NONE', #35992, 1000.000000000000114 ) ;
#43070 = ORIENTED_EDGE ( 'NONE', *, *, #43536, .F. ) ;
#43071 = CARTESIAN_POINT ( 'NONE',  ( -27.06552663992790997, 0.000000000000000000, 7.195101427592543786 ) ) ;
#43072 = DIRECTION ( 'NONE',  ( -0.9999697198139514409, -0.000000000000000000, -0.007781995580013368816 ) ) ;
#43073 = LINE ( 'NONE', #34541, #2253 ) ;
#43074 = AXIS2_PLACEMENT_3D ( 'NONE', #18591, #18886, #35937 ) ;
#43075 = ORIENTED_EDGE ( 'NONE', *, *, #41614, .T. ) ;
#43076 = LINE ( 'NONE', #46777, #52146 ) ;
#43077 = EDGE_CURVE ( 'NONE', #21645, #46158, #22987, .T. ) ;
#43078 = ORIENTED_EDGE ( 'NONE', *, *, #4520, .T. ) ;
#43079 = VECTOR ( 'NONE', #26669, 999.9999999999998863 ) ;
#43080 = DIRECTION ( 'NONE',  ( 0.7660212471507180654, -0.6427876096865404731, 0.005961354470445141482 ) ) ;
#43081 = VERTEX_POINT ( 'NONE', #44551 ) ;
#43082 = VECTOR ( 'NONE', #31637, 1000.000000000000114 ) ;
#43083 = COLOUR_RGB ( '', 0.31764706, 0.68627451, 0.89019608) ;
#43084 = DIRECTION ( 'NONE',  ( -0.6427681459581293666, -0.7660444431189770143, -0.005002170337467561935 ) ) ;
#43085 = VECTOR ( 'NONE', #13483, 1000.000000000000227 ) ;
#43086 = DIRECTION ( 'NONE',  ( 0.007781995580012662783, 0.000000000000000000, -0.9999697198139514409 ) ) ;
#43087 = CARTESIAN_POINT ( 'NONE',  ( -25.20123094555300369, 0.000000000000000000, 6.470945668149052032 ) ) ;
#43088 = ORIENTED_EDGE ( 'NONE', *, *, #36318, .T. ) ;
#43089 = DIRECTION ( 'NONE',  ( -0.6427681459581293666, -0.7660444431189770143, -0.005002170337467561935 ) ) ;
#43090 = ORIENTED_EDGE ( 'NONE', *, *, #40363, .F. ) ;
#43091 = VECTOR ( 'NONE', #51951, 999.9999999999998863 ) ;
#43092 = ADVANCED_FACE ( 'NONE', ( #44844 ), #31789, .F. ) ;
#43093 = DIRECTION ( 'NONE',  ( -0.5449076811759708816, 0.6444004775717707689, 0.5364919789714475140 ) ) ;
#43094 = FACE_OUTER_BOUND ( 'NONE', #13480, .T. ) ;
#43095 = ADVANCED_FACE ( 'NONE', ( #18439 ), #5963, .F. ) ;
#43096 = AXIS2_PLACEMENT_3D ( 'NONE', #7713, #54542, #32989 ) ;
#43097 = DIRECTION ( 'NONE',  ( 0.6427681459581294776, -0.7660444431189769032, 0.005002170337467562802 ) ) ;
#43098 = AXIS2_PLACEMENT_3D ( 'NONE', #3821, #52644, #34495 ) ;
#43099 = CARTESIAN_POINT ( 'NONE',  ( -17.78089619534165067, -0.1191753592594179401, 7.367359596683773937 ) ) ;
#43100 = CARTESIAN_POINT ( 'NONE',  ( -17.29258214062169330, -0.6798977022406558213, 3.576654982803652238 ) ) ;
#43101 = LINE ( 'NONE', #34021, #34868 ) ;
#43102 = DIRECTION ( 'NONE',  ( 0.3535533905932752297, -0.6123724356957952475, 0.7071067811865462405 ) ) ;
#43103 = CARTESIAN_POINT ( 'NONE',  ( -19.11315273645212898, -1.165603555308155626, 6.019083351294370665 ) ) ;
#43104 = VERTEX_POINT ( 'NONE', #39478 ) ;
#43105 = DIRECTION ( 'NONE',  ( -0.9999697198139514409, -0.000000000000000000, -0.007781995580013368816 ) ) ;
#43106 = ORIENTED_EDGE ( 'NONE', *, *, #49035, .T. ) ;
#43107 = DIRECTION ( 'NONE',  ( 0.005002170337468016433, -0.7660444431189770143, -0.6427681459581293666 ) ) ;
#43108 = DIRECTION ( 'NONE',  ( -0.3620778797217455991, 0.000000000000000000, -0.9321478471874540261 ) ) ;
#43109 = ADVANCED_FACE ( 'NONE', ( #5659 ), #22145, .F. ) ;
#43110 = CARTESIAN_POINT ( 'NONE',  ( -20.63393600974853470, -1.327505506330657781, 4.853888218877987271 ) ) ;
#43111 = LINE ( 'NONE', #25786, #7828 ) ;
#43112 = CARTESIAN_POINT ( 'NONE',  ( -16.65536346919183686, 5.143464774974010112, 11.79213186596540730 ) ) ;
#43113 = EDGE_CURVE ( 'NONE', #8976, #41711, #35231, .T. ) ;
#43114 = LINE ( 'NONE', #17845, #55871 ) ;
#43115 = VECTOR ( 'NONE', #2925, 1000.000000000000227 ) ;
#43116 = LINE ( 'NONE', #34033, #3830 ) ;
#43117 = APPLICATION_PROTOCOL_DEFINITION ( 'draft international standard', 'automotive_design', 1998, #26081 ) ;
#43118 = VECTOR ( 'NONE', #31353, 999.9999999999998863 ) ;
#43119 = ORIENTED_EDGE ( 'NONE', *, *, #15073, .F. ) ;
#43120 = CARTESIAN_POINT ( 'NONE',  ( -12.13851405436063047, 0.000000000000000000, 11.68505802764555135 ) ) ;
#43121 = CARTESIAN_POINT ( 'NONE',  ( -30.79411802867772607, 0.000000000000000000, 8.643412946479525516 ) ) ;
#43122 = DIRECTION ( 'NONE',  ( -0.9999697198139514409, -0.000000000000000000, -0.007781995580013368816 ) ) ;
#43123 = VECTOR ( 'NONE', #24311, 1000.000000000000114 ) ;
#43124 = EDGE_CURVE ( 'NONE', #5501, #48505, #48244, .T. ) ;
#43125 = CARTESIAN_POINT ( 'NONE',  ( -9.670752905330047611, 1.395709466279072997, 2.096644049295062651 ) ) ;
#43126 = AXIS2_PLACEMENT_3D ( 'NONE', #47069, #51609, #25771 ) ;
#43127 = CARTESIAN_POINT ( 'NONE',  ( -10.84028925556084388, -0.1191753592594197858, 11.14116300850493246 ) ) ;
#43128 = DIRECTION ( 'NONE',  ( -0.7660212471507179544, -0.6427876096865405842, -0.005961354470445141482 ) ) ;
#43129 = CARTESIAN_POINT ( 'NONE',  ( 2.072287782118878319, 0.000000000000000000, -2.950529333540147015 ) ) ;
#43130 = ORIENTED_EDGE ( 'NONE', *, *, #18204, .F. ) ;
#43131 = ADVANCED_FACE ( 'NONE', ( #40015 ), #35480, .T. ) ;
#43132 = DIRECTION ( 'NONE',  ( 0.005002170337468016433, -0.7660444431189770143, -0.6427681459581293666 ) ) ;
#43133 = VECTOR ( 'NONE', #27028, 999.9999999999998863 ) ;
#43134 = LINE ( 'NONE', #8482, #3316 ) ;
#43135 = VECTOR ( 'NONE', #32189, 999.9999999999998863 ) ;
#43136 = ORIENTED_EDGE ( 'NONE', *, *, #12047, .T. ) ;
#43137 = ORIENTED_EDGE ( 'NONE', *, *, #13046, .T. ) ;
#43138 = LINE ( 'NONE', #4776, #31042 ) ;
#43139 = AXIS2_PLACEMENT_3D ( 'NONE', #13834, #9294, #18372 ) ;
#43140 = ORIENTED_EDGE ( 'NONE', *, *, #39856, .F. ) ;
#43141 = AXIS2_PLACEMENT_3D ( 'NONE', #25595, #8282, #16816 ) ;
#43142 = VECTOR ( 'NONE', #13523, 1000.000000000000114 ) ;
#43143 = ORIENTED_EDGE ( 'NONE', *, *, #52415, .F. ) ;
#43144 = AXIS2_PLACEMENT_3D ( 'NONE', #48630, #44356, #18509 ) ;
#43145 = EDGE_LOOP ( 'NONE', ( #42228, #48335, #46403, #4404 ) ) ;
#43146 = ORIENTED_EDGE ( 'NONE', *, *, #49922, .T. ) ;
#43147 = CARTESIAN_POINT ( 'NONE',  ( -11.16083420050063957, 0.000000000000000000, 5.472215072723697560 ) ) ;
#43148 = EDGE_LOOP ( 'NONE', ( #29281, #5495, #14562, #12892 ) ) ;
#43149 = DIRECTION ( 'NONE',  ( -0.5449076811759708816, 0.6444004775717707689, 0.5364919789714475140 ) ) ;
#43150 = LINE ( 'NONE', #1066, #2201 ) ;
#43151 = EDGE_LOOP ( 'NONE', ( #647, #22331, #42410, #11543 ) ) ;
#43153 = ORIENTED_EDGE ( 'NONE', *, *, #36544, .F. ) ;
#43152 = ADVANCED_FACE ( 'NONE', ( #1102 ), #1400, .F. ) ;
#43154 = VECTOR ( 'NONE', #35568, 1000.000000000000227 ) ;
#43155 = ADVANCED_FACE ( 'NONE', ( #48551 ), #9938, .F. ) ;
#43156 = PLANE ( 'NONE',  #13042 ) ;
#43157 = VECTOR ( 'NONE', #6520, 999.9999999999998863 ) ;
#43159 = ADVANCED_FACE ( 'NONE', ( #32891 ), #55057, .F. ) ;
#43158 = ORIENTED_EDGE ( 'NONE', *, *, #50780, .T. ) ;
#43160 = DIRECTION ( 'NONE',  ( -0.9999697198139514409, -0.000000000000000000, -0.007781995580013368816 ) ) ;
#43161 = CARTESIAN_POINT ( 'NONE',  ( -19.12962290826653700, 0.000000000000000000, 14.40064212555863854 ) ) ;
#43162 = ORIENTED_EDGE ( 'NONE', *, *, #22220, .T. ) ;
#43163 = CIRCLE ( 'NONE', #18685, 1.000000000000000222 ) ;
#43164 = CARTESIAN_POINT ( 'NONE',  ( -13.27065584551087163, 0.000000000000000000, 12.04557950825129176 ) ) ;
#43165 = ADVANCED_FACE ( 'NONE', ( #23545 ), #11318, .F. ) ;
#43166 = EDGE_CURVE ( 'NONE', #37821, #55875, #50513, .T. ) ;
#43167 = EDGE_CURVE ( 'NONE', #16382, #38901, #32618, .T. ) ;
#43168 = ORIENTED_EDGE ( 'NONE', *, *, #42297, .F. ) ;
#43169 = FACE_OUTER_BOUND ( 'NONE', #7456, .T. ) ;
#43170 = VECTOR ( 'NONE', #31221, 1000.000000000000227 ) ;
#43171 = LINE ( 'NONE', #12769, #44508 ) ;
#43172 = VECTOR ( 'NONE', #10500, 1000.000000000000227 ) ;
#43173 = VECTOR ( 'NONE', #42717, 999.9999999999998863 ) ;
#43174 = ORIENTED_EDGE ( 'NONE', *, *, #14231, .T. ) ;
#43175 = CARTESIAN_POINT ( 'NONE',  ( -12.30315455128273783, 0.000000000000000000, 7.140659607065521719 ) ) ;
#43176 = DIRECTION ( 'NONE',  ( -0.9999697198139514409, -0.000000000000000000, -0.007781995580013368816 ) ) ;
#43177 = DIRECTION ( 'NONE',  ( 0.5449076811759707706, 0.6444004775717708799, -0.5364919789714476250 ) ) ;
#43178 = AXIS2_PLACEMENT_3D ( 'NONE', #16074, #16922, #21156 ) ;
#43179 = DIRECTION ( 'NONE',  ( -0.6427681459581293666, -0.7660444431189770143, -0.005002170337467561935 ) ) ;
#43180 = VERTEX_POINT ( 'NONE', #15307 ) ;
#43181 = VECTOR ( 'NONE', #27382, 1000.000000000000227 ) ;
#43182 = VECTOR ( 'NONE', #48459, 1000.000000000000227 ) ;
#43183 = CARTESIAN_POINT ( 'NONE',  ( -14.95364393125079694, -0.1166911823299087991, 2.590129555119498495 ) ) ;
#43184 = FACE_OUTER_BOUND ( 'NONE', #7095, .T. ) ;
#43185 = CARTESIAN_POINT ( 'NONE',  ( -12.33287787548504078, -3.594132820645661308, 7.371024595448199435 ) ) ;
#43186 = EDGE_CURVE ( 'NONE', #8862, #50596, #53917, .T. ) ;
#43187 = CARTESIAN_POINT ( 'NONE',  ( -14.86355910770291366, 0.000000000000000000, 3.596739262290799211 ) ) ;
#43188 = DIRECTION ( 'NONE',  ( 0.9999697198139515519, 0.000000000000000000, 0.007781995580013368816 ) ) ;
#43189 = CARTESIAN_POINT ( 'NONE',  ( 4.866417447938705898, 0.000000000000000000, -1.967953638240998337 ) ) ;
#43190 = LINE ( 'NONE', #44552, #22543 ) ;
#43191 = AXIS2_PLACEMENT_3D ( 'NONE', #48868, #23021, #49128 ) ;
#43192 = ADVANCED_FACE ( 'NONE', ( #23810 ), #15036, .F. ) ;
#43193 = AXIS2_PLACEMENT_3D ( 'NONE', #14425, #31733, #49037 ) ;
#43194 = DIRECTION ( 'NONE',  ( 0.7660212471507180654, -0.6427876096865404731, 0.005961354470445141482 ) ) ;
#43195 = CARTESIAN_POINT ( 'NONE',  ( -15.09097593232924872, 0.000000000000000000, 7.118964136457464065 ) ) ;
#43196 = VERTEX_POINT ( 'NONE', #37159 ) ;
#43197 = EDGE_CURVE ( 'NONE', #40269, #52695, #6786, .T. ) ;
#43198 = DIRECTION ( 'NONE',  ( -0.9999697198139514409, -0.000000000000000000, -0.007781995580013368816 ) ) ;
#43199 = ORIENTED_EDGE ( 'NONE', *, *, #48385, .T. ) ;
#43200 = PLANE ( 'NONE',  #51956 ) ;
#43201 = CARTESIAN_POINT ( 'NONE',  ( -17.74404816805336793, 0.000000000000000000, 3.574322630375089460 ) ) ;
#43202 = ADVANCED_FACE ( 'NONE', ( #7081 ), #41959, .F. ) ;
#43203 = ADVANCED_FACE ( 'NONE', ( #45971 ), #50772, .F. ) ;
#43204 = DIRECTION ( 'NONE',  ( -0.000000000000000000, -0.000000000000000000, -1.000000000000000000 ) ) ;
#43205 = DIRECTION ( 'NONE',  ( -0.9321478471874540261, 0.000000000000000000, 0.3620778797217457656 ) ) ;
#43206 = DIRECTION ( 'NONE',  ( -0.005002170337468016433, -0.7660444431189770143, 0.6427681459581293666 ) ) ;
#43207 = VECTOR ( 'NONE', #31104, 1000.000000000000000 ) ;
#43208 = VERTEX_POINT ( 'NONE', #11026 ) ;
#43209 = ORIENTED_EDGE ( 'NONE', *, *, #43166, .F. ) ;
#43210 = FACE_OUTER_BOUND ( 'NONE', #19416, .T. ) ;
#43211 = FACE_OUTER_BOUND ( 'NONE', #20965, .T. ) ;
#43212 = ORIENTED_EDGE ( 'NONE', *, *, #9168, .F. ) ;
#43213 = VECTOR ( 'NONE', #9434, 1000.000000000000227 ) ;
#43214 = DIRECTION ( 'NONE',  ( 0.000000000000000000, -1.000000000000000000, 0.000000000000000000 ) ) ;
#43215 = EDGE_LOOP ( 'NONE', ( #11748, #37970, #30841, #44140 ) ) ;
#43216 = DIRECTION ( 'NONE',  ( -0.005002170337468016433, -0.7660444431189770143, 0.6427681459581293666 ) ) ;
#43217 = VECTOR ( 'NONE', #53867, 1000.000000000000227 ) ;
#43218 = EDGE_LOOP ( 'NONE', ( #37839, #38988, #1612, #9192 ) ) ;
#43219 = DIRECTION ( 'NONE',  ( 0.6427681459581294776, -0.7660444431189769032, 0.005002170337467562802 ) ) ;
#43220 = VECTOR ( 'NONE', #24638, 1000.000000000000227 ) ;
#43221 = ORIENTED_EDGE ( 'NONE', *, *, #32052, .T. ) ;
#43222 = ORIENTED_EDGE ( 'NONE', *, *, #32733, .T. ) ;
#43223 = ORIENTED_EDGE ( 'NONE', *, *, #56176, .T. ) ;
#43224 = CARTESIAN_POINT ( 'NONE',  ( -58.00000000000000711, -9.000000000000000000, 2.750000000000008438 ) ) ;
#43225 = DIRECTION ( 'NONE',  ( -0.005961354470445682716, -0.6427876096865404731, 0.7660212471507180654 ) ) ;
#43226 = FACE_OUTER_BOUND ( 'NONE', #7939, .T. ) ;
#43227 = VECTOR ( 'NONE', #27535, 1000.000000000000114 ) ;
#43228 = VECTOR ( 'NONE', #21723, 1000.000000000000000 ) ;
#43229 = PLANE ( 'NONE',  #17609 ) ;
#43230 = ORIENTED_EDGE ( 'NONE', *, *, #47449, .F. ) ;
#43231 = ORIENTED_EDGE ( 'NONE', *, *, #25850, .F. ) ;
#43232 = VECTOR ( 'NONE', #41103, 999.9999999999998863 ) ;
#43233 = AXIS2_PLACEMENT_3D ( 'NONE', #25640, #26475, #38994 ) ;
#43234 = ORIENTED_EDGE ( 'NONE', *, *, #38441, .F. ) ;
#43235 = EDGE_CURVE ( 'NONE', #48860, #29778, #24375, .T. ) ;
#43236 = LINE ( 'NONE', #46921, #14957 ) ;
#43237 = VERTEX_POINT ( 'NONE', #6241 ) ;
#43238 = CARTESIAN_POINT ( 'NONE',  ( -16.81190032086591302, 0.000000000000000000, 3.212244750653343583 ) ) ;
#43239 = ORIENTED_EDGE ( 'NONE', *, *, #24447, .T. ) ;
#43240 = FACE_OUTER_BOUND ( 'NONE', #27909, .T. ) ;
#43241 = CARTESIAN_POINT ( 'NONE',  ( -16.03593764792711340, 0.000000000000000000, 9.127596588505243247 ) ) ;
#43242 = EDGE_CURVE ( 'NONE', #18181, #1604, #10774, .T. ) ;
#43243 = EDGE_CURVE ( 'NONE', #45359, #38901, #24109, .T. ) ;
#43244 = EDGE_LOOP ( 'NONE', ( #40162, #13864, #22125, #49302, #28994 ) ) ;
#43245 = LINE ( 'NONE', #4039, #12272 ) ;
#43246 = ORIENTED_EDGE ( 'NONE', *, *, #54517, .T. ) ;
#43247 = EDGE_CURVE ( 'NONE', #20652, #37968, #19270, .T. ) ;
#43248 = VECTOR ( 'NONE', #42082, 999.9999999999998863 ) ;
#43249 = DIRECTION ( 'NONE',  ( -0.6427681459581293666, -0.7660444431189770143, -0.005002170337467561935 ) ) ;
#43250 = ORIENTED_EDGE ( 'NONE', *, *, #30905, .F. ) ;
#43251 = LINE ( 'NONE', #12295, #51313 ) ;
#43252 = CARTESIAN_POINT ( 'NONE',  ( -17.16054654051782080, 0.2864062442990030766, 3.338532923747152381 ) ) ;
#43253 = DIRECTION ( 'NONE',  ( 0.9999697198139515519, 0.000000000000000000, 0.007781995580013368816 ) ) ;
#43254 = VERTEX_POINT ( 'NONE', #6501 ) ;
#43255 = LINE ( 'NONE', #24097, #33836 ) ;
#43256 = DIRECTION ( 'NONE',  ( -0.005002170337468016433, -0.7660444431189770143, 0.6427681459581293666 ) ) ;
#43257 = VECTOR ( 'NONE', #54934, 999.9999999999998863 ) ;
#43258 = PLANE ( 'NONE',  #47571 ) ;
#43259 = LINE ( 'NONE', #38715, #3175 ) ;
#43260 = PLANE ( 'NONE',  #8553 ) ;
#43262 = ADVANCED_FACE ( 'NONE', ( #36907 ), #54209, .F. ) ;
#43261 = CARTESIAN_POINT ( 'NONE',  ( -17.74482636761137044, -0.1191753592594197858, 3.674319602356483916 ) ) ;
#43263 = VECTOR ( 'NONE', #10359, 999.9999999999998863 ) ;
#43264 = LINE ( 'NONE', #9738, #27689 ) ;
#43265 = ORIENTED_EDGE ( 'NONE', *, *, #38943, .F. ) ;
#43266 = DIRECTION ( 'NONE',  ( 0.000000000000000000, -1.000000000000000000, 0.000000000000000000 ) ) ;
#43267 = DIRECTION ( 'NONE',  ( -0.005961354470445682716, -0.6427876096865404731, 0.7660212471507180654 ) ) ;
#43268 = ADVANCED_FACE ( 'NONE', ( #2770 ), #20095, .F. ) ;
#43269 = DIRECTION ( 'NONE',  ( 0.005961354470445682716, -0.6427876096865404731, -0.7660212471507180654 ) ) ;
#43270 = VERTEX_POINT ( 'NONE', #38857 ) ;
#43271 = DIRECTION ( 'NONE',  ( 0.000000000000000000, 0.000000000000000000, 1.000000000000000000 ) ) ;
#43272 = DIRECTION ( 'NONE',  ( 0.005002170337468016433, -0.7660444431189770143, -0.6427681459581293666 ) ) ;
#43273 = ORIENTED_EDGE ( 'NONE', *, *, #30032, .T. ) ;
#43274 = FACE_OUTER_BOUND ( 'NONE', #29380, .T. ) ;
#43275 = ADVANCED_FACE ( 'NONE', ( #17252 ), #42268, .F. ) ;
#43276 = VECTOR ( 'NONE', #36060, 999.9999999999998863 ) ;
#43277 = DIRECTION ( 'NONE',  ( 0.7660212471507180654, -0.6427876096865404731, 0.005961354470445141482 ) ) ;
#43278 = CARTESIAN_POINT ( 'NONE',  ( -16.81190032086591302, 0.000000000000000000, 3.212244750653343583 ) ) ;
#43279 = EDGE_CURVE ( 'NONE', #35486, #36692, #12154, .T. ) ;
#43280 = CARTESIAN_POINT ( 'NONE',  ( -65.41140007701454806, 2.000000000000004441, 1.620203490765837362 ) ) ;
#43281 = ORIENTED_EDGE ( 'NONE', *, *, #11607, .F. ) ;
#43282 = AXIS2_PLACEMENT_3D ( 'NONE', #38350, #43722, #30118 ) ;
#43283 = VERTEX_POINT ( 'NONE', #51622 ) ;
#43284 = FACE_OUTER_BOUND ( 'NONE', #11749, .T. ) ;
#43285 = DIRECTION ( 'NONE',  ( 0.5364919789714477361, 0.6444004775717706579, 0.5449076811759711036 ) ) ;
#43286 = LINE ( 'NONE', #26221, #47752 ) ;
#43287 = PLANE ( 'NONE',  #31157 ) ;
#43288 = DIRECTION ( 'NONE',  ( -0.2426528472758542054, 0.7422098413412800966, -0.6246952433987894571 ) ) ;
#43289 = PLANE ( 'NONE',  #39449 ) ;
#43290 = ORIENTED_EDGE ( 'NONE', *, *, #38667, .F. ) ;
#43291 = PLANE ( 'NONE',  #41919 ) ;
#43292 = DIRECTION ( 'NONE',  ( 0.007781995580012663651, -3.146120232559066537E-19, -0.9999697198139514409 ) ) ;
#43293 = ORIENTED_EDGE ( 'NONE', *, *, #15966, .F. ) ;
#43294 = PLANE ( 'NONE',  #29256 ) ;
#43295 = DIRECTION ( 'NONE',  ( 0.000000000000000000, -1.000000000000000000, 0.000000000000000000 ) ) ;
#43296 = DIRECTION ( 'NONE',  ( -0.005961354470445682716, -0.6427876096865404731, 0.7660212471507180654 ) ) ;
#43297 = ORIENTED_EDGE ( 'NONE', *, *, #49047, .F. ) ;
#43298 = DIRECTION ( 'NONE',  ( 0.000000000000000000, -0.000000000000000000, -1.000000000000000000 ) ) ;
#43299 = ORIENTED_EDGE ( 'NONE', *, *, #14087, .T. ) ;
#43300 = VERTEX_POINT ( 'NONE', #3913 ) ;
#43301 = VECTOR ( 'NONE', #50982, 1000.000000000000114 ) ;
#43302 = ORIENTED_EDGE ( 'NONE', *, *, #43420, .F. ) ;
#43303 = VERTEX_POINT ( 'NONE', #34574 ) ;
#43304 = CARTESIAN_POINT ( 'NONE',  ( -18.56571281152978514, 4.172053068839010947, 3.760374745758259252 ) ) ;
#43305 = ORIENTED_EDGE ( 'NONE', *, *, #24550, .T. ) ;
#43306 = CARTESIAN_POINT ( 'NONE',  ( -12.97073463163625817, 23.43756790714967764, -3.644115791447929631 ) ) ;
#43307 = EDGE_CURVE ( 'NONE', #13391, #48888, #39118, .T. ) ;
#43308 = AXIS2_PLACEMENT_3D ( 'NONE', #32291, #36829, #20309 ) ;
#43309 = ORIENTED_EDGE ( 'NONE', *, *, #37190, .F. ) ;
#43310 = CARTESIAN_POINT ( 'NONE',  ( -14.87218126821876218, 0.000000000000000000, 4.704668372064093163 ) ) ;
#43311 = VERTEX_POINT ( 'NONE', #51889 ) ;
#43312 = DIRECTION ( 'NONE',  ( 0.007781995580012662783, 0.000000000000000000, -0.9999697198139514409 ) ) ;
#43313 = ORIENTED_EDGE ( 'NONE', *, *, #11519, .F. ) ;
#43314 = EDGE_CURVE ( 'NONE', #33246, #17026, #13006, .T. ) ;
#43315 = EDGE_CURVE ( 'NONE', #48572, #47834, #17000, .T. ) ;
#43316 = DIRECTION ( 'NONE',  ( -0.9999697198139514409, -0.000000000000000000, -0.007781995580013368816 ) ) ;
#43317 = DIRECTION ( 'NONE',  ( 0.007781995580012662783, 0.000000000000000000, -0.9999697198139514409 ) ) ;
#43318 = CARTESIAN_POINT ( 'NONE',  ( -22.40478740399063895, 0.000000000000000000, 5.384712028983816623 ) ) ;
#43319 = DIRECTION ( 'NONE',  ( 0.6427681459581294776, -0.7660444431189769032, 0.005002170337467562802 ) ) ;
#43320 = DIRECTION ( 'NONE',  ( 0.6427681459581294776, -0.7660444431189769032, 0.005002170337467562802 ) ) ;
#43321 = VERTEX_POINT ( 'NONE', #26088 ) ;
#43322 = ORIENTED_EDGE ( 'NONE', *, *, #49776, .F. ) ;
#43323 = CARTESIAN_POINT ( 'NONE',  ( -17.42853068406109784, 0.000000000000000000, 8.947433093906241197 ) ) ;
#43324 = CARTESIAN_POINT ( 'NONE',  ( -19.32961685222932147, 0.000000000000000000, 14.39908572644263351 ) ) ;
#43325 = DIRECTION ( 'NONE',  ( 0.9335804264972047406, -0.3583679495452924968, 0.000000000000000000 ) ) ;
#43326 = DIRECTION ( 'NONE',  ( 0.9999697198139515519, 0.000000000000000000, 0.007781995580013368816 ) ) ;
#43327 = LINE ( 'NONE', #4421, #5900 ) ;
#43328 = CARTESIAN_POINT ( 'NONE',  ( -1.602641424070903486, 5.553834702102301790, 3.840893930704793569 ) ) ;
#43329 = VERTEX_POINT ( 'NONE', #46499 ) ;
#43330 = LINE ( 'NONE', #4424, #27477 ) ;
#43331 = DIRECTION ( 'NONE',  ( 0.9999697198139515519, 0.000000000000000000, 0.007781995580013368816 ) ) ;
#43332 = ORIENTED_EDGE ( 'NONE', *, *, #51854, .F. ) ;
#43333 = CARTESIAN_POINT ( 'NONE',  ( -25.20123094555300369, 0.000000000000000000, 6.470945668149052032 ) ) ;
#43334 = LINE ( 'NONE', #5272, #44186 ) ;
#43335 = CARTESIAN_POINT ( 'NONE',  ( -22.36868959911851462, 19.74370688441071309, 4.433756599430258127 ) ) ;
#43336 = EDGE_CURVE ( 'NONE', #8803, #42565, #30045, .T. ) ;
#43337 = PLANE ( 'NONE',  #8789 ) ;
#43338 = AXIS2_PLACEMENT_3D ( 'NONE', #50658, #46669, #11752 ) ;
#43339 = ORIENTED_EDGE ( 'NONE', *, *, #13986, .F. ) ;
#43340 = EDGE_CURVE ( 'NONE', #31630, #40301, #3373, .T. ) ;
#43341 = VERTEX_POINT ( 'NONE', #34031 ) ;
#43342 = CARTESIAN_POINT ( 'NONE',  ( -10.66901316772273489, 0.000000000000000000, 1.982727895876851942 ) ) ;
#43343 = DIRECTION ( 'NONE',  ( 0.007781995580012662783, 0.000000000000000000, -0.9999697198139514409 ) ) ;
#43344 = FACE_OUTER_BOUND ( 'NONE', #36897, .T. ) ;
#43345 = VECTOR ( 'NONE', #21920, 999.9999999999998863 ) ;
#43346 = CARTESIAN_POINT ( 'NONE',  ( -22.03063137938938354, 19.66613178766788295, -4.421226477812651545 ) ) ;
#43347 = ADVANCED_FACE ( 'NONE', ( #20944 ), #51045, .F. ) ;
#43348 = CARTESIAN_POINT ( 'NONE',  ( -15.35406248609154112, 0.000000000000000000, 6.916910679842669829 ) ) ;
#43349 = CARTESIAN_POINT ( 'NONE',  ( 1.971453974394196562, 0.000000000000000000, 10.00639841352631088 ) ) ;
#43350 = CARTESIAN_POINT ( 'NONE',  ( -15.40103151951671734, 0.000000000000000000, 12.95233060667165681 ) ) ;
#43351 = VERTEX_POINT ( 'NONE', #47651 ) ;
#43352 = CARTESIAN_POINT ( 'NONE',  ( -10.47421230394850866, 0.000000000000000000, 10.95934586908605723 ) ) ;
#43353 = DIRECTION ( 'NONE',  ( 0.005961354470445682716, -0.6427876096865404731, -0.7660212471507180654 ) ) ;
#43354 = ORIENTED_EDGE ( 'NONE', *, *, #9761, .T. ) ;
#43355 = DIRECTION ( 'NONE',  ( 0.9999697198139515519, 0.000000000000000000, 0.007781995580013368816 ) ) ;
#43356 = ORIENTED_EDGE ( 'NONE', *, *, #10474, .T. ) ;
#43357 = DIRECTION ( 'NONE',  ( -0.5364919789714478471, 0.6444004775717705469, -0.5449076811759709926 ) ) ;
#43358 = EDGE_LOOP ( 'NONE', ( #13598, #43239, #16088, #8574 ) ) ;
#43359 = ORIENTED_EDGE ( 'NONE', *, *, #44643, .F. ) ;
#43360 = EDGE_LOOP ( 'NONE', ( #32611, #2986, #24453, #41038 ) ) ;
#43361 = ORIENTED_EDGE ( 'NONE', *, *, #51998, .F. ) ;
#43362 = ORIENTED_EDGE ( 'NONE', *, *, #322, .F. ) ;
#43363 = ORIENTED_EDGE ( 'NONE', *, *, #6770, .F. ) ;
#43364 = LINE ( 'NONE', #3872, #32238 ) ;
#43365 = DIRECTION ( 'NONE',  ( 0.007781995580012663651, -3.146120232559066537E-19, -0.9999697198139514409 ) ) ;
#43366 = EDGE_CURVE ( 'NONE', #41874, #20696, #12466, .T. ) ;
#43367 = LINE ( 'NONE', #39088, #34906 ) ;
#43368 = EDGE_LOOP ( 'NONE', ( #7458, #11224, #48085, #15647 ) ) ;
#43369 = DIRECTION ( 'NONE',  ( -0.5449076811759708816, 0.6444004775717707689, 0.5364919789714475140 ) ) ;
#43370 = ORIENTED_EDGE ( 'NONE', *, *, #29719, .T. ) ;
#43371 = ORIENTED_EDGE ( 'NONE', *, *, #15376, .T. ) ;
#43372 = ADVANCED_FACE ( 'NONE', ( #29784 ), #8771, .F. ) ;
#43373 = FACE_OUTER_BOUND ( 'NONE', #19756, .T. ) ;
#43374 = CARTESIAN_POINT ( 'NONE',  ( -15.32464057242408195, 5.305366725996512933, 2.465273581601329145 ) ) ;
#43375 = VERTEX_POINT ( 'NONE', #4491 ) ;
#43376 = DIRECTION ( 'NONE',  ( 0.007781995580012663651, -3.146120232559066537E-19, -0.9999697198139514409 ) ) ;
#43377 = ORIENTED_EDGE ( 'NONE', *, *, #36382, .F. ) ;
#43378 = AXIS2_PLACEMENT_3D ( 'NONE', #51680, #3984, #12783 ) ;
#43379 = FACE_OUTER_BOUND ( 'NONE', #30786, .T. ) ;
#43380 = LINE ( 'NONE', #12707, #12132 ) ;
#43381 = EDGE_CURVE ( 'NONE', #8547, #35585, #21799, .T. ) ;
#43382 = PLANE ( 'NONE',  #41432 ) ;
#43383 = FACE_OUTER_BOUND ( 'NONE', #49777, .T. ) ;
#43384 = CARTESIAN_POINT ( 'NONE',  ( -18.71879214953967008, -0.1191753592594166911, 8.468056882921050743 ) ) ;
#43385 = CARTESIAN_POINT ( 'NONE',  ( 5.617911074533876281, -1.049994927612889040, -2.260412882205727669 ) ) ;
#43386 = FACE_OUTER_BOUND ( 'NONE', #29481, .T. ) ;
#43387 = CARTESIAN_POINT ( 'NONE',  ( -69.34563465300942653, -11.65986150400551580, 7.856885134693455619 ) ) ;
#43388 = EDGE_LOOP ( 'NONE', ( #32100, #41075, #17958, #46762 ) ) ;
#43389 = CARTESIAN_POINT ( 'NONE',  ( -55.85443948382626900, 6.788488266608555755, -1.722920386167723583 ) ) ;
#43390 = DIRECTION ( 'NONE',  ( 0.9999697198139515519, 0.000000000000000000, 0.007781995580013368816 ) ) ;
#43391 = DIRECTION ( 'NONE',  ( -0.005961354470445682716, -0.6427876096865404731, 0.7660212471507180654 ) ) ;
#43392 = CARTESIAN_POINT ( 'NONE',  ( -17.87879731337576317, 0.000000000000000000, 7.097268665849407299 ) ) ;
#43393 = CARTESIAN_POINT ( 'NONE',  ( -24.40242990923838562, 16.83747556133229395, -4.580958211367532229 ) ) ;
#43394 = CARTESIAN_POINT ( 'NONE',  ( -17.64908100030126548, -3.270328918600660995, 8.904601060243949817 ) ) ;
#43395 = LINE ( 'NONE', #783, #18705 ) ;
#43396 = CARTESIAN_POINT ( 'NONE',  ( -9.042074112879289416, 0.000000000000000000, 6.058041879668295771 ) ) ;
#43397 = VERTEX_POINT ( 'NONE', #24945 ) ;
#43398 = LINE ( 'NONE', #34321, #50169 ) ;
#43399 = PLANE ( 'NONE',  #42124 ) ;
#43400 = PLANE ( 'NONE',  #25469 ) ;
#43401 = LINE ( 'NONE', #9302, #24585 ) ;
#43402 = EDGE_CURVE ( 'NONE', #38162, #27809, #11862, .T. ) ;
#43403 = DIRECTION ( 'NONE',  ( 0.005961354470445682716, -0.6427876096865404731, -0.7660212471507180654 ) ) ;
#43404 = CARTESIAN_POINT ( 'NONE',  ( -16.32868032335150232, 2.067327705546508021, 2.958587115942813206 ) ) ;
#43405 = CARTESIAN_POINT ( 'NONE',  ( -15.83583329205734103, -2.784623065533159636, 7.403148020359251014 ) ) ;
#43406 = LINE ( 'NONE', #30645, #13102 ) ;
#43407 = CARTESIAN_POINT ( 'NONE',  ( -15.35118843258626065, 0.000000000000000000, 6.547600976584903698 ) ) ;
#43408 = ORIENTED_EDGE ( 'NONE', *, *, #54402, .F. ) ;
#43409 = CARTESIAN_POINT ( 'NONE',  ( -28.93137873341882127, 0.000000000000000000, 8.119251130998824451 ) ) ;
#43410 = ADVANCED_FACE ( 'NONE', ( #8187 ), #38007, .F. ) ;
#43411 = AXIS2_PLACEMENT_3D ( 'NONE', #44355, #22769, #44618 ) ;
#43412 = ORIENTED_EDGE ( 'NONE', *, *, #5992, .T. ) ;
#43413 = EDGE_CURVE ( 'NONE', #46599, #3531, #55897, .T. ) ;
#43414 = ADVANCED_FACE ( 'NONE', ( #21543 ), #1043, .F. ) ;
#43415 = ORIENTED_EDGE ( 'NONE', *, *, #41719, .T. ) ;
#43416 = ORIENTED_EDGE ( 'NONE', *, *, #32701, .F. ) ;
#43417 = ORIENTED_EDGE ( 'NONE', *, *, #15465, .T. ) ;
#43418 = ORIENTED_EDGE ( 'NONE', *, *, #54418, .T. ) ;
#43419 = CARTESIAN_POINT ( 'NONE',  ( -17.21261007345589178, 0.000000000000000000, 6.902447032770631097 ) ) ;
#43420 = EDGE_CURVE ( 'NONE', #14352, #49950, #48186, .T. ) ;
#43421 = PLANE ( 'NONE',  #26702 ) ;
#43422 = ADVANCED_FACE ( 'NONE', ( #36019 ), #44239, .F. ) ;
#43423 = ORIENTED_EDGE ( 'NONE', *, *, #9046, .T. ) ;
#43424 = ADVANCED_FACE ( 'NONE', ( #18955 ), #30877, .F. ) ;
#43425 = CARTESIAN_POINT ( 'NONE',  ( 2.072287782118878319, 0.000000000000000000, -2.950529333540147015 ) ) ;
#43426 = VERTEX_POINT ( 'NONE', #31732 ) ;
#43427 = DIRECTION ( 'NONE',  ( 0.005961354470445682716, -0.6427876096865404731, -0.7660212471507180654 ) ) ;
#43428 = LINE ( 'NONE', #29820, #17768 ) ;
#43429 = VERTEX_POINT ( 'NONE', #43935 ) ;
#43430 = DIRECTION ( 'NONE',  ( -0.6427681459581293666, -0.7660444431189770143, -0.005002170337467561935 ) ) ;
#43431 = EDGE_CURVE ( 'NONE', #45114, #6152, #27457, .T. ) ;
#43432 = ORIENTED_EDGE ( 'NONE', *, *, #41368, .T. ) ;
#43433 = DIRECTION ( 'NONE',  ( -0.5364919789714478471, 0.6444004775717705469, -0.5449076811759709926 ) ) ;
#43434 = ADVANCED_FACE ( 'NONE', ( #14423 ), #1333, .F. ) ;
#43435 = LINE ( 'NONE', #247, #31830 ) ;
#43436 = EDGE_LOOP ( 'NONE', ( #28451, #40274, #26797, #25136 ) ) ;
#43437 = DIRECTION ( 'NONE',  ( 0.6427681459581294776, -0.7660444431189769032, 0.005002170337467562802 ) ) ;
#43438 = CARTESIAN_POINT ( 'NONE',  ( -19.45503627000849889, 0.000000000000000000, 7.556996783084074742 ) ) ;
#43439 = CARTESIAN_POINT ( 'NONE',  ( -19.60834386242827776, 0.000000000000000000, 4.298478389818581213 ) ) ;
#43440 = CARTESIAN_POINT ( 'NONE',  ( -12.74036856746027802, 0.000000000000000000, 3.613262422014844155 ) ) ;
#43441 = VERTEX_POINT ( 'NONE', #53027 ) ;
#43442 = VECTOR ( 'NONE', #55118, 1000.000000000000114 ) ;
#43443 = CARTESIAN_POINT ( 'NONE',  ( -69.93390552824286033, -0.8671508776962656428, -7.500305896622813329 ) ) ;
#43444 = CARTESIAN_POINT ( 'NONE',  ( -23.33693525117809386, 0.000000000000000000, 5.746789908705562944 ) ) ;
#43445 = LINE ( 'NONE', #42872, #32174 ) ;
#43446 = CARTESIAN_POINT ( 'NONE',  ( -11.20636620717317378, 0.000000000000000000, 11.32298014792380414 ) ) ;
#43447 = CYLINDRICAL_SURFACE ( 'NONE', #37733, 0.5000000000000004441 ) ;
#43448 = LINE ( 'NONE', #13070, #36727 ) ;
#43449 = CARTESIAN_POINT ( 'NONE',  ( -20.72814514249575168, 20.40220053346460460, -4.657437592157546824 ) ) ;
#43450 = PLANE ( 'NONE',  #41971 ) ;
#43451 = DIRECTION ( 'NONE',  ( -0.9999697198139514409, -0.000000000000000000, -0.007781995580013368816 ) ) ;
#43452 = FACE_OUTER_BOUND ( 'NONE', #21898, .T. ) ;
#43453 = ORIENTED_EDGE ( 'NONE', *, *, #33931, .T. ) ;
#43454 = PLANE ( 'NONE',  #17513 ) ;
#43455 = LINE ( 'NONE', #9370, #935 ) ;
#43456 = DIRECTION ( 'NONE',  ( 0.005961354470445682716, -0.6427876096865404731, -0.7660212471507180654 ) ) ;
#43457 = LINE ( 'NONE', #48565, #1917 ) ;
#43458 = ADVANCED_FACE ( 'NONE', ( #781 ), #22082, .F. ) ;
#43459 = DIRECTION ( 'NONE',  ( 0.000000000000000000, -0.000000000000000000, -1.000000000000000000 ) ) ;
#43460 = PLANE ( 'NONE',  #8412 ) ;
#43461 = ORIENTED_EDGE ( 'NONE', *, *, #27381, .F. ) ;
#43462 = EDGE_LOOP ( 'NONE', ( #24001, #4581, #37578, #6259 ) ) ;
#43463 = CARTESIAN_POINT ( 'NONE',  ( -12.20933787556949213, -1.813211359398156919, 4.400241940589850742 ) ) ;
#43464 = DIRECTION ( 'NONE',  ( 0.7660212471507180654, -0.6427876096865404731, 0.005961354470445141482 ) ) ;
#43465 = EDGE_LOOP ( 'NONE', ( #42655, #30512, #30070, #38533 ) ) ;
#43466 = EDGE_CURVE ( 'NONE', #25808, #46628, #44783, .T. ) ;
#43467 = ADVANCED_FACE ( 'NONE', ( #4760 ), #18676, .F. ) ;
#43468 = DIRECTION ( 'NONE',  ( 0.5364919789714477361, 0.6444004775717706579, 0.5449076811759711036 ) ) ;
#43469 = VERTEX_POINT ( 'NONE', #5896 ) ;
#43470 = CARTESIAN_POINT ( 'NONE',  ( -17.46532115785441519, 0.000000000000000000, 13.67492996699914265 ) ) ;
#43471 = EDGE_LOOP ( 'NONE', ( #15894, #24557, #53816, #3539 ) ) ;
#43472 = DIRECTION ( 'NONE',  ( 0.9999697198139515519, 0.000000000000000000, 0.007781995580013368816 ) ) ;
#43473 = EDGE_CURVE ( 'NONE', #36189, #10560, #31159, .T. ) ;
#43474 = EDGE_LOOP ( 'NONE', ( #17169, #13701, #46631, #49844 ) ) ;
#43475 = ORIENTED_EDGE ( 'NONE', *, *, #34340, .F. ) ;
#43476 = ORIENTED_EDGE ( 'NONE', *, *, #41233, .F. ) ;
#43477 = LINE ( 'NONE', #12814, #41097 ) ;
#43478 = DIRECTION ( 'NONE',  ( -0.7660212471507179544, -0.6427876096865405842, -0.005961354470445141482 ) ) ;
#43479 = DIRECTION ( 'NONE',  ( -0.6427681459581293666, -0.7660444431189770143, -0.005002170337467561935 ) ) ;
#43480 = FACE_OUTER_BOUND ( 'NONE', #53287, .T. ) ;
#43481 = EDGE_CURVE ( 'NONE', #44308, #39505, #27183, .T. ) ;
#43482 = ORIENTED_EDGE ( 'NONE', *, *, #37135, .F. ) ;
#43483 = VERTEX_POINT ( 'NONE', #23222 ) ;
#43484 = EDGE_CURVE ( 'NONE', #54767, #7497, #505, .T. ) ;
#43485 = EDGE_LOOP ( 'NONE', ( #34699, #26793, #21572, #49419 ) ) ;
#43486 = CARTESIAN_POINT ( 'NONE',  ( -67.27731269685068582, -9.409571107119717226, -7.454891809856700746 ) ) ;
#43487 = VERTEX_POINT ( 'NONE', #44489 ) ;
#43488 = CARTESIAN_POINT ( 'NONE',  ( 2.072287782118878319, 0.000000000000000000, -2.950529333540147015 ) ) ;
#43489 = EDGE_LOOP ( 'NONE', ( #17492, #51761, #35455, #47904 ) ) ;
#43490 = DIRECTION ( 'NONE',  ( -0.7660212471507179544, -0.6427876096865405842, -0.005961354470445141482 ) ) ;
#43491 = CARTESIAN_POINT ( 'NONE',  ( -18.23205287539565589, -0.6798977022406563764, 4.879708191131419071 ) ) ;
#43492 = EDGE_CURVE ( 'NONE', #34678, #45226, #5598, .T. ) ;
#43493 = ORIENTED_EDGE ( 'NONE', *, *, #19554, .F. ) ;
#43494 = CARTESIAN_POINT ( 'NONE',  ( -18.67619601524082285, 0.000000000000000000, 3.936400510096834893 ) ) ;
#43495 = EDGE_LOOP ( 'NONE', ( #7407, #52433, #36425, #5270 ) ) ;
#43496 = CARTESIAN_POINT ( 'NONE',  ( -17.19979620504548024, 0.000000000000000000, 5.255892460444599124 ) ) ;
#43497 = ORIENTED_EDGE ( 'NONE', *, *, #41715, .T. ) ;
#43498 = PLANE ( 'NONE',  #5111 ) ;
#43499 = FACE_OUTER_BOUND ( 'NONE', #36095, .T. ) ;
#43500 = CARTESIAN_POINT ( 'NONE',  ( -10.72382211176504008, -1.165603555308156736, 2.760382433798663993 ) ) ;
#43501 = EDGE_LOOP ( 'NONE', ( #12193, #52672, #32267 ) ) ;
#43502 = DIRECTION ( 'NONE',  ( 0.5449076811759707706, 0.6444004775717708799, -0.5364919789714476250 ) ) ;
#43503 = DIRECTION ( 'NONE',  ( -0.1139275668495183524, 0.9934890585767659488, 4.694855797473114533E-16 ) ) ;
#43504 = DIRECTION ( 'NONE',  ( 0.005961354470445682716, -0.6427876096865404731, -0.7660212471507180654 ) ) ;
#43505 = DIRECTION ( 'NONE',  ( 0.000000000000000000, -1.000000000000000000, 0.000000000000000000 ) ) ;
#43506 = DIRECTION ( 'NONE',  ( 0.000000000000000000, -0.000000000000000000, -1.000000000000000000 ) ) ;
#43507 = LINE ( 'NONE', #44352, #26113 ) ;
#43508 = DIRECTION ( 'NONE',  ( -0.005961354470445682716, -0.6427876096865404731, 0.7660212471507180654 ) ) ;
#43509 = ORIENTED_EDGE ( 'NONE', *, *, #29371, .T. ) ;
#43510 = DIRECTION ( 'NONE',  ( 0.000000000000000000, -0.000000000000000000, -1.000000000000000000 ) ) ;
#43511 = DIRECTION ( 'NONE',  ( 0.007781995580012663651, -3.146120232559066537E-19, -0.9999697198139514409 ) ) ;
#43512 = CARTESIAN_POINT ( 'NONE',  ( -16.26764835785802532, 0.000000000000000000, 4.893814580722853691 ) ) ;
#43513 = ORIENTED_EDGE ( 'NONE', *, *, #16953, .F. ) ;
#43514 = CARTESIAN_POINT ( 'NONE',  ( -15.60102546347950536, 0.000000000000000000, 12.95077420755565356 ) ) ;
#43515 = CARTESIAN_POINT ( 'NONE',  ( -16.53317331066696383, 0.000000000000000000, 13.31285208727739899 ) ) ;
#43516 = ORIENTED_EDGE ( 'NONE', *, *, #30015, .F. ) ;
#43517 = ADVANCED_FACE ( 'NONE', ( #40243 ), #52186, .F. ) ;
#43518 = DIRECTION ( 'NONE',  ( -0.5364919789714478471, 0.6444004775717705469, -0.5449076811759709926 ) ) ;
#43519 = DIRECTION ( 'NONE',  ( 0.007781995580012663651, 0.000000000000000000, -0.9999697198139515519 ) ) ;
#43520 = ADVANCED_FACE ( 'NONE', ( #17844 ), #35174, .F. ) ;
#43521 = LINE ( 'NONE', #8321, #16921 ) ;
#43522 = DIRECTION ( 'NONE',  ( 0.9999697198139515519, 0.000000000000000000, 0.007781995580013368816 ) ) ;
#43523 = EDGE_LOOP ( 'NONE', ( #11990, #50447, #17887, #28411, #29821 ) ) ;
#43524 = ORIENTED_EDGE ( 'NONE', *, *, #12901, .T. ) ;
#43525 = EDGE_CURVE ( 'NONE', #51710, #52991, #50443, .T. ) ;
#43526 = DIRECTION ( 'NONE',  ( 0.9999697198139515519, 0.000000000000000000, 0.007781995580013368816 ) ) ;
#43527 = FACE_OUTER_BOUND ( 'NONE', #18925, .T. ) ;
#43528 = DIRECTION ( 'NONE',  ( 0.9999697198139515519, 0.000000000000000000, 0.007781995580013368816 ) ) ;
#43529 = EDGE_CURVE ( 'NONE', #55216, #56100, #6188, .T. ) ;
#43530 = EDGE_CURVE ( 'NONE', #21707, #39029, #2463, .T. ) ;
#43531 = EDGE_CURVE ( 'NONE', #47622, #50731, #10726, .T. ) ;
#43532 = CARTESIAN_POINT ( 'NONE',  ( -21.12145515939264584, -2.460819163488159766, 5.007098573608039338 ) ) ;
#43533 = CARTESIAN_POINT ( 'NONE',  ( -14.92626657078307417, -2.298917212465660054, 2.605842456189420009 ) ) ;
#43534 = CARTESIAN_POINT ( 'NONE',  ( -24.26908309836554878, 0.000000000000000000, 6.108867788427308376 ) ) ;
#43536 = EDGE_CURVE ( 'NONE', #41476, #35980, #41628, .T. ) ;
#43535 = EDGE_LOOP ( 'NONE', ( #32528, #20520, #2819, #25826 ) ) ;
#43537 = LINE ( 'NONE', #21696, #12924 ) ;
#43538 = DIRECTION ( 'NONE',  ( 0.7660212471507180654, -0.6427876096865404731, 0.005961354470445141482 ) ) ;
#43539 = VERTEX_POINT ( 'NONE', #11253 ) ;
#43540 = DIRECTION ( 'NONE',  ( 0.005002170337468016433, -0.7660444431189770143, -0.6427681459581293666 ) ) ;
#43541 = LINE ( 'NONE', #14312, #53119 ) ;
#43542 = DIRECTION ( 'NONE',  ( 0.007781995580012663651, 0.000000000000000000, -0.9999697198139515519 ) ) ;
#43543 = ORIENTED_EDGE ( 'NONE', *, *, #41233, .T. ) ;
#43544 = LINE ( 'NONE', #47237, #36537 ) ;
#43545 = ADVANCED_FACE ( 'NONE', ( #24576 ), #37104, .F. ) ;
#43546 = VERTEX_POINT ( 'NONE', #6445 ) ;
#43547 = VECTOR ( 'NONE', #13564, 1000.000000000000227 ) ;
#43549 = ORIENTED_EDGE ( 'NONE', *, *, #24551, .F. ) ;
#43548 = ADVANCED_FACE ( 'NONE', ( #14968 ), #41372, .F. ) ;
#43550 = VERTEX_POINT ( 'NONE', #49323 ) ;
#43551 = EDGE_CURVE ( 'NONE', #39622, #13853, #5038, .T. ) ;
#43552 = ORIENTED_EDGE ( 'NONE', *, *, #20205, .T. ) ;
#43553 = LINE ( 'NONE', #13473, #4880 ) ;
#43554 = ORIENTED_EDGE ( 'NONE', *, *, #4103, .T. ) ;
#43555 = CARTESIAN_POINT ( 'NONE',  ( -11.64139776398414128, 0.000000000000000000, 7.515141621207298783 ) ) ;
#43556 = EDGE_CURVE ( 'NONE', #14263, #10825, #6721, .T. ) ;
#43557 = ORIENTED_EDGE ( 'NONE', *, *, #16928, .T. ) ;
#43558 = FACE_OUTER_BOUND ( 'NONE', #47509, .T. ) ;
#43559 = ORIENTED_EDGE ( 'NONE', *, *, #20347, .T. ) ;
#43560 = DIRECTION ( 'NONE',  ( -0.9999697198139514409, -0.000000000000000000, -0.007781995580013368816 ) ) ;
#43561 = VERTEX_POINT ( 'NONE', #24041 ) ;
#43562 = EDGE_CURVE ( 'NONE', #38932, #42767, #46166, .T. ) ;
#43563 = CARTESIAN_POINT ( 'NONE',  ( -14.88810793486117667, 0.000000000000000000, 6.751210832315702959 ) ) ;
#43564 = CARTESIAN_POINT ( 'NONE',  ( -15.49681410618518562, 3.848249166794011522, 2.578641308138473143 ) ) ;
#43565 = LINE ( 'NONE', #55797, #15877 ) ;
#43566 = DIRECTION ( 'NONE',  ( -0.005961354470445682716, -0.6427876096865404731, 0.7660212471507180654 ) ) ;
#43567 = DIRECTION ( 'NONE',  ( -0.5449076811759708816, 0.6444004775717707689, 0.5364919789714475140 ) ) ;
#43568 = ORIENTED_EDGE ( 'NONE', *, *, #48145, .T. ) ;
#43569 = ORIENTED_EDGE ( 'NONE', *, *, #40795, .T. ) ;
#43570 = DIRECTION ( 'NONE',  ( 0.007781995580012663651, 0.000000000000000000, -0.9999697198139515519 ) ) ;
#43571 = CARTESIAN_POINT ( 'NONE',  ( -16.46169322245890498, -5.698858183938163791, 12.42900958272824852 ) ) ;
#43572 = CARTESIAN_POINT ( 'NONE',  ( -12.08879033979353324, 0.000000000000000000, 5.295667489892703195 ) ) ;
#43573 = DIRECTION ( 'NONE',  ( 0.000000000000000000, -1.000000000000000000, 0.000000000000000000 ) ) ;
#43574 = DIRECTION ( 'NONE',  ( -0.9999697198139514409, -0.000000000000000000, -0.007781995580013368816 ) ) ;
#43575 = CARTESIAN_POINT ( 'NONE',  ( -26.13415699229845757, -0.1191753592594197858, 6.933020519852192365 ) ) ;
#43576 = ORIENTED_EDGE ( 'NONE', *, *, #31038, .T. ) ;
#43577 = CARTESIAN_POINT ( 'NONE',  ( -18.14475792064334314, 0.000000000000000000, 7.264524912492376529 ) ) ;
#43578 = LINE ( 'NONE', #8382, #32220 ) ;
#43579 = ORIENTED_EDGE ( 'NONE', *, *, #49848, .T. ) ;
#43580 = DIRECTION ( 'NONE',  ( 0.007781995580012663651, 0.000000000000000000, -0.9999697198139515519 ) ) ;
#43581 = DIRECTION ( 'NONE',  ( 0.000000000000000000, -0.000000000000000000, -1.000000000000000000 ) ) ;
#43582 = DIRECTION ( 'NONE',  ( 0.007781995580012663651, 0.000000000000000000, -0.9999697198139515519 ) ) ;
#43583 = PLANE ( 'NONE',  #15096 ) ;
#43584 = AXIS2_PLACEMENT_3D ( 'NONE', #38346, #55380, #46889 ) ;
#43585 = LINE ( 'NONE', #50775, #26529 ) ;
#43586 = ORIENTED_EDGE ( 'NONE', *, *, #24767, .T. ) ;
#43587 = ORIENTED_EDGE ( 'NONE', *, *, #49689, .T. ) ;
#43588 = CARTESIAN_POINT ( 'NONE',  ( -15.99989958031287962, 5.467268677019012202, 12.06894479977838408 ) ) ;
#43589 = FACE_OUTER_BOUND ( 'NONE', #7296, .T. ) ;
#43590 = DIRECTION ( 'NONE',  ( -0.005961354470445682716, -0.6427876096865404731, 0.7660212471507180654 ) ) ;
#43591 = ADVANCED_FACE ( 'NONE', ( #20036 ), #15499, .F. ) ;
#43592 = ADVANCED_FACE ( 'NONE', ( #32825 ), #28030, .F. ) ;
#43593 = CYLINDRICAL_SURFACE ( 'NONE', #16479, 0.2499999999999998612 ) ;
#43594 = DIRECTION ( 'NONE',  ( 0.9999697198139515519, 0.000000000000000000, 0.007781995580013368816 ) ) ;
#43595 = EDGE_CURVE ( 'NONE', #28974, #21716, #53572, .T. ) ;
#43596 = DIRECTION ( 'NONE',  ( 0.5364919789714477361, 0.6444004775717706579, 0.5449076811759711036 ) ) ;
#43597 = CARTESIAN_POINT ( 'NONE',  ( -27.99923088623136636, 0.000000000000000000, 7.757173251277078130 ) ) ;
#43598 = ORIENTED_EDGE ( 'NONE', *, *, #25108, .T. ) ;
#43599 = DIRECTION ( 'NONE',  ( 0.005961354470445682716, -0.6427876096865404731, -0.7660212471507180654 ) ) ;
#43600 = DIRECTION ( 'NONE',  ( 0.000000000000000000, -1.000000000000000000, 0.000000000000000000 ) ) ;
#43601 = ORIENTED_EDGE ( 'NONE', *, *, #42511, .F. ) ;
#43602 = CARTESIAN_POINT ( 'NONE',  ( -15.33107005804928313, 0.000000000000000000, 3.962433053780552328 ) ) ;
#43603 = ORIENTED_EDGE ( 'NONE', *, *, #54320, .F. ) ;
#43604 = CARTESIAN_POINT ( 'NONE',  ( -15.38456134770231110, -1.165603555308156736, 4.570771832407389823 ) ) ;
#43605 = LINE ( 'NONE', #24974, #2972 ) ;
#43606 = ORIENTED_EDGE ( 'NONE', *, *, #45332, .F. ) ;
#43607 = VECTOR ( 'NONE', #10980, 1000.000000000000227 ) ;
#43608 = VERTEX_POINT ( 'NONE', #50140 ) ;
#43609 = ORIENTED_EDGE ( 'NONE', *, *, #50485, .F. ) ;
#43610 = ORIENTED_EDGE ( 'NONE', *, *, #51560, .F. ) ;
#43611 = ORIENTED_EDGE ( 'NONE', *, *, #10080, .F. ) ;
#43612 = ORIENTED_EDGE ( 'NONE', *, *, #20343, .F. ) ;
#43613 = LINE ( 'NONE', #34284, #37699 ) ;
#43614 = CARTESIAN_POINT ( 'NONE',  ( -14.01623497886155256, -0.1191753592594197858, 2.226008083469502630 ) ) ;
#43615 = CARTESIAN_POINT ( 'NONE',  ( -14.00280974873554030, 0.000000000000000000, 12.40921378708904044 ) ) ;
#43616 = VECTOR ( 'NONE', #45719, 999.9999999999998863 ) ;
#43617 = ORIENTED_EDGE ( 'NONE', *, *, #14377, .F. ) ;
#43618 = CARTESIAN_POINT ( 'NONE',  ( -25.20123094555300369, 0.000000000000000000, 6.470945668149052032 ) ) ;
#43619 = ORIENTED_EDGE ( 'NONE', *, *, #43942, .T. ) ;
#43620 = ORIENTED_EDGE ( 'NONE', *, *, #4251, .T. ) ;
#43621 = ADVANCED_FACE ( 'NONE', ( #27762 ), #37358, .F. ) ;
#43622 = AXIS2_PLACEMENT_3D ( 'NONE', #12730, #35431, #47358 ) ;
#43623 = CARTESIAN_POINT ( 'NONE',  ( -12.80458192191714595, 0.000000000000000000, 11.86454056839041726 ) ) ;
#43624 = EDGE_CURVE ( 'NONE', #54774, #17288, #23750, .T. ) ;
#43625 = CARTESIAN_POINT ( 'NONE',  ( -16.81345671998191449, 0.000000000000000000, 3.412238694616132495 ) ) ;
#43626 = PLANE ( 'NONE',  #7796 ) ;
#43627 = EDGE_CURVE ( 'NONE', #6097, #5412, #28577, .T. ) ;
#43628 = EDGE_LOOP ( 'NONE', ( #23722, #19301, #11138, #30232 ) ) ;
#43629 = CARTESIAN_POINT ( 'NONE',  ( -13.63673279712320507, -0.1191753592594197858, 12.22739664767016521 ) ) ;
#43630 = ORIENTED_EDGE ( 'NONE', *, *, #51818, .F. ) ;
#43631 = CARTESIAN_POINT ( 'NONE',  ( -10.84028925556084388, -0.1191753592594197858, 11.14116300850493246 ) ) ;
#43632 = EDGE_CURVE ( 'NONE', #54969, #55411, #33956, .T. ) ;
#43633 = LINE ( 'NONE', #13286, #7595 ) ;
#43634 = PLANE ( 'NONE',  #36900 ) ;
#43635 = LINE ( 'NONE', #39399, #49443 ) ;
#43636 = CARTESIAN_POINT ( 'NONE',  ( -20.63663879154963965, 20.74370688441071664, -4.657437592157546824 ) ) ;
#43637 = CARTESIAN_POINT ( 'NONE',  ( -21.47263955680318404, 0.000000000000000000, 5.022634149262071190 ) ) ;
#43638 = CARTESIAN_POINT ( 'NONE',  ( 2.072287782118878319, 0.000000000000000000, -2.950529333540147015 ) ) ;
#43639 = CARTESIAN_POINT ( 'NONE',  ( -69.66748085948010782, -11.69676896150251011, 8.217082732571148185 ) ) ;
#43640 = ORIENTED_EDGE ( 'NONE', *, *, #17855, .T. ) ;
#43641 = LINE ( 'NONE', #4753, #49196 ) ;
#43642 = VECTOR ( 'NONE', #26096, 1000.000000000000227 ) ;
#43643 = VECTOR ( 'NONE', #52769, 999.9999999999998863 ) ;
#43644 = DIRECTION ( 'NONE',  ( 0.9999697198139515519, 0.000000000000000000, 0.007781995580013368816 ) ) ;
#43645 = CARTESIAN_POINT ( 'NONE',  ( -14.15152357901523139, 0.000000000000000000, 5.818272906257401900 ) ) ;
#43646 = CARTESIAN_POINT ( 'NONE',  ( -10.74029228357944987, 0.000000000000000000, 11.14194120806293320 ) ) ;
#43647 = CARTESIAN_POINT ( 'NONE',  ( -37.38198873126034272, 9.343723781475320678, -4.940473224498643567 ) ) ;
#43648 = DIRECTION ( 'NONE',  ( 0.5449076811759707706, 0.6444004775717708799, -0.5364919789714476250 ) ) ;
#43649 = DIRECTION ( 'NONE',  ( 0.3583679495452941066, 0.9335804264972041855, -0.000000000000000000 ) ) ;
#43650 = CARTESIAN_POINT ( 'NONE',  ( -18.76354595665420177, -0.1191753592594177458, 14.21882498613976331 ) ) ;
#43651 = ORIENTED_EDGE ( 'NONE', *, *, #24483, .F. ) ;
#43652 = CARTESIAN_POINT ( 'NONE',  ( -28.93060053386082231, -0.1191753592594197858, 8.019254159017428663 ) ) ;
#43653 = PLANE ( 'NONE',  #39428 ) ;
#43654 = FACE_OUTER_BOUND ( 'NONE', #51247, .T. ) ;
#43655 = ADVANCED_FACE ( 'NONE', ( #16934 ), #42738, .F. ) ;
#43656 = LINE ( 'NONE', #4238, #27312 ) ;
#43657 = DIRECTION ( 'NONE',  ( 0.005002170337468016433, -0.7660444431189770143, -0.6427681459581293666 ) ) ;
#43658 = LINE ( 'NONE', #49051, #23204 ) ;
#43659 = EDGE_CURVE ( 'NONE', #41210, #27927, #7858, .T. ) ;
#43660 = ADVANCED_FACE ( 'NONE', ( #29724 ), #17193, .F. ) ;
#43661 = LINE ( 'NONE', #18113, #8384 ) ;
#43662 = VECTOR ( 'NONE', #51401, 999.9999999999998863 ) ;
#43663 = CARTESIAN_POINT ( 'NONE',  ( -69.43545830293986398, -9.790829293527439248, 7.501778215771295777 ) ) ;
#43664 = ORIENTED_EDGE ( 'NONE', *, *, #14564, .F. ) ;
#43665 = LINE ( 'NONE', #4249, #55526 ) ;
#43666 = B_SPLINE_CURVE_WITH_KNOTS ( 'NONE', 3,
 ( #49084, #10186, #13607, #48536 ),
 .UNSPECIFIED., .F., .F.,
 ( 4, 4 ),
 ( 0.5868166818973559185, 0.6110328696463859233 ),
 .UNSPECIFIED. ) ;
#43667 = ORIENTED_EDGE ( 'NONE', *, *, #38620, .F. ) ;
#43668 = EDGE_CURVE ( 'NONE', #21619, #43550, #42197, .T. ) ;
#43669 = VERTEX_POINT ( 'NONE', #54990 ) ;
#43670 = VERTEX_POINT ( 'NONE', #20631 ) ;
#43671 = ORIENTED_EDGE ( 'NONE', *, *, #40617, .T. ) ;
#43672 = ORIENTED_EDGE ( 'NONE', *, *, #11613, .T. ) ;
#43673 = CARTESIAN_POINT ( 'NONE',  ( -21.47419595591918906, 0.000000000000000000, 5.222628093224860102 ) ) ;
#43674 = PLANE ( 'NONE',  #24878 ) ;
#43675 = AXIS2_PLACEMENT_3D ( 'NONE', #11261, #50983, #2473 ) ;
#43676 = AXIS2_PLACEMENT_3D ( 'NONE', #6924, #33025, #3490 ) ;
#43677 = VERTEX_POINT ( 'NONE', #3839 ) ;
#43678 = ORIENTED_EDGE ( 'NONE', *, *, #30907, .T. ) ;
#43679 = CARTESIAN_POINT ( 'NONE',  ( -65.63888213997375942, -3.295974604355933479E-14, -1.301894315629612997 ) ) ;
#43680 = ORIENTED_EDGE ( 'NONE', *, *, #13722, .F. ) ;
#43681 = DIRECTION ( 'NONE',  ( -0.000000000000000000, -0.000000000000000000, -1.000000000000000000 ) ) ;
#43682 = LINE ( 'NONE', #51928, #17722 ) ;
#43683 = EDGE_LOOP ( 'NONE', ( #52117, #25833, #23897, #25489 ) ) ;
#43684 = DIRECTION ( 'NONE',  ( -0.005002170337468016433, -0.7660444431189770143, 0.6427681459581293666 ) ) ;
#43685 = ORIENTED_EDGE ( 'NONE', *, *, #12638, .T. ) ;
#43686 = CARTESIAN_POINT ( 'NONE',  ( -14.19717356985994705, -3.594132820645661308, 8.095180354891688523 ) ) ;
#43687 = ADVANCED_FACE ( 'NONE', ( #37942 ), #29419, .F. ) ;
#43688 = VECTOR ( 'NONE', #27497, 1000.000000000000227 ) ;
#43689 = VECTOR ( 'NONE', #7903, 1000.000000000000227 ) ;
#43690 = DIRECTION ( 'NONE',  ( -0.9999697198139514409, -0.000000000000000000, -0.007781995580013368816 ) ) ;
#43691 = DIRECTION ( 'NONE',  ( -0.000000000000000000, -0.000000000000000000, -1.000000000000000000 ) ) ;
#43692 = ORIENTED_EDGE ( 'NONE', *, *, #7614, .T. ) ;
#43693 = LINE ( 'NONE', #39748, #32178 ) ;
#43694 = LINE ( 'NONE', #53082, #47431 ) ;
#43695 = LINE ( 'NONE', #13608, #25739 ) ;
#43696 = ORIENTED_EDGE ( 'NONE', *, *, #26683, .F. ) ;
#43697 = CARTESIAN_POINT ( 'NONE',  ( 1.969897575278193980, 0.000000000000000000, 10.20639235748909890 ) ) ;
#43698 = ORIENTED_EDGE ( 'NONE', *, *, #55337, .T. ) ;
#43699 = EDGE_CURVE ( 'NONE', #35428, #52435, #38491, .T. ) ;
#43700 = CARTESIAN_POINT ( 'NONE',  ( -15.36998915273395738, 0.000000000000000000, 8.963453140094282290 ) ) ;
#43701 = CARTESIAN_POINT ( 'NONE',  ( -27.06708303904391144, 0.000000000000000000, 7.395095371555332697 ) ) ;
#43702 = FACE_OUTER_BOUND ( 'NONE', #44417, .T. ) ;
#43703 = LINE ( 'NONE', #47722, #7830 ) ;
#43704 = CARTESIAN_POINT ( 'NONE',  ( -12.62965358101575397, -0.1191753592594188005, 2.236798780523178820 ) ) ;
#43705 = EDGE_CURVE ( 'NONE', #2028, #12064, #25712, .T. ) ;
#43706 = DIRECTION ( 'NONE',  ( 0.005002170337468016433, -0.7660444431189770143, -0.6427681459581293666 ) ) ;
#43708 = ADVANCED_FACE ( 'NONE', ( #38201 ), #46428, .F. ) ;
#43707 = CARTESIAN_POINT ( 'NONE',  ( -14.12003756145438871, 4.981562823951513508, 2.007695903425033901 ) ) ;
#43709 = CARTESIAN_POINT ( 'NONE',  ( -25.20200914511100265, -0.1191753592594197858, 6.570942640130446932 ) ) ;
#43710 = FILL_AREA_STYLE_COLOUR ( '', #6284 ) ;
#43711 = LINE ( 'NONE', #56228, #37773 ) ;
#43712 = EDGE_LOOP ( 'NONE', ( #2441, #14584, #44669, #7896 ) ) ;
#43713 = VECTOR ( 'NONE', #395, 999.9999999999998863 ) ;
#43714 = CARTESIAN_POINT ( 'NONE',  ( -22.15441699824221899, 19.68629271404579484, -4.426028624882090590 ) ) ;
#43715 = EDGE_CURVE ( 'NONE', #46599, #41809, #21167, .T. ) ;
#43716 = LINE ( 'NONE', #52534, #32712 ) ;
#43717 = DIRECTION ( 'NONE',  ( 0.5449076811759707706, 0.6444004775717708799, -0.5364919789714476250 ) ) ;
#43718 = VECTOR ( 'NONE', #33901, 1000.000000000000114 ) ;
#43719 = VECTOR ( 'NONE', #30095, 1000.000000000000000 ) ;
#43720 = EDGE_CURVE ( 'NONE', #42927, #54093, #8698, .T. ) ;
#43721 = CARTESIAN_POINT ( 'NONE',  ( -12.60956183379353845, -3.917936722690661178, 8.009915408982919871 ) ) ;
#43722 = DIRECTION ( 'NONE',  ( -0.7660212471507179544, -0.6427876096865405842, -0.005961354470445141482 ) ) ;
#43723 = EDGE_CURVE ( 'NONE', #44901, #26765, #16627, .T. ) ;
#43724 = CARTESIAN_POINT ( 'NONE',  ( -3.638205267667341758, -7.220147766006030032, -1.805171095730843112 ) ) ;
#43725 = ORIENTED_EDGE ( 'NONE', *, *, #9572, .T. ) ;
#43726 = VECTOR ( 'NONE', #30282, 999.9999999999998863 ) ;
#43727 = AXIS2_PLACEMENT_3D ( 'NONE', #28412, #32959, #37799 ) ;
#43728 = ORIENTED_EDGE ( 'NONE', *, *, #9960, .F. ) ;
#43729 = CARTESIAN_POINT ( 'NONE',  ( -14.93495759592298988, 0.000000000000000000, 12.77129166681078409 ) ) ;
#43730 = LINE ( 'NONE', #4843, #40447 ) ;
#43731 = EDGE_LOOP ( 'NONE', ( #28226, #26132, #41398, #44213 ) ) ;
#43732 = PLANE ( 'NONE',  #18420 ) ;
#43733 = EDGE_CURVE ( 'NONE', #54076, #7274, #35044, .T. ) ;
#43734 = ORIENTED_EDGE ( 'NONE', *, *, #16891, .F. ) ;
#43735 = LINE ( 'NONE', #13638, #22267 ) ;
#43736 = MECHANICAL_DESIGN_GEOMETRIC_PRESENTATION_REPRESENTATION (  '', ( #31960 ), #50984 ) ;
#43737 = ORIENTED_EDGE ( 'NONE', *, *, #43917, .T. ) ;
#43738 = LINE ( 'NONE', #39508, #7524 ) ;
#43739 = EDGE_CURVE ( 'NONE', #41032, #29707, #12932, .T. ) ;
#43740 = ORIENTED_EDGE ( 'NONE', *, *, #817, .T. ) ;
#43741 = ORIENTED_EDGE ( 'NONE', *, *, #31553, .F. ) ;
#43742 = ORIENTED_EDGE ( 'NONE', *, *, #32299, .F. ) ;
#43743 = CARTESIAN_POINT ( 'NONE',  ( -13.58962795970950843, 1.581621852479004664, 1.910142718956624908 ) ) ;
#43744 = PLANE ( 'NONE',  #15094 ) ;
#43745 = DIRECTION ( 'NONE',  ( -0.5364919789714478471, 0.6444004775717705469, -0.5449076811759709926 ) ) ;
#43746 = DIRECTION ( 'NONE',  ( 0.007781995580012663651, -3.146120232559066537E-19, -0.9999697198139514409 ) ) ;
#43747 = EDGE_LOOP ( 'NONE', ( #29980, #11693, #56213, #44366, #53302 ) ) ;
#43748 = EDGE_LOOP ( 'NONE', ( #42300, #34198, #9007, #472 ) ) ;
#43749 = AXIS2_PLACEMENT_3D ( 'NONE', #40864, #36613, #5969 ) ;
#43750 = LINE ( 'NONE', #34991, #16399 ) ;
#43751 = ORIENTED_EDGE ( 'NONE', *, *, #39713, .F. ) ;
#43752 = AXIS2_PLACEMENT_3D ( 'NONE', #922, #5478, #4381 ) ;
#43753 = CARTESIAN_POINT ( 'NONE',  ( -10.21874653840805891, 0.000000000000000000, 3.832892323933682732 ) ) ;
#43754 = EDGE_LOOP ( 'NONE', ( #47740, #32530, #1436, #18951 ) ) ;
#43755 = LINE ( 'NONE', #26183, #24216 ) ;
#43756 = CARTESIAN_POINT ( 'NONE',  ( -17.74560456716937296, 0.000000000000000000, 3.774316574337878372 ) ) ;
#43757 = AXIS2_PLACEMENT_3D ( 'NONE', #25506, #29200, #34331 ) ;
#43758 = AXIS2_PLACEMENT_3D ( 'NONE', #20315, #7541, #42188 ) ;
#43759 = ORIENTED_EDGE ( 'NONE', *, *, #31657, .F. ) ;
#43760 = FACE_OUTER_BOUND ( 'NONE', #5151, .T. ) ;
#43761 = EDGE_CURVE ( 'NONE', #27148, #31034, #20325, .T. ) ;
#43762 = VERTEX_POINT ( 'NONE', #7549 ) ;
#43763 = AXIS2_PLACEMENT_3D ( 'NONE', #50860, #32704, #16232 ) ;
#43764 = DIRECTION ( 'NONE',  ( -0.9321478471874540261, 0.000000000000000000, 0.3620778797217457656 ) ) ;
#43765 = VECTOR ( 'NONE', #5652, 1000.000000000000000 ) ;
#43766 = ORIENTED_EDGE ( 'NONE', *, *, #39081, .T. ) ;
#43767 = LINE ( 'NONE', #27584, #38530 ) ;
#43768 = CARTESIAN_POINT ( 'NONE',  ( -16.26034385173145580, 0.000000000000000000, 3.955201230244533850 ) ) ;
#43769 = CARTESIAN_POINT ( 'NONE',  ( -15.75813278794938732, -0.5179957512181557755, 2.985788263993758296 ) ) ;
#43770 = ORIENTED_EDGE ( 'NONE', *, *, #53471, .F. ) ;
#43771 = DIRECTION ( 'NONE',  ( 0.9999697198139515519, 0.000000000000000000, 0.007781995580013368816 ) ) ;
#43772 = LINE ( 'NONE', #55728, #24628 ) ;
#43773 = CARTESIAN_POINT ( 'NONE',  ( -12.33850799832341849, 0.000000000000000000, 11.68350162852954632 ) ) ;
#43774 = VECTOR ( 'NONE', #6776, 1000.000000000000227 ) ;
#43775 = DIRECTION ( 'NONE',  ( 0.007781995580012662783, 0.000000000000000000, -0.9999697198139514409 ) ) ;
#43776 = VECTOR ( 'NONE', #22483, 1000.000000000000227 ) ;
#43777 = FACE_OUTER_BOUND ( 'NONE', #53602, .T. ) ;
#43779 = EDGE_CURVE ( 'NONE', #29854, #50717, #34508, .T. ) ;
#43778 = CARTESIAN_POINT ( 'NONE',  ( -17.29901497746887173, -0.1191753592594167882, 5.155117288905197270 ) ) ;
#43780 =( LENGTH_UNIT ( ) NAMED_UNIT ( * ) SI_UNIT ( .MILLI., .METRE. ) );
#43781 = ORIENTED_EDGE ( 'NONE', *, *, #52802, .F. ) ;
#43782 = PLANE ( 'NONE',  #20742 ) ;
#43783 = PLANE ( 'NONE',  #38596 ) ;
#43784 = CARTESIAN_POINT ( 'NONE',  ( -14.20280369269832832, 0.000000000000000000, 12.40765738797303719 ) ) ;
#43785 = VERTEX_POINT ( 'NONE', #47576 ) ;
#43786 = CARTESIAN_POINT ( 'NONE',  ( -20.28958894222632736, -4.241740624735664156, 4.627152765803700163 ) ) ;
#43787 = ORIENTED_EDGE ( 'NONE', *, *, #2534, .F. ) ;
#43788 = VECTOR ( 'NONE', #44215, 999.9999999999998863 ) ;
#43789 = DIRECTION ( 'NONE',  ( -0.005961354470445682716, -0.6427876096865404731, 0.7660212471507180654 ) ) ;
#43790 = ADVANCED_FACE ( 'NONE', ( #37663 ), #1259, .F. ) ;
#43791 = CARTESIAN_POINT ( 'NONE',  ( -11.47013034581549462, -2.622721114510659479, 1.253030735756987424 ) ) ;
#43792 = AXIS2_PLACEMENT_3D ( 'NONE', #2017, #32446, #49478 ) ;
#43793 = PLANE ( 'NONE',  #26897 ) ;
#43794 = EDGE_CURVE ( 'NONE', #329, #38597, #17771, .T. ) ;
#43795 = CARTESIAN_POINT ( 'NONE',  ( -10.42005813676012949, 0.000000000000000000, 4.000651684112655815 ) ) ;
#43796 = ORIENTED_EDGE ( 'NONE', *, *, #4691, .T. ) ;
#43797 = ORIENTED_EDGE ( 'NONE', *, *, #2621, .F. ) ;
#43798 = DIRECTION ( 'NONE',  ( 0.7660212471507180654, -0.6427876096865404731, 0.005961354470445141482 ) ) ;
#43799 = CARTESIAN_POINT ( 'NONE',  ( -24.57312852195785524, 18.34675584111407787, 4.549864924635812713 ) ) ;
#43800 = AXIS2_PLACEMENT_3D ( 'NONE', #3455, #25581, #8265 ) ;
#43801 = CARTESIAN_POINT ( 'NONE',  ( -26.13337879274045505, 0.000000000000000000, 6.833023547870798353 ) ) ;
#43802 = VECTOR ( 'NONE', #44184, 1000.000000000000227 ) ;
#43803 = DIRECTION ( 'NONE',  ( 0.5364919789714477361, 0.6444004775717706579, 0.5449076811759711036 ) ) ;
#43804 = ADVANCED_FACE ( 'NONE', ( #22847 ), #44169, .F. ) ;
#43805 = AXIS2_PLACEMENT_3D ( 'NONE', #31077, #1254, #53257 ) ;
#43806 = DIRECTION ( 'NONE',  ( 0.5364919789714477361, 0.6444004775717706579, 0.5449076811759711036 ) ) ;
#43807 = DIRECTION ( 'NONE',  ( 0.9999697198139515519, 0.000000000000000000, 0.007781995580013368816 ) ) ;
#43808 = ORIENTED_EDGE ( 'NONE', *, *, #49248, .F. ) ;
#43809 = FACE_OUTER_BOUND ( 'NONE', #33069, .T. ) ;
#43810 = ADVANCED_FACE ( 'NONE', ( #40167 ), #9815, .F. ) ;
#43811 = VECTOR ( 'NONE', #51388, 999.9999999999998863 ) ;
#43812 = PLANE ( 'NONE',  #36045 ) ;
#43813 = VECTOR ( 'NONE', #2156, 999.9999999999998863 ) ;
#43814 = VERTEX_POINT ( 'NONE', #5274 ) ;
#43815 = LINE ( 'NONE', #22255, #21112 ) ;
#43816 = PLANE ( 'NONE',  #32290 ) ;
#43817 = PLANE ( 'NONE',  #32057 ) ;
#43818 = ORIENTED_EDGE ( 'NONE', *, *, #33888, .T. ) ;
#43819 = CARTESIAN_POINT ( 'NONE',  ( -14.46888367232926420, 0.000000000000000000, 12.59025272694991315 ) ) ;
#43820 = VERTEX_POINT ( 'NONE', #22008 ) ;
#43821 = VECTOR ( 'NONE', #35390, 1000.000000000000227 ) ;
#43822 = ORIENTED_EDGE ( 'NONE', *, *, #36983, .T. ) ;
#43823 = ORIENTED_EDGE ( 'NONE', *, *, #13380, .F. ) ;
#43824 = VERTEX_POINT ( 'NONE', #34795 ) ;
#43825 = CARTESIAN_POINT ( 'NONE',  ( -16.60113548713373888, 2.391131607591508335, 3.054086914397361685 ) ) ;
#43827 = ADVANCED_FACE ( 'NONE', ( #18038 ), #26846, .T. ) ;
#43826 = EDGE_LOOP ( 'NONE', ( #6425, #10741, #8864, #35994 ) ) ;
#43828 = AXIS2_PLACEMENT_3D ( 'NONE', #45502, #11453, #37555 ) ;
#43829 = CARTESIAN_POINT ( 'NONE',  ( -11.77243710274829525, -0.1191753592594197858, 11.50324088822667612 ) ) ;
#43830 = ORIENTED_EDGE ( 'NONE', *, *, #39985, .F. ) ;
#43831 = DIRECTION ( 'NONE',  ( 0.5449076811759707706, 0.6444004775717708799, -0.5364919789714476250 ) ) ;
#43832 = VERTEX_POINT ( 'NONE', #9225 ) ;
#43833 = DIRECTION ( 'NONE',  ( -0.7660212471507179544, -0.6427876096865405842, -0.005961354470445141482 ) ) ;
#43834 = EDGE_CURVE ( 'NONE', #20287, #26373, #18597, .T. ) ;
#43835 = VECTOR ( 'NONE', #33542, 999.9999999999998863 ) ;
#43836 = VERTEX_POINT ( 'NONE', #22583 ) ;
#43837 = EDGE_CURVE ( 'NONE', #55008, #17361, #4981, .T. ) ;
#43838 = DIRECTION ( 'NONE',  ( 0.9999697198139515519, 0.000000000000000000, 0.007781995580013368816 ) ) ;
#43839 = LINE ( 'NONE', #40718, #15079 ) ;
#43840 = EDGE_CURVE ( 'NONE', #30649, #29572, #425, .T. ) ;
#43841 = LINE ( 'NONE', #39032, #24967 ) ;
#43842 = DIRECTION ( 'NONE',  ( 0.5449076811759707706, 0.6444004775717708799, -0.5364919789714476250 ) ) ;
#43843 = VECTOR ( 'NONE', #40500, 1000.000000000000114 ) ;
#43844 = CARTESIAN_POINT ( 'NONE',  ( -15.39653247616405096, 2.067327705546508021, 2.596509236221068218 ) ) ;
#43845 = ORIENTED_EDGE ( 'NONE', *, *, #15372, .T. ) ;
#43846 = EDGE_CURVE ( 'NONE', #49012, #17901, #53263, .T. ) ;
#43847 = EDGE_CURVE ( 'NONE', #43483, #13988, #39893, .T. ) ;
#43848 = EDGE_CURVE ( 'NONE', #1080, #13383, #35104, .T. ) ;
#43849 = VECTOR ( 'NONE', #18496, 999.9999999999998863 ) ;
#43850 = AXIS2_PLACEMENT_3D ( 'NONE', #40552, #14146, #23494 ) ;
#43851 = ORIENTED_EDGE ( 'NONE', *, *, #32980, .F. ) ;
#43852 = LINE ( 'NONE', #25696, #49418 ) ;
#43853 = CARTESIAN_POINT ( 'NONE',  ( -18.67619601524082285, 0.000000000000000000, 3.936400510096834893 ) ) ;
#43854 = LINE ( 'NONE', #31377, #46008 ) ;
#43855 = AXIS2_PLACEMENT_3D ( 'NONE', #5855, #9845, #19457 ) ;
#43856 = VECTOR ( 'NONE', #17258, 999.9999999999998863 ) ;
#43857 = CARTESIAN_POINT ( 'NONE',  ( -14.94421173320987428, 3.686347215771509145, 8.736084265198291732 ) ) ;
#43858 = FACE_OUTER_BOUND ( 'NONE', #4782, .T. ) ;
#43859 = CARTESIAN_POINT ( 'NONE',  ( -19.49503486152984166, 0.000000000000000000, 7.454022801337932158 ) ) ;
#43860 = ORIENTED_EDGE ( 'NONE', *, *, #52572, .T. ) ;
#43861 = DIRECTION ( 'NONE',  ( -0.8531650599175527594, 0.4028455766673922356, 0.3313982828793700652 ) ) ;
#43862 = DIRECTION ( 'NONE',  ( -0.05705673239519651330, 0.9983709377222391712, 2.351258244848514932E-16 ) ) ;
#43863 = ORIENTED_EDGE ( 'NONE', *, *, #33366, .T. ) ;
#43864 = DIRECTION ( 'NONE',  ( 0.6427681459581294776, -0.7660444431189769032, 0.005002170337467562802 ) ) ;
#43865 = PLANE ( 'NONE',  #35125 ) ;
#43866 = EDGE_CURVE ( 'NONE', #5703, #55216, #48408, .T. ) ;
#43867 = DIRECTION ( 'NONE',  ( 0.9999697198139515519, 0.000000000000000000, 0.007781995580013368816 ) ) ;
#43868 = DIRECTION ( 'NONE',  ( -0.005961354470445682716, -0.6427876096865404731, 0.7660212471507180654 ) ) ;
#43869 = EDGE_CURVE ( 'NONE', #12359, #13117, #30818, .T. ) ;
#43870 = PLANE ( 'NONE',  #21092 ) ;
#43871 = ORIENTED_EDGE ( 'NONE', *, *, #11788, .F. ) ;
#43872 = VECTOR ( 'NONE', #10322, 999.9999999999998863 ) ;
#43873 = ORIENTED_EDGE ( 'NONE', *, *, #38698, .T. ) ;
#43874 = ADVANCED_FACE ( 'NONE', ( #13504 ), #4432, .F. ) ;
#43875 = LINE ( 'NONE', #30825, #357 ) ;
#43876 = DIRECTION ( 'NONE',  ( -0.005961354470445682716, -0.6427876096865404731, 0.7660212471507180654 ) ) ;
#43877 = CARTESIAN_POINT ( 'NONE',  ( -9.939733318003350249, 0.000000000000000000, 1.988403320296867616 ) ) ;
#43878 = AXIS2_PLACEMENT_3D ( 'NONE', #47335, #8752, #25768 ) ;
#43879 = ADVANCED_FACE ( 'NONE', ( #717 ), #21740, .T. ) ;
#43880 = DIRECTION ( 'NONE',  ( -0.7660212471507179544, -0.6427876096865405842, -0.005961354470445141482 ) ) ;
#43881 = CARTESIAN_POINT ( 'NONE',  ( -10.76754721030951245, -0.6798977022406572646, 1.042109824751433989 ) ) ;
#43882 = VECTOR ( 'NONE', #31459, 1000.000000000000000 ) ;
#43883 = CARTESIAN_POINT ( 'NONE',  ( -13.95518489968810627, 24.60124608745501007, -3.681743400992149695 ) ) ;
#43884 = DIRECTION ( 'NONE',  ( 0.000000000000000000, -0.000000000000000000, -1.000000000000000000 ) ) ;
#43885 = CARTESIAN_POINT ( 'NONE',  ( -18.39746900504187010, 0.000000000000000000, 14.03700784672088808 ) ) ;
#43886 = DIRECTION ( 'NONE',  ( 0.000000000000000000, -0.000000000000000000, -1.000000000000000000 ) ) ;
#43887 = VECTOR ( 'NONE', #32706, 1000.000000000000000 ) ;
#43888 = EDGE_LOOP ( 'NONE', ( #1511, #11157, #44190, #30521 ) ) ;
#43889 = CARTESIAN_POINT ( 'NONE',  ( -21.47263955680318404, 0.000000000000000000, 5.022634149262071190 ) ) ;
#43890 = ORIENTED_EDGE ( 'NONE', *, *, #5466, .F. ) ;
#43891 = PLANE ( 'NONE',  #46782 ) ;
#43892 = DIRECTION ( 'NONE',  ( -0.7660212471507179544, -0.6427876096865405842, -0.005961354470445141482 ) ) ;
#43893 = VECTOR ( 'NONE', #23339, 1000.000000000000114 ) ;
#43894 = ORIENTED_EDGE ( 'NONE', *, *, #17022, .F. ) ;
#43895 = EDGE_LOOP ( 'NONE', ( #50020, #16219, #6441, #46532 ) ) ;
#43896 = AXIS2_PLACEMENT_3D ( 'NONE', #7029, #49878, #24053 ) ;
#43897 = VERTEX_POINT ( 'NONE', #13227 ) ;
#43898 = ORIENTED_EDGE ( 'NONE', *, *, #3306, .F. ) ;
#43899 = VECTOR ( 'NONE', #24582, 1000.000000000000000 ) ;
#43900 = ORIENTED_EDGE ( 'NONE', *, *, #39675, .T. ) ;
#43901 = ORIENTED_EDGE ( 'NONE', *, *, #17503, .F. ) ;
#43902 = LINE ( 'NONE', #13268, #46528 ) ;
#43903 = DIRECTION ( 'NONE',  ( -0.000000000000000000, -0.000000000000000000, -1.000000000000000000 ) ) ;
#43904 = VERTEX_POINT ( 'NONE', #47869 ) ;
#43905 = CARTESIAN_POINT ( 'NONE',  ( -12.23851102634202448, -0.1191753592594197858, 11.68427982808754884 ) ) ;
#43906 = ORIENTED_EDGE ( 'NONE', *, *, #14710, .F. ) ;
#43907 = ORIENTED_EDGE ( 'NONE', *, *, #38550, .F. ) ;
#43908 = VECTOR ( 'NONE', #7967, 1000.000000000000114 ) ;
#43909 = DIRECTION ( 'NONE',  ( -0.7660212471507179544, -0.6427876096865405842, -0.005961354470445141482 ) ) ;
#43910 = VECTOR ( 'NONE', #45772, 999.9999999999998863 ) ;
#43911 = LINE ( 'NONE', #31136, #5870 ) ;
#43912 = LINE ( 'NONE', #9577, #25961 ) ;
#43913 = VERTEX_POINT ( 'NONE', #8970 ) ;
#43914 = PLANE ( 'NONE',  #18325 ) ;
#43915 = VECTOR ( 'NONE', #49531, 1000.000000000000114 ) ;
#43916 = VERTEX_POINT ( 'NONE', #49809 ) ;
#43917 = EDGE_CURVE ( 'NONE', #14283, #36681, #41000, .T. ) ;
#43918 = ADVANCED_FACE ( 'NONE', ( #50369 ), #6123, .F. ) ;
#43919 = LINE ( 'NONE', #9016, #3042 ) ;
#43920 = EDGE_CURVE ( 'NONE', #13117, #11647, #19137, .T. ) ;
#43921 = CARTESIAN_POINT ( 'NONE',  ( -13.48689273821135259, 0.000000000000000000, 5.823445217141414609 ) ) ;
#43922 = DIRECTION ( 'NONE',  ( 0.005961354470445682716, -0.6427876096865404731, -0.7660212471507180654 ) ) ;
#43923 = LINE ( 'NONE', #5047, #52116 ) ;
#43924 = CARTESIAN_POINT ( 'NONE',  ( -9.312465172768151334, 0.000000000000000000, 6.794601773531817379 ) ) ;
#43925 = DIRECTION ( 'NONE',  ( 0.000000000000000000, -0.000000000000000000, -1.000000000000000000 ) ) ;
#43926 = VECTOR ( 'NONE', #4789, 1000.000000000000227 ) ;
#43927 = DIRECTION ( 'NONE',  ( -0.005961354470445682716, -0.6427876096865404731, 0.7660212471507180654 ) ) ;
#43928 = ORIENTED_EDGE ( 'NONE', *, *, #37142, .F. ) ;
#43929 = CARTESIAN_POINT ( 'NONE',  ( -10.47421230394850866, 0.000000000000000000, 10.95934586908605723 ) ) ;
#43930 = AXIS2_PLACEMENT_3D ( 'NONE', #15022, #46209, #37412 ) ;
#43931 = DIRECTION ( 'NONE',  ( 0.007781995580012663651, -3.146120232559066537E-19, -0.9999697198139514409 ) ) ;
#43932 = CARTESIAN_POINT ( 'NONE',  ( -9.480844528172831076, 0.000000000000000000, 2.730638638580407118 ) ) ;
#43933 = PLANE ( 'NONE',  #36299 ) ;
#43934 = CARTESIAN_POINT ( 'NONE',  ( -45.77156441860525149, 4.499999999999981348, -5.000000000000000000 ) ) ;
#43935 = CARTESIAN_POINT ( 'NONE',  ( 5.282355347525632183, -1.069580340602398705, -2.393146392891059460 ) ) ;
#43936 = ADVANCED_FACE ( 'NONE', ( #36462 ), #23427, .F. ) ;
#43937 = DIRECTION ( 'NONE',  ( -0.6246952433987893460, -0.7422098413412802076, 0.2426528472758542054 ) ) ;
#43938 = AXIS2_PLACEMENT_3D ( 'NONE', #23625, #45222, #23082 ) ;
#43939 = CARTESIAN_POINT ( 'NONE',  ( -9.808144436391993182, 0.000000000000000000, 10.77986332834118777 ) ) ;
#43940 = VECTOR ( 'NONE', #20262, 999.9999999999998863 ) ;
#43941 = ORIENTED_EDGE ( 'NONE', *, *, #20121, .T. ) ;
#43942 = EDGE_CURVE ( 'NONE', #17442, #52077, #54081, .T. ) ;
#43943 = LINE ( 'NONE', #48790, #40219 ) ;
#43944 = CARTESIAN_POINT ( 'NONE',  ( -25.20123094555300369, 0.000000000000000000, 6.470945668149052032 ) ) ;
#43945 = DIRECTION ( 'NONE',  ( 0.9999697198139515519, 0.000000000000000000, 0.007781995580013368816 ) ) ;
#43946 = EDGE_CURVE ( 'NONE', #31801, #5857, #53778, .T. ) ;
#43947 = CARTESIAN_POINT ( 'NONE',  ( -12.80458192191714595, 0.000000000000000000, 11.86454056839041726 ) ) ;
#43948 = LINE ( 'NONE', #17859, #34875 ) ;
#43949 = DIRECTION ( 'NONE',  ( 0.7660212471507180654, -0.6427876096865404731, 0.005961354470445141482 ) ) ;
#43950 = FACE_OUTER_BOUND ( 'NONE', #26852, .T. ) ;
#43951 = EDGE_CURVE ( 'NONE', #12635, #17633, #36208, .T. ) ;
#43952 = AXIS2_PLACEMENT_3D ( 'NONE', #10446, #53857, #54408 ) ;
#43953 = CARTESIAN_POINT ( 'NONE',  ( -69.32931325251749399, -9.778513531655887547, 7.370754069753730597 ) ) ;
#43954 = VECTOR ( 'NONE', #3738, 1000.000000000000227 ) ;
#43955 = CARTESIAN_POINT ( 'NONE',  ( -9.442067484779661513, -0.1191753592594197858, 10.59804618892231254 ) ) ;
#43956 = VECTOR ( 'NONE', #38714, 1000.000000000000114 ) ;
#43957 = ORIENTED_EDGE ( 'NONE', *, *, #5299, .F. ) ;
#43958 = VECTOR ( 'NONE', #19888, 999.9999999999998863 ) ;
#43959 = ORIENTED_EDGE ( 'NONE', *, *, #11402, .T. ) ;
#43960 = VERTEX_POINT ( 'NONE', #1811 ) ;
#43961 = VECTOR ( 'NONE', #21236, 1000.000000000000114 ) ;
#43962 = VECTOR ( 'NONE', #45809, 1000.000000000000227 ) ;
#43963 = ORIENTED_EDGE ( 'NONE', *, *, #1623, .F. ) ;
#43964 = VECTOR ( 'NONE', #34152, 999.9999999999998863 ) ;
#43965 = EDGE_LOOP ( 'NONE', ( #27874, #28075, #9962, #7891 ) ) ;
#43966 = FACE_OUTER_BOUND ( 'NONE', #42995, .T. ) ;
#43967 = DIRECTION ( 'NONE',  ( 0.007781995580012663651, 0.000000000000000000, -0.9999697198139515519 ) ) ;
#43968 = VECTOR ( 'NONE', #27042, 1000.000000000000227 ) ;
#43969 = EDGE_LOOP ( 'NONE', ( #49553, #26258, #29308, #23997 ) ) ;
#43970 = ORIENTED_EDGE ( 'NONE', *, *, #18533, .F. ) ;
#43971 = AXIS2_PLACEMENT_3D ( 'NONE', #40331, #41165, #18461 ) ;
#43972 = VECTOR ( 'NONE', #47011, 999.9999999999998863 ) ;
#43973 = PLANE ( 'NONE',  #39396 ) ;
#43974 = ORIENTED_EDGE ( 'NONE', *, *, #33597, .T. ) ;
#43975 = DIRECTION ( 'NONE',  ( 0.000000000000000000, -0.000000000000000000, -1.000000000000000000 ) ) ;
#43976 = LINE ( 'NONE', #41661, #27784 ) ;
#43977 = ORIENTED_EDGE ( 'NONE', *, *, #40404, .T. ) ;
#43978 = DIRECTION ( 'NONE',  ( 0.007781995580012663651, 0.000000000000000000, -0.9999697198139515519 ) ) ;
#43980 = ORIENTED_EDGE ( 'NONE', *, *, #27906, .T. ) ;
#43979 = ADVANCED_FACE ( 'NONE', ( #32225 ), #10664, .F. ) ;
#43981 = LINE ( 'NONE', #35460, #30040 ) ;
#43982 = CARTESIAN_POINT ( 'NONE',  ( -12.77066550162910730, 0.000000000000000000, 7.506353398555276613 ) ) ;
#43983 = ADVANCED_FACE ( 'NONE', ( #40474 ), #45276, .F. ) ;
#43984 = EDGE_CURVE ( 'NONE', #51541, #38019, #6650, .T. ) ;
#43985 = AXIS2_PLACEMENT_3D ( 'NONE', #4697, #14073, #4438 ) ;
#43986 = DIRECTION ( 'NONE',  ( 0.5364919789714477361, 0.6444004775717706579, 0.5449076811759711036 ) ) ;
#43987 = DIRECTION ( 'NONE',  ( -0.9999697198139514409, -0.000000000000000000, -0.007781995580013368816 ) ) ;
#43988 = VERTEX_POINT ( 'NONE', #41296 ) ;
#43989 = DIRECTION ( 'NONE',  ( 0.000000000000000000, -0.000000000000000000, -1.000000000000000000 ) ) ;
#43990 = LINE ( 'NONE', #44537, #13865 ) ;
#43992 = VECTOR ( 'NONE', #5865, 1000.000000000000000 ) ;
#43991 = DIRECTION ( 'NONE',  ( 0.007781995580012663651, 0.000000000000000000, -0.9999697198139515519 ) ) ;
#43993 = VERTEX_POINT ( 'NONE', #23679 ) ;
#43994 = LINE ( 'NONE', #38908, #21060 ) ;
#43995 = ORIENTED_EDGE ( 'NONE', *, *, #40275, .T. ) ;
#43996 = AXIS2_PLACEMENT_3D ( 'NONE', #20625, #33950, #27827 ) ;
#43997 = PLANE ( 'NONE',  #14716 ) ;
#43998 = DIRECTION ( 'NONE',  ( -0.005002170337468016433, -0.7660444431189770143, 0.6427681459581293666 ) ) ;
#43999 = CARTESIAN_POINT ( 'NONE',  ( -17.62617585138765008, -3.117730071725258956, 12.26528855537868701 ) ) ;
#44000 = LINE ( 'NONE', #34941, #23235 ) ;
#44001 = AXIS2_PLACEMENT_3D ( 'NONE', #34019, #46796, #46207 ) ;
#44002 = DIRECTION ( 'NONE',  ( -0.7660212471507179544, -0.6427876096865405842, -0.005961354470445141482 ) ) ;
#44003 = DIRECTION ( 'NONE',  ( 0.005002170337468016433, -0.7660444431189770143, -0.6427681459581293666 ) ) ;
#44004 = CARTESIAN_POINT ( 'NONE',  ( -21.96455284011576836, 19.88594039843075834, -4.412914656511901512 ) ) ;
#44006 = AXIS2_PLACEMENT_3D ( 'NONE', #51171, #42085, #12287 ) ;
#44005 = DIRECTION ( 'NONE',  ( 0.000000000000000000, -0.000000000000000000, -1.000000000000000000 ) ) ;
#44007 = VECTOR ( 'NONE', #12525, 1000.000000000000227 ) ;
#44009 = CARTESIAN_POINT ( 'NONE',  ( -13.53673582514181106, 0.000000000000000000, 12.22817484722816772 ) ) ;
#44008 = AXIS2_PLACEMENT_3D ( 'NONE', #8103, #39312, #25410 ) ;
#44010 = ORIENTED_EDGE ( 'NONE', *, *, #23577, .T. ) ;
#44011 = CARTESIAN_POINT ( 'NONE',  ( -16.26609195874202385, 0.000000000000000000, 4.693820636760064779 ) ) ;
#44012 = CARTESIAN_POINT ( 'NONE',  ( -14.20280369269832832, 0.000000000000000000, 12.40765738797303719 ) ) ;
#44013 = LINE ( 'NONE', #18448, #39943 ) ;
#44015 = VECTOR ( 'NONE', #19783, 999.9999999999998863 ) ;
#44014 = LINE ( 'NONE', #18449, #14205 ) ;
#44016 = AXIS2_PLACEMENT_3D ( 'NONE', #18412, #35454, #22960 ) ;
#44017 = DIRECTION ( 'NONE',  ( 0.005961354470445682716, -0.6427876096865404731, -0.7660212471507180654 ) ) ;
#44018 = EDGE_CURVE ( 'NONE', #9219, #46158, #2389, .T. ) ;
#44019 = DIRECTION ( 'NONE',  ( -0.005002170337468016433, -0.7660444431189770143, 0.6427681459581293666 ) ) ;
#44020 = CARTESIAN_POINT ( 'NONE',  ( -10.41586642886556824, 0.000000000000000000, 3.462026221559915129 ) ) ;
#44021 = ORIENTED_EDGE ( 'NONE', *, *, #25804, .F. ) ;
#44022 = AXIS2_PLACEMENT_3D ( 'NONE', #35252, #30426, #26161 ) ;
#44023 = AXIS2_PLACEMENT_3D ( 'NONE', #9510, #44692, #5265 ) ;
#44024 = ORIENTED_EDGE ( 'NONE', *, *, #47449, .T. ) ;
#44025 = EDGE_CURVE ( 'NONE', #33489, #22565, #37040, .T. ) ;
#44026 = LINE ( 'NONE', #35496, #15990 ) ;
#44027 = LINE ( 'NONE', #53396, #24989 ) ;
#44028 = ORIENTED_EDGE ( 'NONE', *, *, #18134, .F. ) ;
#44029 = DIRECTION ( 'NONE',  ( -1.000000000000000000, 0.000000000000000000, 0.000000000000000000 ) ) ;
#44030 = EDGE_CURVE ( 'NONE', #11534, #32995, #54343, .T. ) ;
#44031 = EDGE_LOOP ( 'NONE', ( #1338, #50684, #31048, #34187 ) ) ;
#44032 = DIRECTION ( 'NONE',  ( 0.9999697198139515519, 0.000000000000000000, 0.007781995580013368816 ) ) ;
#44033 = VECTOR ( 'NONE', #39778, 999.9999999999998863 ) ;
#44034 = ORIENTED_EDGE ( 'NONE', *, *, #30414, .T. ) ;
#44035 = ORIENTED_EDGE ( 'NONE', *, *, #24727, .F. ) ;
#44036 = ORIENTED_EDGE ( 'NONE', *, *, #16582, .F. ) ;
#44037 = TOROIDAL_SURFACE ( 'NONE', #15899, 2.750000000000006217, 1.000000000000000000 ) ;
#44038 = DIRECTION ( 'NONE',  ( -0.5364919789714478471, 0.6444004775717705469, -0.5449076811759709926 ) ) ;
#44039 = CARTESIAN_POINT ( 'NONE',  ( -6.777710503706796175, -6.513112611849074085, -0.5856806440065189800 ) ) ;
#44040 = AXIS2_PLACEMENT_3D ( 'NONE', #56159, #4216, #51613 ) ;
#44041 = DIRECTION ( 'NONE',  ( 0.9999697198139515519, 0.000000000000000000, 0.007781995580013368816 ) ) ;
#44042 = DIRECTION ( 'NONE',  ( -0.005002170337468016433, -0.7660444431189770143, 0.6427681459581293666 ) ) ;
#44043 = ORIENTED_EDGE ( 'NONE', *, *, #26490, .F. ) ;
#44044 = VECTOR ( 'NONE', #2577, 1000.000000000000227 ) ;
#44045 = ORIENTED_EDGE ( 'NONE', *, *, #28296, .T. ) ;
#44046 = EDGE_CURVE ( 'NONE', #24636, #39671, #49246, .T. ) ;
#44047 = VECTOR ( 'NONE', #13129, 1000.000000000000227 ) ;
#44048 = VECTOR ( 'NONE', #41327, 1000.000000000000227 ) ;
#44049 = LINE ( 'NONE', #40057, #7323 ) ;
#44050 = ORIENTED_EDGE ( 'NONE', *, *, #13746, .T. ) ;
#44051 = FACE_OUTER_BOUND ( 'NONE', #39381, .T. ) ;
#44052 = ADVANCED_FACE ( 'NONE', ( #19974 ), #24259, .F. ) ;
#44053 = ORIENTED_EDGE ( 'NONE', *, *, #28812, .F. ) ;
#44054 = DIRECTION ( 'NONE',  ( 0.000000000000000000, -0.000000000000000000, -1.000000000000000000 ) ) ;
#44055 = DIRECTION ( 'NONE',  ( -0.9999697198139514409, -0.000000000000000000, -0.007781995580013368816 ) ) ;
#44056 = VECTOR ( 'NONE', #24801, 1000.000000000000114 ) ;
#44057 = VERTEX_POINT ( 'NONE', #15712 ) ;
#44058 = AXIS2_PLACEMENT_3D ( 'NONE', #55033, #53888, #36580 ) ;
#44059 = EDGE_CURVE ( 'NONE', #36108, #27112, #33049, .T. ) ;
#44060 = LINE ( 'NONE', #53679, #10509 ) ;
#44061 = VECTOR ( 'NONE', #23824, 1000.000000000000227 ) ;
#44062 = ORIENTED_EDGE ( 'NONE', *, *, #14006, .F. ) ;
#44063 = EDGE_CURVE ( 'NONE', #31769, #23301, #5820, .T. ) ;
#44064 = VECTOR ( 'NONE', #25389, 1000.000000000000227 ) ;
#44065 = FACE_OUTER_BOUND ( 'NONE', #38320, .T. ) ;
#44066 = VECTOR ( 'NONE', #50282, 1000.000000000000227 ) ;
#44067 = EDGE_LOOP ( 'NONE', ( #8548, #12042, #11882, #120, #18700 ) ) ;
#44068 = PLANE ( 'NONE',  #34900 ) ;
#44069 = DIRECTION ( 'NONE',  ( 0.005002170337468016433, -0.7660444431189770143, -0.6427681459581293666 ) ) ;
#44070 = FACE_OUTER_BOUND ( 'NONE', #14232, .T. ) ;
#44071 = ORIENTED_EDGE ( 'NONE', *, *, #18306, .F. ) ;
#44072 = DIRECTION ( 'NONE',  ( -0.6246952433987893460, -0.7422098413412802076, 0.2426528472758542054 ) ) ;
#44073 = FACE_OUTER_BOUND ( 'NONE', #17883, .T. ) ;
#44074 = DIRECTION ( 'NONE',  ( -0.005002170337468016433, -0.7660444431189770143, 0.6427681459581293666 ) ) ;
#44075 = CARTESIAN_POINT ( 'NONE',  ( -60.74376512051347277, 7.691826835550698682, 2.999999999999993339 ) ) ;
#44076 = CARTESIAN_POINT ( 'NONE',  ( -12.13851405436063047, 0.000000000000000000, 11.68505802764555135 ) ) ;
#44077 = DIRECTION ( 'NONE',  ( -0.6246952433987894571, 0.7422098413412802076, 0.2426528472758539834 ) ) ;
#44078 = VECTOR ( 'NONE', #36343, 1000.000000000000114 ) ;
#44079 = EDGE_CURVE ( 'NONE', #93, #49846, #7476, .T. ) ;
#44080 = FACE_OUTER_BOUND ( 'NONE', #27432, .T. ) ;
#44081 = EDGE_LOOP ( 'NONE', ( #52156, #35639, #43078, #19831 ) ) ;
#44082 = DIRECTION ( 'NONE',  ( 0.000000000000000000, -0.000000000000000000, -1.000000000000000000 ) ) ;
#44083 = DIRECTION ( 'NONE',  ( -0.005961354470445682716, -0.6427876096865404731, 0.7660212471507180654 ) ) ;
#44084 = CARTESIAN_POINT ( 'NONE',  ( -16.33317936670417225, 0.000000000000000000, 13.31440848639340224 ) ) ;
#44085 = ORIENTED_EDGE ( 'NONE', *, *, #5531, .F. ) ;
#44086 = DIRECTION ( 'NONE',  ( -0.005961354470445682716, -0.6427876096865404731, 0.7660212471507180654 ) ) ;
#44087 = DIRECTION ( 'NONE',  ( 0.9999697198139515519, 0.000000000000000000, 0.007781995580013368816 ) ) ;
#44088 = VECTOR ( 'NONE', #12002, 999.9999999999998863 ) ;
#44089 = EDGE_LOOP ( 'NONE', ( #54505, #40841, #543, #31829 ) ) ;
#44090 = DIRECTION ( 'NONE',  ( 0.000000000000000000, 0.000000000000000000, 1.000000000000000000 ) ) ;
#44091 = DIRECTION ( 'NONE',  ( -0.6246952433987893460, -0.7422098413412802076, 0.2426528472758542054 ) ) ;
#44092 = AXIS2_PLACEMENT_3D ( 'NONE', #11608, #28928, #24641 ) ;
#44093 = CARTESIAN_POINT ( 'NONE',  ( -13.63673279712320507, -0.1191753592594197858, 12.22739664767016521 ) ) ;
#44094 = CARTESIAN_POINT ( 'NONE',  ( -15.86710544311044302, 0.000000000000000000, 13.13336954653252953 ) ) ;
#44095 = ORIENTED_EDGE ( 'NONE', *, *, #3961, .T. ) ;
#44096 = VECTOR ( 'NONE', #50770, 999.9999999999998863 ) ;
#44097 = AXIS2_PLACEMENT_3D ( 'NONE', #23592, #15354, #41733 ) ;
#44098 = VERTEX_POINT ( 'NONE', #47995 ) ;
#44099 = CARTESIAN_POINT ( 'NONE',  ( -56.75000000000000711, 4.550000000000001599, -2.449489742783172108 ) ) ;
#44100 = DIRECTION ( 'NONE',  ( 0.9999697198139515519, 0.000000000000000000, 0.007781995580013368816 ) ) ;
#44101 = CARTESIAN_POINT ( 'NONE',  ( -66.29759486836289284, 1.999999999999978462, 5.111569279459581061 ) ) ;
#44102 = AXIS2_PLACEMENT_3D ( 'NONE', #6700, #50691, #24015 ) ;
#44103 = DIRECTION ( 'NONE',  ( -0.6427681459581293666, -0.7660444431189770143, -0.005002170337467561935 ) ) ;
#44105 = DIRECTION ( 'NONE',  ( 0.5449076811759707706, 0.6444004775717708799, -0.5364919789714476250 ) ) ;
#44104 = VECTOR ( 'NONE', #47000, 1000.000000000000114 ) ;
#44106 = DIRECTION ( 'NONE',  ( 0.005961354470445682716, -0.6427876096865404731, -0.7660212471507180654 ) ) ;
#44107 = EDGE_CURVE ( 'NONE', #55375, #38787, #12321, .T. ) ;
#44108 = ORIENTED_EDGE ( 'NONE', *, *, #1013, .T. ) ;
#44109 = DIRECTION ( 'NONE',  ( 0.7660212471507180654, -0.6427876096865404731, 0.005961354470445141482 ) ) ;
#44110 = VECTOR ( 'NONE', #13106, 999.9999999999998863 ) ;
#44111 = AXIS2_PLACEMENT_3D ( 'NONE', #33890, #20560, #32758 ) ;
#44112 = LINE ( 'NONE', #55765, #12448 ) ;
#44113 = ORIENTED_EDGE ( 'NONE', *, *, #39323, .F. ) ;
#44114 = DIRECTION ( 'NONE',  ( -0.3620778797217456546, 0.000000000000000000, -0.9321478471874540261 ) ) ;
#44115 = LINE ( 'NONE', #48662, #31343 ) ;
#44116 = DIRECTION ( 'NONE',  ( 0.6427681459581294776, -0.7660444431189769032, 0.005002170337467562802 ) ) ;
#44117 = EDGE_CURVE ( 'NONE', #55206, #26525, #52268, .T. ) ;
#44118 = ORIENTED_EDGE ( 'NONE', *, *, #11973, .F. ) ;
#44119 = DIRECTION ( 'NONE',  ( 0.9999697198139515519, 0.000000000000000000, 0.007781995580013368816 ) ) ;
#44120 = ORIENTED_EDGE ( 'NONE', *, *, #43402, .T. ) ;
#44121 = EDGE_CURVE ( 'NONE', #48671, #52431, #46362, .T. ) ;
#44122 = EDGE_CURVE ( 'NONE', #51697, #15737, #55452, .T. ) ;
#44123 = VECTOR ( 'NONE', #17053, 999.9999999999998863 ) ;
#44124 = VERTEX_POINT ( 'NONE', #24510 ) ;
#44125 = ORIENTED_EDGE ( 'NONE', *, *, #47268, .F. ) ;
#44126 = ORIENTED_EDGE ( 'NONE', *, *, #28786, .T. ) ;
#44127 = CARTESIAN_POINT ( 'NONE',  ( -13.95596008767372709, 0.000000000000000000, 6.389132952593959303 ) ) ;
#44128 = PRODUCT_DEFINITION_SHAPE ( 'NONE', 'NONE',  #56239 ) ;
#44129 = ADVANCED_FACE ( 'NONE', ( #37883 ), #25109, .F. ) ;
#44130 = VECTOR ( 'NONE', #22515, 1000.000000000000114 ) ;
#44131 = VERTEX_POINT ( 'NONE', #16276 ) ;
#44132 = DIRECTION ( 'NONE',  ( -0.05705673239519651330, 0.9983709377222391712, 2.351258244848514932E-16 ) ) ;
#44133 = DIRECTION ( 'NONE',  ( -0.4165485852472818884, -0.02380568209675183733, -0.9088017196442776946 ) ) ;
#44134 = ORIENTED_EDGE ( 'NONE', *, *, #41993, .F. ) ;
#44135 = LINE ( 'NONE', #18010, #24096 ) ;
#44136 = EDGE_CURVE ( 'NONE', #1292, #31910, #42419, .T. ) ;
#44137 = VECTOR ( 'NONE', #7226, 1000.000000000000114 ) ;
#44138 = EDGE_LOOP ( 'NONE', ( #54887, #11356, #9073, #3867, #46304 ) ) ;
#44139 = DIRECTION ( 'NONE',  ( 0.005002170337468016433, -0.7660444431189770143, -0.6427681459581293666 ) ) ;
#44140 = ORIENTED_EDGE ( 'NONE', *, *, #42803, .F. ) ;
#44141 = EDGE_CURVE ( 'NONE', #12681, #12998, #51206, .T. ) ;
#44142 = VECTOR ( 'NONE', #32565, 999.9999999999998863 ) ;
#44143 = DIRECTION ( 'NONE',  ( 0.007781995580012662783, 0.000000000000000000, -0.9999697198139514409 ) ) ;
#44144 = LINE ( 'NONE', #31361, #28384 ) ;
#44145 = CARTESIAN_POINT ( 'NONE',  ( 3.004435629306332345, -1.000000000000000000, -3.312607213261892003 ) ) ;
#44146 = LINE ( 'NONE', #5255, #31167 ) ;
#44147 = LINE ( 'NONE', #13743, #45053 ) ;
#44148 = DIRECTION ( 'NONE',  ( -0.5364919789714478471, 0.6444004775717705469, -0.5449076811759709926 ) ) ;
#44149 = ORIENTED_EDGE ( 'NONE', *, *, #32131, .F. ) ;
#44150 = EDGE_CURVE ( 'NONE', #26242, #52494, #4833, .T. ) ;
#44151 = ORIENTED_EDGE ( 'NONE', *, *, #17573, .T. ) ;
#44152 = VECTOR ( 'NONE', #14410, 1000.000000000000227 ) ;
#44153 = DIRECTION ( 'NONE',  ( -0.6427681459581293666, -0.7660444431189770143, -0.005002170337467561935 ) ) ;
#44154 = CARTESIAN_POINT ( 'NONE',  ( -25.20123094555300369, 0.000000000000000000, 6.470945668149052032 ) ) ;
#44155 = VECTOR ( 'NONE', #43149, 1000.000000000000227 ) ;
#44156 = DIRECTION ( 'NONE',  ( 0.005002170337468016433, -0.7660444431189770143, -0.6427681459581293666 ) ) ;
#44157 = EDGE_CURVE ( 'NONE', #38693, #10700, #39490, .T. ) ;
#44158 = VECTOR ( 'NONE', #850, 999.9999999999998863 ) ;
#44159 = CARTESIAN_POINT ( 'NONE',  ( -18.59945500257930107, 0.000000000000000000, 5.983664131656099450 ) ) ;
#44160 = ORIENTED_EDGE ( 'NONE', *, *, #47577, .T. ) ;
#44161 = CARTESIAN_POINT ( 'NONE',  ( -11.20636620717317378, 0.000000000000000000, 11.32298014792380414 ) ) ;
#44162 = CARTESIAN_POINT ( 'NONE',  ( -25.20278734466900517, 0.000000000000000000, 6.670939612111840944 ) ) ;
#44163 = VERTEX_POINT ( 'NONE', #26148 ) ;
#44164 = LINE ( 'NONE', #48114, #41095 ) ;
#44165 = CARTESIAN_POINT ( 'NONE',  ( -22.40478740399063895, 0.000000000000000000, 5.384712028983816623 ) ) ;
#44166 = EDGE_LOOP ( 'NONE', ( #109, #47244, #12031, #29540 ) ) ;
#44167 = CARTESIAN_POINT ( 'NONE',  ( -66.57154759241068120, -8.723685910846755931, -0.6652792357935665146 ) ) ;
#44168 = DIRECTION ( 'NONE',  ( 0.007781995580012663651, 0.000000000000000000, -0.9999697198139515519 ) ) ;
#44169 = PLANE ( 'NONE',  #25009 ) ;
#44170 = DIRECTION ( 'NONE',  ( -0.6427681459581293666, -0.7660444431189770143, -0.005002170337467561935 ) ) ;
#44171 = AXIS2_PLACEMENT_3D ( 'NONE', #52311, #34995, #13413 ) ;
#44172 = PLANE ( 'NONE',  #13843 ) ;
#44173 = ORIENTED_EDGE ( 'NONE', *, *, #15089, .F. ) ;
#44174 = ORIENTED_EDGE ( 'NONE', *, *, #54315, .T. ) ;
#44175 = CARTESIAN_POINT ( 'NONE',  ( -12.63252763452103800, -0.1191753592594188005, 2.606108483780943619 ) ) ;
#44176 = FACE_OUTER_BOUND ( 'NONE', #2293, .T. ) ;
#44177 = CARTESIAN_POINT ( 'NONE',  ( -23.33849165029409889, 0.000000000000000000, 5.946783852668351855 ) ) ;
#44178 = CARTESIAN_POINT ( 'NONE',  ( -12.54037462349748822, 0.000000000000000000, 3.614818821130846072 ) ) ;
#44179 = AXIS2_PLACEMENT_3D ( 'NONE', #52895, #49188, #48659 ) ;
#44180 = CARTESIAN_POINT ( 'NONE',  ( -16.85449645516476380, -0.1191753592594192307, 7.743901123477560766 ) ) ;
#44181 = ADVANCED_FACE ( 'NONE', ( #35238 ), #29060, .F. ) ;
#44182 = VERTEX_POINT ( 'NONE', #7211 ) ;
#44183 = CARTESIAN_POINT ( 'NONE',  ( -17.65907840528382522, 22.46280217494961562, -4.109392642200513812 ) ) ;
#44184 = DIRECTION ( 'NONE',  ( -0.9999697198139514409, -0.000000000000000000, -0.007781995580013368816 ) ) ;
#44186 = VECTOR ( 'NONE', #4979, 1000.000000000000114 ) ;
#44185 = FACE_OUTER_BOUND ( 'NONE', #27413, .T. ) ;
#44187 = DIRECTION ( 'NONE',  ( 0.000000000000000000, -0.000000000000000000, -1.000000000000000000 ) ) ;
#44188 = ORIENTED_EDGE ( 'NONE', *, *, #6603, .T. ) ;
#44189 = FACE_OUTER_BOUND ( 'NONE', #32097, .T. ) ;
#44190 = ORIENTED_EDGE ( 'NONE', *, *, #17735, .F. ) ;
#44191 = DIRECTION ( 'NONE',  ( 0.6427681459581294776, -0.7660444431189769032, 0.005002170337467562802 ) ) ;
#44192 = EDGE_CURVE ( 'NONE', #20216, #40878, #34955, .T. ) ;
#44193 = ADVANCED_FACE ( 'NONE', ( #39184 ), #12009, .F. ) ;
#44194 = PLANE ( 'NONE',  #4856 ) ;
#44195 = EDGE_CURVE ( 'NONE', #24619, #16314, #29348, .T. ) ;
#44196 = ORIENTED_EDGE ( 'NONE', *, *, #25394, .T. ) ;
#44197 = VECTOR ( 'NONE', #15179, 1000.000000000000000 ) ;
#44198 = DIRECTION ( 'NONE',  ( 0.9999697198139515519, 0.000000000000000000, 0.007781995580013368816 ) ) ;
#44199 = ORIENTED_EDGE ( 'NONE', *, *, #10714, .T. ) ;
#44200 = EDGE_CURVE ( 'NONE', #29572, #1220, #17914, .T. ) ;
#44201 = VERTEX_POINT ( 'NONE', #46104 ) ;
#44202 = ORIENTED_EDGE ( 'NONE', *, *, #49637, .T. ) ;
#44203 = LINE ( 'NONE', #52689, #15755 ) ;
#44204 = ORIENTED_EDGE ( 'NONE', *, *, #29286, .F. ) ;
#44205 = VERTEX_POINT ( 'NONE', #41827 ) ;
#44206 = CARTESIAN_POINT ( 'NONE',  ( -15.00457102831626699, -0.1191753592594181482, 8.866293880322892562 ) ) ;
#44207 = DIRECTION ( 'NONE',  ( -0.5364919789714478471, 0.6444004775717705469, -0.5449076811759709926 ) ) ;
#44208 = ORIENTED_EDGE ( 'NONE', *, *, #49122, .T. ) ;
#44209 = ORIENTED_EDGE ( 'NONE', *, *, #9060, .F. ) ;
#44210 = DIRECTION ( 'NONE',  ( 0.9999697198139515519, 0.000000000000000000, 0.007781995580013368816 ) ) ;
#44211 = ADVANCED_FACE ( 'NONE', ( #2917 ), #54911, .F. ) ;
#44212 = ORIENTED_EDGE ( 'NONE', *, *, #41079, .T. ) ;
#44213 = ORIENTED_EDGE ( 'NONE', *, *, #48767, .F. ) ;
#44214 = ADVANCED_FACE ( 'NONE', ( #36335 ), #5974, .F. ) ;
#44215 = DIRECTION ( 'NONE',  ( 0.9999697198139515519, 0.000000000000000000, 0.007781995580013368816 ) ) ;
#44216 = DIRECTION ( 'NONE',  ( -0.000000000000000000, -0.000000000000000000, 1.000000000000000000 ) ) ;
#44217 = ADVANCED_FACE ( 'NONE', ( #1690 ), #13906, .F. ) ;
#44218 = DIRECTION ( 'NONE',  ( 0.5364919789714477361, 0.6444004775717706579, 0.5449076811759711036 ) ) ;
#44219 = LINE ( 'NONE', #5319, #38634 ) ;
#44220 = VERTEX_POINT ( 'NONE', #48253 ) ;
#44221 = CARTESIAN_POINT ( 'NONE',  ( -14.32071356977549925, -5.375054281893163477, 11.06596300975003544 ) ) ;
#44222 = ORIENTED_EDGE ( 'NONE', *, *, #2855, .F. ) ;
#44223 = EDGE_CURVE ( 'NONE', #15160, #14352, #19015, .T. ) ;
#44224 = DIRECTION ( 'NONE',  ( -0.7660212471507179544, -0.6427876096865405842, -0.005961354470445141482 ) ) ;
#44225 = PLANE ( 'NONE',  #30625 ) ;
#44226 = VECTOR ( 'NONE', #34264, 1000.000000000000227 ) ;
#44227 = PLANE ( 'NONE',  #54910 ) ;
#44228 = DIRECTION ( 'NONE',  ( 0.9999697198139515519, 0.000000000000000000, 0.007781995580013368816 ) ) ;
#44229 = CARTESIAN_POINT ( 'NONE',  ( 5.283701512688073976, -1.082329719221734932, -2.393429442024904485 ) ) ;
#44230 = CARTESIAN_POINT ( 'NONE',  ( -5.059434328074208231, -6.953069894654446692, 5.183629687800835661 ) ) ;
#44231 = DIRECTION ( 'NONE',  ( 0.007781995580012663651, -3.146120232559066537E-19, -0.9999697198139514409 ) ) ;
#44232 = ORIENTED_EDGE ( 'NONE', *, *, #40668, .F. ) ;
#44233 = CARTESIAN_POINT ( 'NONE',  ( -16.99924723426068951, 0.000000000000000000, 13.49389102713827171 ) ) ;
#44234 = VECTOR ( 'NONE', #44920, 1000.000000000000000 ) ;
#44235 = DIRECTION ( 'NONE',  ( 0.000000000000000000, -1.000000000000000000, 0.000000000000000000 ) ) ;
#44236 = DIRECTION ( 'NONE',  ( 0.005002170337468016433, -0.7660444431189770143, -0.6427681459581293666 ) ) ;
#44237 = DIRECTION ( 'NONE',  ( 0.007781995580012663651, 0.000000000000000000, -0.9999697198139515519 ) ) ;
#44238 = CARTESIAN_POINT ( 'NONE',  ( -19.81260243149071698, 19.48741369114385691, -4.324310068654933836 ) ) ;
#44239 = PLANE ( 'NONE',  #47631 ) ;
#44240 = DIRECTION ( 'NONE',  ( 0.007781995580012663651, 0.000000000000000000, -0.9999697198139515519 ) ) ;
#44241 = DIRECTION ( 'NONE',  ( 0.007781995580012663651, 0.000000000000000000, -0.9999697198139515519 ) ) ;
#44242 = VERTEX_POINT ( 'NONE', #19278 ) ;
#44243 = LINE ( 'NONE', #26624, #8481 ) ;
#44244 = CARTESIAN_POINT ( 'NONE',  ( -18.19297601772640860, 2.067327705546506689, 3.682742875386304515 ) ) ;
#44245 = CARTESIAN_POINT ( 'NONE',  ( -18.36880263084326259, 0.000000000000000000, 10.35344032464643149 ) ) ;
#44246 = EDGE_CURVE ( 'NONE', #43064, #32693, #36618, .T. ) ;
#44247 = CARTESIAN_POINT ( 'NONE',  ( -69.33845141029836157, 1.348542913706229918, -7.487543234984622487 ) ) ;
#44248 = CARTESIAN_POINT ( 'NONE',  ( -8.875996589204540044, 0.000000000000000000, 10.41778544861944233 ) ) ;
#44249 = EDGE_CURVE ( 'NONE', #24292, #33398, #27840, .T. ) ;
#44250 = CARTESIAN_POINT ( 'NONE',  ( -18.12906999872765113, 0.000000000000000000, 5.248660636908578425 ) ) ;
#44251 = LINE ( 'NONE', #5354, #37386 ) ;
#44252 = CARTESIAN_POINT ( 'NONE',  ( -67.98277075215574428, -9.624319141569721126, 5.224814904089846834 ) ) ;
#44253 = LINE ( 'NONE', #9311, #2940 ) ;
#44254 = EDGE_CURVE ( 'NONE', #33081, #23263, #32082, .T. ) ;
#44255 = EDGE_CURVE ( 'NONE', #563, #55181, #49398, .T. ) ;
#44256 = EDGE_CURVE ( 'NONE', #38231, #40790, #44856, .T. ) ;
#44257 = EDGE_LOOP ( 'NONE', ( #8358, #8291, #47343, #54202, #26883 ) ) ;
#44258 = EDGE_CURVE ( 'NONE', #37328, #37239, #40028, .T. ) ;
#44259 = ORIENTED_EDGE ( 'NONE', *, *, #36917, .F. ) ;
#44260 = ORIENTED_EDGE ( 'NONE', *, *, #51737, .T. ) ;
#44261 = VERTEX_POINT ( 'NONE', #23556 ) ;
#44262 = ORIENTED_EDGE ( 'NONE', *, *, #10021, .F. ) ;
#44263 = CARTESIAN_POINT ( 'NONE',  ( -14.85649334630307017, 0.000000000000000000, 2.688804096480295502 ) ) ;
#44264 = CARTESIAN_POINT ( 'NONE',  ( -19.71722652620312743, 0.000000000000000000, 4.497637095973019861 ) ) ;
#44265 = VECTOR ( 'NONE', #39890, 999.9999999999998863 ) ;
#44266 = ORIENTED_EDGE ( 'NONE', *, *, #22498, .T. ) ;
#44267 = VERTEX_POINT ( 'NONE', #40318 ) ;
#44268 = EDGE_CURVE ( 'NONE', #25423, #33543, #9946, .T. ) ;
#44269 = EDGE_CURVE ( 'NONE', #41178, #50871, #39768, .T. ) ;
#44270 = CARTESIAN_POINT ( 'NONE',  ( -67.31341032591832629, -9.413710574012958077, -5.859509639694563177 ) ) ;
#44271 = ORIENTED_EDGE ( 'NONE', *, *, #9586, .F. ) ;
#44272 = EDGE_CURVE ( 'NONE', #22478, #27583, #44560, .T. ) ;
#44273 = CARTESIAN_POINT ( 'NONE',  ( -29.86352658060627618, 0.000000000000000000, 8.481329010720569883 ) ) ;
#44274 = CARTESIAN_POINT ( 'NONE',  ( -14.42347103802009300, 0.000000000000000000, 6.754826744083713308 ) ) ;
#44275 = VERTEX_POINT ( 'NONE', #30943 ) ;
#44276 = CARTESIAN_POINT ( 'NONE',  ( -10.90349575374891700, 0.000000000000000000, 6.412887935854022281 ) ) ;
#44277 = EDGE_LOOP ( 'NONE', ( #55029, #46135, #44991, #39926 ) ) ;
#44278 = EDGE_CURVE ( 'NONE', #52907, #33376, #44014, .T. ) ;
#44279 = PLANE ( 'NONE',  #49995 ) ;
#44280 = CARTESIAN_POINT ( 'NONE',  ( -23.33693525117809386, 0.000000000000000000, 5.746789908705562944 ) ) ;
#44281 = ADVANCED_FACE ( 'NONE', ( #31235 ), #22460, .F. ) ;
#44282 = CARTESIAN_POINT ( 'NONE',  ( -13.19638330378551316, 0.000000000000000000, 2.501717400473541186 ) ) ;
#44283 = LINE ( 'NONE', #14194, #2426 ) ;
#44284 = ORIENTED_EDGE ( 'NONE', *, *, #22365, .F. ) ;
#44285 = LINE ( 'NONE', #5113, #53930 ) ;
#44286 = DIRECTION ( 'NONE',  ( -0.5364919789714478471, 0.6444004775717705469, -0.5449076811759709926 ) ) ;
#44287 = DIRECTION ( 'NONE',  ( 0.6427681459581294776, -0.7660444431189769032, 0.005002170337467562802 ) ) ;
#44288 = EDGE_LOOP ( 'NONE', ( #4802, #26850, #20398, #48958 ) ) ;
#44289 = CARTESIAN_POINT ( 'NONE',  ( -16.33317936670417225, 0.000000000000000000, 13.31440848639340224 ) ) ;
#44290 = EDGE_LOOP ( 'NONE', ( #29022, #1822, #17165, #36715 ) ) ;
#44291 = CARTESIAN_POINT ( 'NONE',  ( -16.27052241136330579, 0.000000000000000000, 5.263124283980618046 ) ) ;
#44292 = LINE ( 'NONE', #834, #6968 ) ;
#44293 = LINE ( 'NONE', #13615, #8582 ) ;
#44294 = FACE_OUTER_BOUND ( 'NONE', #7246, .T. ) ;
#44295 = CARTESIAN_POINT ( 'NONE',  ( -14.00280974873554030, 0.000000000000000000, 12.40921378708904044 ) ) ;
#44296 = CARTESIAN_POINT ( 'NONE',  ( -6.110905869600904872, 1.712176620043476140E-14, 3.600000000000000089 ) ) ;
#44297 = FACE_OUTER_BOUND ( 'NONE', #11827, .T. ) ;
#44298 = DIRECTION ( 'NONE',  ( 0.007781995580012663651, 0.000000000000000000, -0.9999697198139515519 ) ) ;
#44299 = CARTESIAN_POINT ( 'NONE',  ( -10.70481946417540797, 0.000000000000000000, 6.583760094264999196 ) ) ;
#44300 = EDGE_LOOP ( 'NONE', ( #49957, #21434, #38610, #14933 ) ) ;
#44301 = LINE ( 'NONE', #26689, #16656 ) ;
#44302 = DIRECTION ( 'NONE',  ( 0.2113248654051873565, 0.7886751345948121994, -0.5773502691896263972 ) ) ;
#44303 = DIRECTION ( 'NONE',  ( 0.5364919789714477361, 0.6444004775717706579, 0.5449076811759711036 ) ) ;
#44304 = CARTESIAN_POINT ( 'NONE',  ( -13.10210881006539552, 0.4483081953215033444, 1.756932364226573728 ) ) ;
#44305 = FACE_OUTER_BOUND ( 'NONE', #35097, .T. ) ;
#44306 = PLANE ( 'NONE',  #47811 ) ;
#44307 = LINE ( 'NONE', #8849, #51934 ) ;
#44308 = VERTEX_POINT ( 'NONE', #18166 ) ;
#44309 = ORIENTED_EDGE ( 'NONE', *, *, #35419, .F. ) ;
#44310 = CARTESIAN_POINT ( 'NONE',  ( -12.65748011252205352, 1.581621852479007106, 1.548064839234879031 ) ) ;
#44311 = CARTESIAN_POINT ( 'NONE',  ( -20.17480658638558921, -5.213152330870665097, 4.551574281445605052 ) ) ;
#44312 = EDGE_CURVE ( 'NONE', #23289, #39974, #52798, .T. ) ;
#44313 = EDGE_LOOP ( 'NONE', ( #35600, #46953, #21668, #37218 ) ) ;
#44314 = CARTESIAN_POINT ( 'NONE',  ( -30.79567442779373110, 0.000000000000000000, 8.843406890442315316 ) ) ;
#44315 = ORIENTED_EDGE ( 'NONE', *, *, #15614, .F. ) ;
#44316 = CARTESIAN_POINT ( 'NONE',  ( -7.167951541316091024, 2.571841242220739510, 8.539956480301096775 ) ) ;
#44317 = EDGE_CURVE ( 'NONE', #18631, #49377, #9678, .T. ) ;
#44318 = EDGE_CURVE ( 'NONE', #24756, #53854, #22713, .T. ) ;
#44319 = ORIENTED_EDGE ( 'NONE', *, *, #52923, .F. ) ;
#44320 = EDGE_LOOP ( 'NONE', ( #457, #723, #40155, #46369 ) ) ;
#44321 = EDGE_LOOP ( 'NONE', ( #26043, #51466, #2889, #5433 ) ) ;
#44322 = LINE ( 'NONE', #48867, #23863 ) ;
#44323 = CYLINDRICAL_SURFACE ( 'NONE', #47727, 0.2499999999999998612 ) ;
#44324 = LINE ( 'NONE', #52823, #52971 ) ;
#44325 = CARTESIAN_POINT ( 'NONE',  ( -13.53673582514181106, 0.000000000000000000, 12.22817484722816772 ) ) ;
#44326 = ORIENTED_EDGE ( 'NONE', *, *, #11093, .F. ) ;
#44327 = ORIENTED_EDGE ( 'NONE', *, *, #20124, .F. ) ;
#44328 = CARTESIAN_POINT ( 'NONE',  ( 0.09621548157177368943, -1.683565401097097958, 2.124999999999999556 ) ) ;
#44329 = ORIENTED_EDGE ( 'NONE', *, *, #13028, .T. ) ;
#44330 = CARTESIAN_POINT ( 'NONE',  ( -16.94090135917774376, 0.000000000000000000, 5.996571379612134045 ) ) ;
#44331 = EDGE_LOOP ( 'NONE', ( #23611, #11773, #55234, #11709 ) ) ;
#44332 = PLANE ( 'NONE',  #55965 ) ;
#44333 = CARTESIAN_POINT ( 'NONE',  ( -9.293664452620451044, 0.000000000000000000, 4.378749610022443228 ) ) ;
#44334 =( GEOMETRIC_REPRESENTATION_CONTEXT ( 3 ) GLOBAL_UNCERTAINTY_ASSIGNED_CONTEXT ( ( #46721 ) ) GLOBAL_UNIT_ASSIGNED_CONTEXT ( ( #30108, #5968, #5398 ) ) REPRESENTATION_CONTEXT ( 'NONE', 'WORKASPACE' ) );
#44335 = ORIENTED_EDGE ( 'NONE', *, *, #45500, .T. ) ;
#44336 = DIRECTION ( 'NONE',  ( 0.5364919789714477361, 0.6444004775717706579, 0.5449076811759711036 ) ) ;
#44337 = ORIENTED_EDGE ( 'NONE', *, *, #45705, .F. ) ;
#44338 = EDGE_CURVE ( 'NONE', #3513, #34450, #50522, .T. ) ;
#44339 = FACE_OUTER_BOUND ( 'NONE', #9047, .T. ) ;
#44341 = EDGE_CURVE ( 'NONE', #34349, #661, #20404, .T. ) ;
#44340 = ORIENTED_EDGE ( 'NONE', *, *, #22336, .F. ) ;
#44342 = DIRECTION ( 'NONE',  ( 0.9999697198139515519, 0.000000000000000000, 0.007781995580013368816 ) ) ;
#44343 = CARTESIAN_POINT ( 'NONE',  ( -25.20123094555300369, 0.000000000000000000, 6.470945668149052032 ) ) ;
#44344 = LINE ( 'NONE', #49150, #42785 ) ;
#44345 = ADVANCED_FACE ( 'NONE', ( #7336 ), #6509, .F. ) ;
#44346 = ORIENTED_EDGE ( 'NONE', *, *, #19994, .T. ) ;
#44347 = DIRECTION ( 'NONE',  ( 0.7660212471507180654, -0.6427876096865404731, 0.005961354470445141482 ) ) ;
#44348 = EDGE_CURVE ( 'NONE', #35486, #26517, #28937, .T. ) ;
#44349 = LINE ( 'NONE', #9424, #4975 ) ;
#44350 = PLANE ( 'NONE',  #22295 ) ;
#44351 = DIRECTION ( 'NONE',  ( 0.005002170337468016433, -0.7660444431189770143, -0.6427681459581293666 ) ) ;
#44352 = CARTESIAN_POINT ( 'NONE',  ( -28.92982233430281980, 0.000000000000000000, 7.919257187036034651 ) ) ;
#44353 = CARTESIAN_POINT ( 'NONE',  ( -67.08121593252555215, -9.520946988596053373, 2.735910648343088614 ) ) ;
#44354 = EDGE_LOOP ( 'NONE', ( #10168, #7966, #18975, #49704 ) ) ;
#44355 = CARTESIAN_POINT ( 'NONE',  ( 2.072287782118878319, 0.000000000000000000, -2.950529333540147015 ) ) ;
#44356 = DIRECTION ( 'NONE',  ( -0.005961354470445682716, -0.6427876096865404731, 0.7660212471507180654 ) ) ;
#44357 = DIRECTION ( 'NONE',  ( 0.000000000000000000, 1.000000000000000000, 0.000000000000000000 ) ) ;
#44358 = VERTEX_POINT ( 'NONE', #33209 ) ;
#44359 = LINE ( 'NONE', #49742, #26593 ) ;
#44360 = FACE_OUTER_BOUND ( 'NONE', #47937, .T. ) ;
#44361 = ORIENTED_EDGE ( 'NONE', *, *, #32372, .T. ) ;
#44362 = DIRECTION ( 'NONE',  ( -0.7660212471507179544, -0.6427876096865405842, -0.005961354470445141482 ) ) ;
#44363 = CARTESIAN_POINT ( 'NONE',  ( 2.072287782118878319, 0.000000000000000000, -2.950529333540147015 ) ) ;
#44364 = CARTESIAN_POINT ( 'NONE',  ( -18.67775241435682432, 0.000000000000000000, 4.136394454059623804 ) ) ;
#44365 = LINE ( 'NONE', #18235, #50065 ) ;
#44366 = ORIENTED_EDGE ( 'NONE', *, *, #24806, .T. ) ;
#44367 = ORIENTED_EDGE ( 'NONE', *, *, #26869, .F. ) ;
#44368 = DIRECTION ( 'NONE',  ( 0.5449076811759707706, 0.6444004775717708799, -0.5364919789714476250 ) ) ;
#44369 = FACE_OUTER_BOUND ( 'NONE', #16510, .T. ) ;
#44370 = CARTESIAN_POINT ( 'NONE',  ( -23.33771345073609638, -0.1191753592594197858, 5.846786880686956955 ) ) ;
#44371 = ADVANCED_FACE ( 'NONE', ( #41693 ), #15046, .F. ) ;
#44372 = LINE ( 'NONE', #2021, #16639 ) ;
#44373 = EDGE_CURVE ( 'NONE', #3752, #36925, #23819, .T. ) ;
#44374 = LINE ( 'NONE', #31870, #174 ) ;
#44375 = FACE_OUTER_BOUND ( 'NONE', #44906, .T. ) ;
#44376 = EDGE_LOOP ( 'NONE', ( #30091, #42602, #11216, #8022 ) ) ;
#44377 = LINE ( 'NONE', #52893, #42865 ) ;
#44378 = EDGE_CURVE ( 'NONE', #2867, #11380, #16153, .T. ) ;
#44379 = EDGE_CURVE ( 'NONE', #30096, #26810, #15314, .T. ) ;
#44380 = FACE_OUTER_BOUND ( 'NONE', #30443, .T. ) ;
#44381 = ORIENTED_EDGE ( 'NONE', *, *, #34447, .F. ) ;
#44382 = DIRECTION ( 'NONE',  ( -0.005961354470445682716, -0.6427876096865404731, 0.7660212471507180654 ) ) ;
#44383 = DIRECTION ( 'NONE',  ( 0.000000000000000000, -0.000000000000000000, -1.000000000000000000 ) ) ;
#44384 = CARTESIAN_POINT ( 'NONE',  ( -12.13851405436063047, 0.000000000000000000, 11.68505802764555135 ) ) ;
#44385 = VERTEX_POINT ( 'NONE', #36916 ) ;
#44386 = CARTESIAN_POINT ( 'NONE',  ( -16.99924723426068951, 0.000000000000000000, 13.49389102713827171 ) ) ;
#44387 = VERTEX_POINT ( 'NONE', #32901 ) ;
#44388 = EDGE_CURVE ( 'NONE', #27005, #11058, #54216, .T. ) ;
#44389 = ORIENTED_EDGE ( 'NONE', *, *, #1165, .T. ) ;
#44390 = EDGE_LOOP ( 'NONE', ( #34827, #18579, #23861, #29515 ) ) ;
#44391 = ORIENTED_EDGE ( 'NONE', *, *, #12001, .F. ) ;
#44392 = CARTESIAN_POINT ( 'NONE',  ( -16.56028341318607389, 0.000000000000000000, 3.214202891609632129 ) ) ;
#44393 = EDGE_LOOP ( 'NONE', ( #4192, #52768, #23440, #15727 ) ) ;
#44394 = FACE_OUTER_BOUND ( 'NONE', #55790, .T. ) ;
#44395 = CARTESIAN_POINT ( 'NONE',  ( -9.958295293424326289, 0.000000000000000000, 4.373577299138431407 ) ) ;
#44396 = VERTEX_POINT ( 'NONE', #20103 ) ;
#44397 = CARTESIAN_POINT ( 'NONE',  ( -10.89199953972778623, 0.000000000000000000, 4.935649122822963974 ) ) ;
#44398 = ORIENTED_EDGE ( 'NONE', *, *, #47969, .F. ) ;
#44399 = CARTESIAN_POINT ( 'NONE',  ( -22.40478740399063895, 0.000000000000000000, 5.384712028983816623 ) ) ;
#44400 = ORIENTED_EDGE ( 'NONE', *, *, #53458, .F. ) ;
#44401 = CARTESIAN_POINT ( 'NONE',  ( -15.36268464660739141, 0.000000000000000000, 8.024839789615963781 ) ) ;
#44402 = CARTESIAN_POINT ( 'NONE',  ( -26.13493519185646008, 0.000000000000000000, 7.033017491833586377 ) ) ;
#44403 = DIRECTION ( 'NONE',  ( 0.005961354470445682716, -0.6427876096865404731, -0.7660212471507180654 ) ) ;
#44404 = DIRECTION ( 'NONE',  ( 0.000000000000000000, 0.000000000000000000, 1.000000000000000000 ) ) ;
#44405 = LINE ( 'NONE', #31063, #31435 ) ;
#44406 = LINE ( 'NONE', #40147, #6577 ) ;
#44407 = ORIENTED_EDGE ( 'NONE', *, *, #30229, .T. ) ;
#44408 = ORIENTED_EDGE ( 'NONE', *, *, #49905, .F. ) ;
#44409 = CARTESIAN_POINT ( 'NONE',  ( -25.25173380393689726, 18.07918053667318858, -4.578956201939200277 ) ) ;
#44410 = ADVANCED_FACE ( 'NONE', ( #53927 ), #11036, .F. ) ;
#44411 = CARTESIAN_POINT ( 'NONE',  ( -18.67619601524082285, 0.000000000000000000, 3.936400510096834893 ) ) ;
#44412 = DIRECTION ( 'NONE',  ( 0.005961354470445682716, -0.6427876096865404731, -0.7660212471507180654 ) ) ;
#44413 = DIRECTION ( 'NONE',  ( -0.5449076811759708816, 0.6444004775717707689, 0.5364919789714475140 ) ) ;
#44414 = VERTEX_POINT ( 'NONE', #24383 ) ;
#44415 = CARTESIAN_POINT ( 'NONE',  ( -10.74029228357944987, 0.000000000000000000, 11.14194120806293320 ) ) ;
#44416 = CARTESIAN_POINT ( 'NONE',  ( -70.05831411642593309, -0.4999789778861470357, -7.502972407220384277 ) ) ;
#44417 = EDGE_LOOP ( 'NONE', ( #22443, #3730, #15137, #49069 ) ) ;
#44418 = CARTESIAN_POINT ( 'NONE',  ( -25.20278734466900517, 0.000000000000000000, 6.670939612111840944 ) ) ;
#44419 = LINE ( 'NONE', #35630, #35826 ) ;
#44420 = ORIENTED_EDGE ( 'NONE', *, *, #37790, .T. ) ;
#44421 = EDGE_CURVE ( 'NONE', #16077, #15628, #28355, .T. ) ;
#44422 = CARTESIAN_POINT ( 'NONE',  ( -69.11683642851026832, -9.015837829197110409, 7.493101075386320531 ) ) ;
#44423 = CARTESIAN_POINT ( 'NONE',  ( -15.13495153988577968, 0.000000000000000000, 12.76973526769478084 ) ) ;
#44424 = CARTESIAN_POINT ( 'NONE',  ( -10.47421230394850866, 0.000000000000000000, 10.95934586908605723 ) ) ;
#44425 = ADVANCED_FACE ( 'NONE', ( #37167 ), #41150, .F. ) ;
#44426 = ADVANCED_FACE ( 'NONE', ( #41446 ), #19848, .F. ) ;
#44427 = FACE_OUTER_BOUND ( 'NONE', #53146, .T. ) ;
#44428 = CARTESIAN_POINT ( 'NONE',  ( -17.87436686075448122, 0.000000000000000000, 6.527965018628854033 ) ) ;
#44429 = ORIENTED_EDGE ( 'NONE', *, *, #25247, .F. ) ;
#44430 = ORIENTED_EDGE ( 'NONE', *, *, #15089, .T. ) ;
#44431 = PLANE ( 'NONE',  #55692 ) ;
#44432 = DIRECTION ( 'NONE',  ( -0.6427681459581293666, -0.7660444431189770143, -0.005002170337467561935 ) ) ;
#44433 = LINE ( 'NONE', #10369, #18814 ) ;
#44434 = ADVANCED_FACE ( 'NONE', ( #49599 ), #31977, .F. ) ;
#44435 = FACE_OUTER_BOUND ( 'NONE', #30784, .T. ) ;
#44436 = ADVANCED_FACE ( 'NONE', ( #15234 ), #48458, .F. ) ;
#44437 = CARTESIAN_POINT ( 'NONE',  ( -19.58350694149355675, 0.9340140483890049250, 6.021096448066252549 ) ) ;
#44438 = ORIENTED_EDGE ( 'NONE', *, *, #32406, .F. ) ;
#44439 = CARTESIAN_POINT ( 'NONE',  ( -13.98444087813280490, 24.58435514042456660, -3.686392358618231668 ) ) ;
#44440 = DIRECTION ( 'NONE',  ( 0.5364919789714477361, 0.6444004775717706579, 0.5449076811759711036 ) ) ;
#44441 = EDGE_CURVE ( 'NONE', #23769, #26810, #27164, .T. ) ;
#44442 = VECTOR ( 'NONE', #1879, 999.9999999999998863 ) ;
#44443 = CARTESIAN_POINT ( 'NONE',  ( -16.45458968868368288, 0.000000000000000000, 3.215025424613001892 ) ) ;
#44444 = FACE_OUTER_BOUND ( 'NONE', #34657, .T. ) ;
#44445 = ORIENTED_EDGE ( 'NONE', *, *, #35247, .F. ) ;
#44446 = LINE ( 'NONE', #19154, #50128 ) ;
#44447 = ORIENTED_EDGE ( 'NONE', *, *, #6963, .F. ) ;
#44448 = DIRECTION ( 'NONE',  ( 0.7660212471507180654, -0.6427876096865404731, 0.005961354470445141482 ) ) ;
#44449 = DIRECTION ( 'NONE',  ( 0.000000000000000000, -0.000000000000000000, -1.000000000000000000 ) ) ;
#44450 = EDGE_CURVE ( 'NONE', #27927, #36106, #28010, .T. ) ;
#44451 = ORIENTED_EDGE ( 'NONE', *, *, #6453, .F. ) ;
#44452 = LINE ( 'NONE', #5556, #35373 ) ;
#44453 = ORIENTED_EDGE ( 'NONE', *, *, #16540, .T. ) ;
#44454 = EDGE_CURVE ( 'NONE', #6528, #29959, #14658, .T. ) ;
#44455 = ORIENTED_EDGE ( 'NONE', *, *, #23438, .T. ) ;
#44456 = VERTEX_POINT ( 'NONE', #6169 ) ;
#44457 = CARTESIAN_POINT ( 'NONE',  ( -43.16120336687457382, 7.739143463467679673, 4.999999999999998224 ) ) ;
#44458 = VERTEX_POINT ( 'NONE', #23471 ) ;
#44459 = ORIENTED_EDGE ( 'NONE', *, *, #3718, .T. ) ;
#44460 = FACE_OUTER_BOUND ( 'NONE', #13859, .T. ) ;
#44461 = LINE ( 'NONE', #1006, #53941 ) ;
#44462 = ORIENTED_EDGE ( 'NONE', *, *, #31513, .T. ) ;
#44463 = EDGE_LOOP ( 'NONE', ( #50655, #6748, #14305 ) ) ;
#44464 = LINE ( 'NONE', #48156, #34933 ) ;
#44465 = ORIENTED_EDGE ( 'NONE', *, *, #29411, .T. ) ;
#44466 = ORIENTED_EDGE ( 'NONE', *, *, #52216, .F. ) ;
#44467 = PLANE ( 'NONE',  #20324 ) ;
#44468 = CARTESIAN_POINT ( 'NONE',  ( -11.20636620717317378, 0.000000000000000000, 11.32298014792380414 ) ) ;
#44469 = DIRECTION ( 'NONE',  ( 0.007781995580012663651, -3.146120232559066537E-19, -0.9999697198139514409 ) ) ;
#44470 = CARTESIAN_POINT ( 'NONE',  ( 1.710209902397132220, -1.000000000000000000, -3.882677180727601041 ) ) ;
#44471 = ORIENTED_EDGE ( 'NONE', *, *, #55712, .F. ) ;
#44472 = LINE ( 'NONE', #35691, #24640 ) ;
#44473 = EDGE_LOOP ( 'NONE', ( #41791, #20066, #35129, #55387 ) ) ;
#44474 = ADVANCED_FACE ( 'NONE', ( #9576 ), #23727, .F. ) ;
#44475 = LINE ( 'NONE', #22905, #28427 ) ;
#44476 = VECTOR ( 'NONE', #39258, 999.9999999999998863 ) ;
#44477 = LINE ( 'NONE', #48169, #55987 ) ;
#44478 = LINE ( 'NONE', #26603, #18645 ) ;
#44479 = PLANE ( 'NONE',  #2199 ) ;
#44480 = CARTESIAN_POINT ( 'NONE',  ( -9.676870672209137325, -1.212633296248882164, 2.080894224339388199 ) ) ;
#44481 = DIRECTION ( 'NONE',  ( -0.9999697198139514409, -0.000000000000000000, -0.007781995580013368816 ) ) ;
#44482 = ORIENTED_EDGE ( 'NONE', *, *, #4134, .F. ) ;
#44483 = CARTESIAN_POINT ( 'NONE',  ( -14.62633903548816328, 0.000000000000000000, 7.122580048225473526 ) ) ;
#44484 = ORIENTED_EDGE ( 'NONE', *, *, #28198, .F. ) ;
#44485 = DIRECTION ( 'NONE',  ( -0.9999697198139514409, -0.000000000000000000, -0.007781995580013368816 ) ) ;
#44486 = LINE ( 'NONE', #27179, #7875 ) ;
#44487 = DIRECTION ( 'NONE',  ( 0.007781995580012663651, -3.146120232559066537E-19, -0.9999697198139514409 ) ) ;
#44488 = CARTESIAN_POINT ( 'NONE',  ( -28.97056323743311523, 14.20006255460496547, -4.749095691681356257 ) ) ;
#44489 = CARTESIAN_POINT ( 'NONE',  ( -20.63663879154963965, 20.74370688441071664, 4.329123301634322907 ) ) ;
#44490 = EDGE_CURVE ( 'NONE', #11209, #8418, #31445, .T. ) ;
#44491 = DIRECTION ( 'NONE',  ( 0.000000000000000000, -1.000000000000000000, 0.000000000000000000 ) ) ;
#44492 = CARTESIAN_POINT ( 'NONE',  ( -70.56555449637278343, -1.000000000000001776, -8.047023921085740383 ) ) ;
#44493 = VERTEX_POINT ( 'NONE', #36512 ) ;
#44494 = FACE_OUTER_BOUND ( 'NONE', #25779, .T. ) ;
#44495 = CARTESIAN_POINT ( 'NONE',  ( -10.27421835998572064, 0.000000000000000000, 10.96090226820206048 ) ) ;
#44496 = LINE ( 'NONE', #28295, #31834 ) ;
#44497 = VECTOR ( 'NONE', #41637, 999.9999999999998863 ) ;
#44498 = DIRECTION ( 'NONE',  ( 0.007781995580012662783, 0.000000000000000000, -0.9999697198139514409 ) ) ;
#44499 = EDGE_CURVE ( 'NONE', #5827, #27227, #26900, .T. ) ;
#44500 = DIRECTION ( 'NONE',  ( -0.6427681459581293666, -0.7660444431189770143, -0.005002170337467561935 ) ) ;
#44501 = FACE_OUTER_BOUND ( 'NONE', #25208, .T. ) ;
#44502 = CARTESIAN_POINT ( 'NONE',  ( -9.299412559631017317, 0.000000000000000000, 5.117369016537971937 ) ) ;
#44503 = ADVANCED_FACE ( 'NONE', ( #5318 ), #45317, .F. ) ;
#44504 = PLANE ( 'NONE',  #48639 ) ;
#44505 = PLANE ( 'NONE',  #17467 ) ;
#44506 = EDGE_CURVE ( 'NONE', #37427, #36569, #31714, .T. ) ;
#44507 = VERTEX_POINT ( 'NONE', #18347 ) ;
#44508 = VECTOR ( 'NONE', #21591, 1000.000000000000227 ) ;
#44509 = VECTOR ( 'NONE', #13573, 1000.000000000000000 ) ;
#44510 = EDGE_CURVE ( 'NONE', #14416, #10323, #53831, .T. ) ;
#44511 = VERTEX_POINT ( 'NONE', #5574 ) ;
#44512 = ORIENTED_EDGE ( 'NONE', *, *, #7425, .T. ) ;
#44513 = VERTEX_POINT ( 'NONE', #14401 ) ;
#44514 = VERTEX_POINT ( 'NONE', #41048 ) ;
#44515 = DIRECTION ( 'NONE',  ( 0.6427681459581294776, -0.7660444431189769032, 0.005002170337467562802 ) ) ;
#44516 = CARTESIAN_POINT ( 'NONE',  ( -19.32961685222932147, 0.000000000000000000, 14.39908572644263351 ) ) ;
#44517 = ORIENTED_EDGE ( 'NONE', *, *, #33852, .F. ) ;
#44518 = ORIENTED_EDGE ( 'NONE', *, *, #10609, .F. ) ;
#44519 = VERTEX_POINT ( 'NONE', #35688 ) ;
#44520 = DIRECTION ( 'NONE',  ( -0.6427681459581293666, -0.7660444431189770143, -0.005002170337467561935 ) ) ;
#44521 = EDGE_LOOP ( 'NONE', ( #23629, #20583, #34994, #32307 ) ) ;
#44522 = CARTESIAN_POINT ( 'NONE',  ( -17.86287064673334868, 0.000000000000000000, 5.050726205597795726 ) ) ;
#44523 = LINE ( 'NONE', #39989, #24076 ) ;
#44524 = VERTEX_POINT ( 'NONE', #10412 ) ;
#44525 = LINE ( 'NONE', #13597, #41865 ) ;
#44526 = EDGE_CURVE ( 'NONE', #18734, #52995, #2140, .T. ) ;
#44527 = ORIENTED_EDGE ( 'NONE', *, *, #18004, .T. ) ;
#44528 = VECTOR ( 'NONE', #35432, 1000.000000000000227 ) ;
#44529 = VECTOR ( 'NONE', #47400, 1000.000000000000114 ) ;
#44530 = DIRECTION ( 'NONE',  ( -0.6427681459581293666, -0.7660444431189770143, -0.005002170337467561935 ) ) ;
#44531 = EDGE_CURVE ( 'NONE', #13033, #33148, #40222, .T. ) ;
#44532 = DIRECTION ( 'NONE',  ( 0.005961354470445682716, -0.6427876096865404731, -0.7660212471507180654 ) ) ;
#44533 = CARTESIAN_POINT ( 'NONE',  ( -14.18665187206895517, 4.981562823951511731, 10.56749175989368617 ) ) ;
#44534 = DIRECTION ( 'NONE',  ( 0.5449076811759707706, 0.6444004775717708799, -0.5364919789714476250 ) ) ;
#44535 = ORIENTED_EDGE ( 'NONE', *, *, #25158, .F. ) ;
#44536 = DIRECTION ( 'NONE',  ( 0.9999697198139515519, 0.000000000000000000, 0.007781995580013368816 ) ) ;
#44537 = CARTESIAN_POINT ( 'NONE',  ( -11.20636620717317378, 0.000000000000000000, 11.32298014792380414 ) ) ;
#44538 = FACE_OUTER_BOUND ( 'NONE', #26122, .T. ) ;
#44539 = EDGE_CURVE ( 'NONE', #9189, #18, #16254, .T. ) ;
#44540 = VERTEX_POINT ( 'NONE', #19183 ) ;
#44541 = DIRECTION ( 'NONE',  ( -0.5364919789714478471, 0.6444004775717705469, -0.5449076811759709926 ) ) ;
#44542 = ORIENTED_EDGE ( 'NONE', *, *, #23718, .F. ) ;
#44543 = ADVANCED_FACE ( 'NONE', ( #10117 ), #23197, .F. ) ;
#44544 = EDGE_CURVE ( 'NONE', #37239, #48873, #2970, .T. ) ;
#44545 = ADVANCED_FACE ( 'NONE', ( #11529 ), #2691, .F. ) ;
#44546 = LINE ( 'NONE', #14208, #53699 ) ;
#44547 = DIRECTION ( 'NONE',  ( -0.005002170337468016433, -0.7660444431189770143, 0.6427681459581293666 ) ) ;
#44548 = LINE ( 'NONE', #18436, #24955 ) ;
#44549 = FACE_OUTER_BOUND ( 'NONE', #5086, .T. ) ;
#44550 = DIRECTION ( 'NONE',  ( -0.5449076811759708816, 0.6444004775717707689, 0.5364919789714475140 ) ) ;
#44551 = CARTESIAN_POINT ( 'NONE',  ( -17.87017515285991820, 0.000000000000000000, 5.989339556076115123 ) ) ;
#44552 = CARTESIAN_POINT ( 'NONE',  ( -15.96710241509184058, -0.1191753592594218814, 13.13259134697452879 ) ) ;
#44553 = AXIS2_PLACEMENT_3D ( 'NONE', #20442, #45712, #6280 ) ;
#44554 = DIRECTION ( 'NONE',  ( -0.9934890585767658377, -0.1139275668495182969, 0.000000000000000000 ) ) ;
#44555 = DIRECTION ( 'NONE',  ( 0.6427681459581294776, -0.7660444431189769032, 0.005002170337467562802 ) ) ;
#44556 = ORIENTED_EDGE ( 'NONE', *, *, #28292, .F. ) ;
#44557 = FACE_OUTER_BOUND ( 'NONE', #6208, .T. ) ;
#44558 = CARTESIAN_POINT ( 'NONE',  ( -17.74404816805336793, 0.000000000000000000, 3.574322630375089460 ) ) ;
#44559 = CARTESIAN_POINT ( 'NONE',  ( -9.342070512798265725, 0.000000000000000000, 10.59882438848031505 ) ) ;
#44560 = LINE ( 'NONE', #26693, #43227 ) ;
#44561 = DIRECTION ( 'NONE',  ( 0.9999697198139515519, 0.000000000000000000, 0.007781995580013368816 ) ) ;
#44562 = EDGE_CURVE ( 'NONE', #52307, #9050, #41347, .T. ) ;
#44563 = LINE ( 'NONE', #48854, #55951 ) ;
#44564 = LINE ( 'NONE', #48567, #54646 ) ;
#44565 = ORIENTED_EDGE ( 'NONE', *, *, #14381, .F. ) ;
#44566 = ADVANCED_FACE ( 'NONE', ( #46143 ), #6996, .F. ) ;
#44567 = ORIENTED_EDGE ( 'NONE', *, *, #18520, .T. ) ;
#44568 = EDGE_CURVE ( 'NONE', #42953, #47190, #3276, .T. ) ;
#44569 = CARTESIAN_POINT ( 'NONE',  ( -18.57070714969772496, 4.657758921906509642, 11.73899034496769112 ) ) ;
#44570 = DIRECTION ( 'NONE',  ( -0.9999697198139514409, -0.000000000000000000, -0.007781995580013368816 ) ) ;
#44571 = VECTOR ( 'NONE', #28586, 999.9999999999998863 ) ;
#44572 = EDGE_CURVE ( 'NONE', #55458, #27295, #3549, .T. ) ;
#44573 = VECTOR ( 'NONE', #30741, 999.9999999999998863 ) ;
#44574 = ORIENTED_EDGE ( 'NONE', *, *, #34149, .F. ) ;
#44575 = DIRECTION ( 'NONE',  ( 0.005002170337468016433, -0.7660444431189770143, -0.6427681459581293666 ) ) ;
#44576 = ORIENTED_EDGE ( 'NONE', *, *, #37329, .F. ) ;
#44577 = CARTESIAN_POINT ( 'NONE',  ( -19.39757902869610717, 2.391131607591508335, 4.140320553562598427 ) ) ;
#44578 = EDGE_CURVE ( 'NONE', #34394, #17707, #54650, .T. ) ;
#44579 = ORIENTED_EDGE ( 'NONE', *, *, #31753, .T. ) ;
#44580 = ORIENTED_EDGE ( 'NONE', *, *, #12205, .F. ) ;
#44581 = VECTOR ( 'NONE', #21075, 1000.000000000000227 ) ;
#44582 = EDGE_LOOP ( 'NONE', ( #18009, #1673, #51321, #35244 ) ) ;
#44583 = CARTESIAN_POINT ( 'NONE',  ( -20.54204810873173415, 0.000000000000000000, 4.860550213503115558 ) ) ;
#44584 = CARTESIAN_POINT ( 'NONE',  ( -19.62507351517958298, -0.1191753592594172323, 5.506347433322916096 ) ) ;
#44585 = PLANE ( 'NONE',  #38455 ) ;
#44586 = PLANE ( 'NONE',  #40268 ) ;
#44587 = VERTEX_POINT ( 'NONE', #55496 ) ;
#44588 = EDGE_LOOP ( 'NONE', ( #23903, #30975, #30288, #19028 ) ) ;
#44589 = VECTOR ( 'NONE', #23936, 1000.000000000000227 ) ;
#44590 = LINE ( 'NONE', #52560, #52684 ) ;
#44591 = ORIENTED_EDGE ( 'NONE', *, *, #42920, .T. ) ;
#44592 = CARTESIAN_POINT ( 'NONE',  ( -18.67697421479882181, -0.1191753592594197858, 4.036397482078229793 ) ) ;
#44593 = EDGE_LOOP ( 'NONE', ( #19602, #13559, #46803, #26359 ) ) ;
#44594 = CARTESIAN_POINT ( 'NONE',  ( -18.67775241435682432, 0.000000000000000000, 4.136394454059623804 ) ) ;
#44595 = DIRECTION ( 'NONE',  ( 0.000000000000000000, -1.000000000000000000, 0.000000000000000000 ) ) ;
#44596 = VERTEX_POINT ( 'NONE', #24299 ) ;
#44597 = CARTESIAN_POINT ( 'NONE',  ( -24.26986129792355129, -0.1191753592594197858, 6.208864760408702388 ) ) ;
#44598 = ORIENTED_EDGE ( 'NONE', *, *, #24580, .T. ) ;
#44599 = DIRECTION ( 'NONE',  ( 0.005002170337468016433, -0.7660444431189770143, -0.6427681459581293666 ) ) ;
#44600 = ORIENTED_EDGE ( 'NONE', *, *, #11679, .F. ) ;
#44601 = CARTESIAN_POINT ( 'NONE',  ( -15.40103151951671734, 0.000000000000000000, 12.95233060667165681 ) ) ;
#44602 = CARTESIAN_POINT ( 'NONE',  ( -27.06708303904391144, 0.000000000000000000, 7.395095371555332697 ) ) ;
#44603 = LINE ( 'NONE', #1991, #3836 ) ;
#44604 = ORIENTED_EDGE ( 'NONE', *, *, #43021, .T. ) ;
#44605 = EDGE_CURVE ( 'NONE', #34911, #17803, #7522, .T. ) ;
#44606 = ADVANCED_FACE ( 'NONE', ( #28846 ), #32547, .F. ) ;
#44607 = AXIS2_PLACEMENT_3D ( 'NONE', #14554, #9759, #41458 ) ;
#44608 = VECTOR ( 'NONE', #20740, 999.9999999999998863 ) ;
#44609 = DIRECTION ( 'NONE',  ( -0.005002170337468016433, -0.7660444431189770143, 0.6427681459581293666 ) ) ;
#44610 = CARTESIAN_POINT ( 'NONE',  ( 2.072287782118878319, 0.000000000000000000, -2.950529333540147015 ) ) ;
#44611 = DIRECTION ( 'NONE',  ( -0.7660212471507179544, -0.6427876096865405842, -0.005961354470445141482 ) ) ;
#44612 = EDGE_CURVE ( 'NONE', #25423, #5277, #16317, .T. ) ;
#44613 = FACE_OUTER_BOUND ( 'NONE', #32166, .T. ) ;
#44614 = CARTESIAN_POINT ( 'NONE',  ( -17.78664430235221516, -0.1191753592594194527, 8.105979003199307087 ) ) ;
#44615 = CARTESIAN_POINT ( 'NONE',  ( -67.38907591727327429, -11.43549468865002972, -4.725549651853786948 ) ) ;
#44616 = VECTOR ( 'NONE', #6030, 999.9999999999998863 ) ;
#44617 = VERTEX_POINT ( 'NONE', #33636 ) ;
#44618 = DIRECTION ( 'NONE',  ( 0.000000000000000000, -0.000000000000000000, -1.000000000000000000 ) ) ;
#44619 = CARTESIAN_POINT ( 'NONE',  ( -8.364753971622430839, 6.050419986852017651, 0.03078093515494761956 ) ) ;
#44620 = DIRECTION ( 'NONE',  ( -0.005002170337468016433, -0.7660444431189770143, 0.6427681459581293666 ) ) ;
#44621 = ORIENTED_EDGE ( 'NONE', *, *, #8948, .F. ) ;
#44622 = DIRECTION ( 'NONE',  ( 2.551063935260010306E-17, -5.102127870520020982E-16, 1.000000000000000000 ) ) ;
#44623 = DIRECTION ( 'NONE',  ( -0.7660212471507179544, -0.6427876096865405842, -0.005961354470445141482 ) ) ;
#44624 = EDGE_LOOP ( 'NONE', ( #3846, #32842, #48757, #7384 ) ) ;
#44625 = CARTESIAN_POINT ( 'NONE',  ( -16.22839869333036589, 0.2864062442990018553, 2.976455044025407837 ) ) ;
#44626 = PLANE ( 'NONE',  #40370 ) ;
#44627 = AXIS2_PLACEMENT_3D ( 'NONE', #4204, #50491, #34298 ) ;
#44628 = CARTESIAN_POINT ( 'NONE',  ( -24.27063949748155380, 0.000000000000000000, 6.308861732390097288 ) ) ;
#44629 = ADVANCED_FACE ( 'NONE', ( #41608 ), #50950, .F. ) ;
#44630 = CARTESIAN_POINT ( 'NONE',  ( -29.86197018149027116, 0.000000000000000000, 8.281335066757780083 ) ) ;
#44631 = ORIENTED_EDGE ( 'NONE', *, *, #33536, .T. ) ;
#44632 = ORIENTED_EDGE ( 'NONE', *, *, #19860, .F. ) ;
#44633 = DIRECTION ( 'NONE',  ( 0.000000000000000000, -1.000000000000000000, 0.000000000000000000 ) ) ;
#44634 = FACE_OUTER_BOUND ( 'NONE', #18227, .T. ) ;
#44635 = DIRECTION ( 'NONE',  ( 0.7660212471507180654, -0.6427876096865404731, 0.005961354470445141482 ) ) ;
#44636 = EDGE_CURVE ( 'NONE', #42224, #6825, #22353, .T. ) ;
#44637 = FACE_OUTER_BOUND ( 'NONE', #12742, .T. ) ;
#44638 = ORIENTED_EDGE ( 'NONE', *, *, #49744, .T. ) ;
#44639 = DIRECTION ( 'NONE',  ( 0.007781995580012663651, -3.146120232559066537E-19, -0.9999697198139514409 ) ) ;
#44640 = VECTOR ( 'NONE', #37588, 999.9999999999998863 ) ;
#44641 = ORIENTED_EDGE ( 'NONE', *, *, #26619, .T. ) ;
#44642 = DIRECTION ( 'NONE',  ( -0.005961354470445682716, -0.6427876096865404731, 0.7660212471507180654 ) ) ;
#44643 = EDGE_CURVE ( 'NONE', #49209, #6017, #33388, .T. ) ;
#44644 = CARTESIAN_POINT ( 'NONE',  ( -16.38698550481839433, -0.1191753592594179401, 7.378207331987803208 ) ) ;
#44645 = EDGE_LOOP ( 'NONE', ( #17639, #7813, #43234, #54181 ) ) ;
#44646 = ADVANCED_FACE ( 'NONE', ( #16065 ), #45580, .F. ) ;
#44647 = DIRECTION ( 'NONE',  ( -0.005961354470445682716, -0.6427876096865404731, 0.7660212471507180654 ) ) ;
#44648 = VECTOR ( 'NONE', #9763, 1000.000000000000114 ) ;
#44649 = DIRECTION ( 'NONE',  ( -0.005002170337468016433, -0.7660444431189770143, 0.6427681459581293666 ) ) ;
#44650 = EDGE_CURVE ( 'NONE', #54725, #30542, #15478, .T. ) ;
#44651 = CARTESIAN_POINT ( 'NONE',  ( -15.50102849149811135, -0.1191753592594197858, 12.95155240711365430 ) ) ;
#44652 = ORIENTED_EDGE ( 'NONE', *, *, #18806, .F. ) ;
#44653 = AXIS2_PLACEMENT_3D ( 'NONE', #45346, #1346, #27198 ) ;
#44654 = VECTOR ( 'NONE', #8826, 999.9999999999998863 ) ;
#44655 = DIRECTION ( 'NONE',  ( 0.007781995580012662783, 0.000000000000000000, -0.9999697198139514409 ) ) ;
#44656 = EDGE_CURVE ( 'NONE', #3804, #39510, #54381, .T. ) ;
#44657 = ORIENTED_EDGE ( 'NONE', *, *, #47755, .F. ) ;
#44658 = ORIENTED_EDGE ( 'NONE', *, *, #52477, .F. ) ;
#44659 = VECTOR ( 'NONE', #1893, 1000.000000000000000 ) ;
#44660 = VERTEX_POINT ( 'NONE', #52386 ) ;
#44661 = LINE ( 'NONE', #23101, #4148 ) ;
#44662 = AXIS2_PLACEMENT_3D ( 'NONE', #26084, #38264, #43107 ) ;
#44663 = ORIENTED_EDGE ( 'NONE', *, *, #13850, .F. ) ;
#44664 = CARTESIAN_POINT ( 'NONE',  ( -10.27421835998572064, 0.000000000000000000, 10.96090226820206048 ) ) ;
#44665 = EDGE_LOOP ( 'NONE', ( #19228, #17659, #23576, #22270 ) ) ;
#44666 = CARTESIAN_POINT ( 'NONE',  ( -12.33850799832341849, 0.000000000000000000, 11.68350162852954632 ) ) ;
#44667 = CARTESIAN_POINT ( 'NONE',  ( -11.40636015113596180, 0.000000000000000000, 11.32142374880780089 ) ) ;
#44668 = ORIENTED_EDGE ( 'NONE', *, *, #36245, .F. ) ;
#44669 = ORIENTED_EDGE ( 'NONE', *, *, #47250, .T. ) ;
#44671 = VECTOR ( 'NONE', #44762, 999.9999999999998863 ) ;
#44670 = FACE_OUTER_BOUND ( 'NONE', #53733, .T. ) ;
#44672 = ORIENTED_EDGE ( 'NONE', *, *, #9369, .F. ) ;
#44673 = CARTESIAN_POINT ( 'NONE',  ( -10.24461301995560447, 0.000000000000000000, 7.156679653253562812 ) ) ;
#44674 = DIRECTION ( 'NONE',  ( -0.6427681459581293666, -0.7660444431189770143, -0.005002170337467561935 ) ) ;
#44675 = PLANE ( 'NONE',  #33202 ) ;
#44676 = CARTESIAN_POINT ( 'NONE',  ( -56.00000000000000711, 4.550000000000001599, -2.749999999999994671 ) ) ;
#44677 = PLANE ( 'NONE',  #41393 ) ;
#44678 = CARTESIAN_POINT ( 'NONE',  ( -17.74560456716937296, 0.000000000000000000, 3.774316574337878372 ) ) ;
#44679 = FACE_OUTER_BOUND ( 'NONE', #55079, .T. ) ;
#44680 = ORIENTED_EDGE ( 'NONE', *, *, #25838, .F. ) ;
#44681 = AXIS2_PLACEMENT_3D ( 'NONE', #18077, #52999, #23469 ) ;
#44682 = EDGE_CURVE ( 'NONE', #44124, #45158, #52091, .T. ) ;
#44683 = VERTEX_POINT ( 'NONE', #43013 ) ;
#44684 = PLANE ( 'NONE',  #14682 ) ;
#44685 = LINE ( 'NONE', #18878, #38445 ) ;
#44686 = VECTOR ( 'NONE', #15126, 1000.000000000000227 ) ;
#44687 = EDGE_CURVE ( 'NONE', #33244, #28164, #21722, .T. ) ;
#44688 = EDGE_CURVE ( 'NONE', #14263, #14113, #8952, .T. ) ;
#44689 = CARTESIAN_POINT ( 'NONE',  ( -16.73317108723761137, -2.784623065533160524, 3.292208973453862431 ) ) ;
#44690 = FACE_OUTER_BOUND ( 'NONE', #755, .T. ) ;
#44691 = EDGE_LOOP ( 'NONE', ( #40774, #23351, #32849, #48011 ) ) ;
#44692 = DIRECTION ( 'NONE',  ( -0.000000000000000000, -0.000000000000000000, -1.000000000000000000 ) ) ;
#44693 = FACE_OUTER_BOUND ( 'NONE', #40488, .T. ) ;
#44694 = ORIENTED_EDGE ( 'NONE', *, *, #55520, .T. ) ;
#44696 = CARTESIAN_POINT ( 'NONE',  ( -21.47263955680318404, 0.000000000000000000, 5.022634149262071190 ) ) ;
#44695 = VECTOR ( 'NONE', #50855, 1000.000000000000114 ) ;
#44697 = CARTESIAN_POINT ( 'NONE',  ( -17.41703447003996175, 0.000000000000000000, 7.470194280875182002 ) ) ;
#44698 = ORIENTED_EDGE ( 'NONE', *, *, #42270, .T. ) ;
#44699 = AXIS2_PLACEMENT_3D ( 'NONE', #39548, #30989, #30168 ) ;
#44700 = VECTOR ( 'NONE', #33189, 1000.000000000000227 ) ;
#44701 = CARTESIAN_POINT ( 'NONE',  ( -13.27065584551087163, 0.000000000000000000, 12.04557950825129176 ) ) ;
#44702 = DIRECTION ( 'NONE',  ( 0.000000000000000000, 1.000000000000000000, 0.000000000000000000 ) ) ;
#44703 = DIRECTION ( 'NONE',  ( -0.5364919789714478471, 0.6444004775717705469, -0.5449076811759709926 ) ) ;
#44704 = CARTESIAN_POINT ( 'NONE',  ( -25.20278734466900517, 0.000000000000000000, 6.670939612111840944 ) ) ;
#44705 = EDGE_CURVE ( 'NONE', #35804, #23263, #35082, .T. ) ;
#44706 = CARTESIAN_POINT ( 'NONE',  ( -9.075990533167328067, 0.000000000000000000, 10.41622904950343909 ) ) ;
#44707 = ORIENTED_EDGE ( 'NONE', *, *, #28472, .F. ) ;
#44708 = CIRCLE ( 'NONE', #38339, 2.000000000000002220 ) ;
#44709 = AXIS2_PLACEMENT_3D ( 'NONE', #37659, #54987, #48056 ) ;
#44710 = ORIENTED_EDGE ( 'NONE', *, *, #31051, .T. ) ;
#44711 = CARTESIAN_POINT ( 'NONE',  ( -17.70820938652583365, -5.051250379848164052, 3.598629682913965677 ) ) ;
#44712 = CARTESIAN_POINT ( 'NONE',  ( -20.36148084596629459, -1.003701604285656579, 4.758388420423439236 ) ) ;
#44713 = CARTESIAN_POINT ( 'NONE',  ( -3.336033939804074588, 4.483638672814038273, -1.922544701254425004 ) ) ;
#44714 = DIRECTION ( 'NONE',  ( 0.7660212471507180654, -0.6427876096865404731, 0.005961354470445141482 ) ) ;
#44715 = VECTOR ( 'NONE', #38555, 999.9999999999998863 ) ;
#44716 = DIRECTION ( 'NONE',  ( 0.9999697198139515519, 0.000000000000000000, 0.007781995580013368816 ) ) ;
#44717 = ORIENTED_EDGE ( 'NONE', *, *, #33462, .F. ) ;
#44719 = VECTOR ( 'NONE', #37696, 999.9999999999998863 ) ;
#44718 = CARTESIAN_POINT ( 'NONE',  ( -18.63902545115410092, 21.89702948422484496, -4.188660131781243301 ) ) ;
#44720 = EDGE_CURVE ( 'NONE', #13585, #1119, #25996, .T. ) ;
#44721 = LINE ( 'NONE', #1274, #35678 ) ;
#44722 = PLANE ( 'NONE',  #54048 ) ;
#44723 = CARTESIAN_POINT ( 'NONE',  ( -20.41971299214364421, 20.86894905309189596, -4.314906280119092941 ) ) ;
#44724 = VERTEX_POINT ( 'NONE', #30801 ) ;
#44725 = EDGE_CURVE ( 'NONE', #13033, #32707, #4668, .T. ) ;
#44726 = CARTESIAN_POINT ( 'NONE',  ( -18.19747506107908563, 0.000000000000000000, 14.03856424583689311 ) ) ;
#44727 = ORIENTED_EDGE ( 'NONE', *, *, #25998, .T. ) ;
#44728 = DIRECTION ( 'NONE',  ( 0.6427681459581294776, -0.7660444431189769032, 0.005002170337467562802 ) ) ;
#44729 = VECTOR ( 'NONE', #2628, 1000.000000000000000 ) ;
#44730 = LINE ( 'NONE', #36229, #28435 ) ;
#44731 = ORIENTED_EDGE ( 'NONE', *, *, #52503, .F. ) ;
#44732 = CARTESIAN_POINT ( 'NONE',  ( -10.96535795190825091, 0.1245042932765017124, 0.9372768063285339402 ) ) ;
#44733 = ADVANCED_FACE ( 'NONE', ( #16600 ), #3816, .F. ) ;
#44734 = VECTOR ( 'NONE', #25042, 999.9999999999998863 ) ;
#44735 = ORIENTED_EDGE ( 'NONE', *, *, #14387, .T. ) ;
#44736 = VERTEX_POINT ( 'NONE', #34487 ) ;
#44737 = EDGE_LOOP ( 'NONE', ( #37036, #31573, #45711, #22616 ) ) ;
#44738 = CARTESIAN_POINT ( 'NONE',  ( -28.48094711209952123, 16.21479336393476700, 4.707673465834044890 ) ) ;
#44739 = ORIENTED_EDGE ( 'NONE', *, *, #45527, .F. ) ;
#44740 = ORIENTED_EDGE ( 'NONE', *, *, #47091, .F. ) ;
#44741 = VECTOR ( 'NONE', #55773, 1000.000000000000114 ) ;
#44742 = LINE ( 'NONE', #35675, #40185 ) ;
#44743 = DIRECTION ( 'NONE',  ( 0.5364919789714477361, 0.6444004775717706579, 0.5449076811759711036 ) ) ;
#44744 = VERTEX_POINT ( 'NONE', #26520 ) ;
#44745 = EDGE_CURVE ( 'NONE', #30192, #45238, #12375, .T. ) ;
#44746 = VECTOR ( 'NONE', #41270, 999.9999999999998863 ) ;
#44747 = AXIS2_PLACEMENT_3D ( 'NONE', #22842, #9810, #26536 ) ;
#44748 = ORIENTED_EDGE ( 'NONE', *, *, #20725, .F. ) ;
#44749 = CARTESIAN_POINT ( 'NONE',  ( -20.89189044771117665, -4.403642575758161648, 4.855941604891849117 ) ) ;
#44750 = ORIENTED_EDGE ( 'NONE', *, *, #53860, .T. ) ;
#44751 = EDGE_CURVE ( 'NONE', #53425, #40325, #43841, .T. ) ;
#44752 = ORIENTED_EDGE ( 'NONE', *, *, #46076, .T. ) ;
#44753 = ADVANCED_FACE ( 'NONE', ( #4409 ), #4957, .F. ) ;
#44754 = VECTOR ( 'NONE', #36937, 999.9999999999998863 ) ;
#44755 = CIRCLE ( 'NONE', #32075, 3.000000000000001332 ) ;
#44756 = FACE_OUTER_BOUND ( 'NONE', #7145, .T. ) ;
#44757 = DIRECTION ( 'NONE',  ( -0.5364919789714478471, 0.6444004775717705469, -0.5449076811759709926 ) ) ;
#44758 = CARTESIAN_POINT ( 'NONE',  ( 5.558065546916891364, 8.867787166497208620E-06, 2.260478567416572826 ) ) ;
#44759 = CARTESIAN_POINT ( 'NONE',  ( -68.26837592669477317, -11.12930981495617644, -7.480194822499078633 ) ) ;
#44760 = EDGE_CURVE ( 'NONE', #5490, #931, #22286, .T. ) ;
#44761 = ORIENTED_EDGE ( 'NONE', *, *, #44760, .F. ) ;
#44762 = DIRECTION ( 'NONE',  ( 0.9999697198139515519, 0.000000000000000000, 0.007781995580013368816 ) ) ;
#44763 = ORIENTED_EDGE ( 'NONE', *, *, #8464, .F. ) ;
#44764 = ADVANCED_FACE ( 'NONE', ( #33936 ), #34240, .F. ) ;
#44765 = DIRECTION ( 'NONE',  ( -0.9999697198139514409, -0.000000000000000000, -0.007781995580013368816 ) ) ;
#44766 = ADVANCED_FACE ( 'NONE', ( #17438 ), #51254, .F. ) ;
#44767 = DIRECTION ( 'NONE',  ( 0.5449076811759707706, 0.6444004775717708799, -0.5364919789714476250 ) ) ;
#44768 = LINE ( 'NONE', #49308, #7727 ) ;
#44769 = PLANE ( 'NONE',  #14017 ) ;
#44770 = VECTOR ( 'NONE', #46323, 999.9999999999998863 ) ;
#44771 = CARTESIAN_POINT ( 'NONE',  ( -17.73140113748535285, 0.000000000000000000, 13.85752530597602039 ) ) ;
#44772 = CARTESIAN_POINT ( 'NONE',  ( -13.48557508382207359, 0.000000000000000000, 5.654129457846438278 ) ) ;
#44773 = ORIENTED_EDGE ( 'NONE', *, *, #13260, .F. ) ;
#44774 = CARTESIAN_POINT ( 'NONE',  ( -14.39317410385126372, 0.000000000000000000, 2.861735767543279518 ) ) ;
#44775 = AXIS2_PLACEMENT_3D ( 'NONE', #34014, #3356, #33448 ) ;
#44776 = ORIENTED_EDGE ( 'NONE', *, *, #16983, .F. ) ;
#44777 = EDGE_CURVE ( 'NONE', #52307, #51848, #43565, .T. ) ;
#44778 = LINE ( 'NONE', #31729, #39233 ) ;
#44779 = CARTESIAN_POINT ( 'NONE',  ( -13.47539652419022360, 0.000000000000000000, 4.346206404110358079 ) ) ;
#44780 = ADVANCED_FACE ( 'NONE', ( #51544 ), #21452, .F. ) ;
#44781 = CARTESIAN_POINT ( 'NONE',  ( -58.57533928340691887, 0.08623575067603483912, -3.000000000000007105 ) ) ;
#44782 = VECTOR ( 'NONE', #7069, 1000.000000000000227 ) ;
#44783 = LINE ( 'NONE', #31468, #33157 ) ;
#44784 = CARTESIAN_POINT ( 'NONE',  ( -16.02312377951670896, 0.000000000000000000, 7.481042016179210385 ) ) ;
#44785 = ADVANCED_FACE ( 'NONE', ( #29955 ), #51799, .F. ) ;
#44786 = CARTESIAN_POINT ( 'NONE',  ( -13.53673582514181106, 0.000000000000000000, 12.22817484722816772 ) ) ;
#44787 = ORIENTED_EDGE ( 'NONE', *, *, #11286, .T. ) ;
#44788 = AXIS2_PLACEMENT_3D ( 'NONE', #47762, #34668, #39209 ) ;
#44789 = DIRECTION ( 'NONE',  ( 0.9321478471874541372, 0.000000000000000000, -0.3620778797217453771 ) ) ;
#44790 = DIRECTION ( 'NONE',  ( -0.005961354470445682716, -0.6427876096865404731, 0.7660212471507180654 ) ) ;
#44791 = CARTESIAN_POINT ( 'NONE',  ( -13.70441031555024480, 0.6102101463440035012, 1.985721203314722016 ) ) ;
#44792 = VECTOR ( 'NONE', #3684, 999.9999999999998863 ) ;
#44793 = FACE_OUTER_BOUND ( 'NONE', #48149, .T. ) ;
#44794 = DIRECTION ( 'NONE',  ( 0.5449076811759707706, 0.6444004775717708799, -0.5364919789714476250 ) ) ;
#44795 = DIRECTION ( 'NONE',  ( 0.9321478471874541372, 0.000000000000000000, -0.3620778797217453771 ) ) ;
#44796 = VECTOR ( 'NONE', #48060, 999.9999999999998863 ) ;
#44797 = VECTOR ( 'NONE', #53787, 999.9999999999998863 ) ;
#44798 = CARTESIAN_POINT ( 'NONE',  ( -11.40636015113596180, 0.000000000000000000, 11.32142374880780089 ) ) ;
#44799 = LINE ( 'NONE', #49884, #28321 ) ;
#44800 = ORIENTED_EDGE ( 'NONE', *, *, #17615, .T. ) ;
#44801 = EDGE_CURVE ( 'NONE', #43375, #51735, #6049, .T. ) ;
#44802 = EDGE_LOOP ( 'NONE', ( #20987, #29126, #37911, #1653 ) ) ;
#44803 = ORIENTED_EDGE ( 'NONE', *, *, #26268, .T. ) ;
#44804 = ORIENTED_EDGE ( 'NONE', *, *, #10214, .F. ) ;
#44805 = ORIENTED_EDGE ( 'NONE', *, *, #44195, .T. ) ;
#44806 = DIRECTION ( 'NONE',  ( 0.005961354470445682716, -0.6427876096865404731, -0.7660212471507180654 ) ) ;
#44807 = CARTESIAN_POINT ( 'NONE',  ( 2.072287782118878319, 0.000000000000000000, -2.950529333540147015 ) ) ;
#44808 = VECTOR ( 'NONE', #42404, 1000.000000000000227 ) ;
#44809 = EDGE_CURVE ( 'NONE', #41560, #3665, #10842, .T. ) ;
#44810 = VERTEX_POINT ( 'NONE', #28428 ) ;
#44811 = EDGE_LOOP ( 'NONE', ( #26964, #9568, #6612, #11417 ) ) ;
#44812 = ORIENTED_EDGE ( 'NONE', *, *, #8881, .T. ) ;
#44813 = AXIS2_PLACEMENT_3D ( 'NONE', #21518, #17514, #47625 ) ;
#44814 = EDGE_CURVE ( 'NONE', #34831, #25201, #50289, .T. ) ;
#44815 = EDGE_CURVE ( 'NONE', #54486, #44201, #37224, .T. ) ;
#44816 = CARTESIAN_POINT ( 'NONE',  ( -67.52981462395439394, -9.438526564586886991, -7.865887534710968687 ) ) ;
#44817 = AXIS2_PLACEMENT_3D ( 'NONE', #11830, #15526, #8152 ) ;
#44818 = CARTESIAN_POINT ( 'NONE',  ( -13.73672976910459909, 0.000000000000000000, 12.22661844811216270 ) ) ;
#44819 = DIRECTION ( 'NONE',  ( 0.5364919789714477361, 0.6444004775717706579, 0.5449076811759711036 ) ) ;
#44820 = ORIENTED_EDGE ( 'NONE', *, *, #8816, .F. ) ;
#44821 = CYLINDRICAL_SURFACE ( 'NONE', #1083, 0.2499999999999998612 ) ;
#44822 = VECTOR ( 'NONE', #47340, 999.9999999999998863 ) ;
#44823 = EDGE_LOOP ( 'NONE', ( #43281, #4283, #40519, #50145 ) ) ;
#44824 = LINE ( 'NONE', #48529, #9198 ) ;
#44825 = EDGE_CURVE ( 'NONE', #50536, #18340, #45211, .T. ) ;
#44826 = DIRECTION ( 'NONE',  ( 0.5364919789714477361, 0.6444004775717706579, 0.5449076811759711036 ) ) ;
#44827 = ADVANCED_FACE ( 'NONE', ( #23615 ), #27611, .F. ) ;
#44828 = VECTOR ( 'NONE', #517, 1000.000000000000114 ) ;
#44829 = CARTESIAN_POINT ( 'NONE',  ( -15.71187809204705665, 4.657758921906512306, 2.636351864413973622 ) ) ;
#44830 = DIRECTION ( 'NONE',  ( 0.005002170337468016433, -0.7660444431189770143, -0.6427681459581293666 ) ) ;
#44831 = VECTOR ( 'NONE', #30768, 1000.000000000000000 ) ;
#44832 = CARTESIAN_POINT ( 'NONE',  ( -14.21625583054634845, 1.743523803501505709, 5.264817263711710105 ) ) ;
#44833 = DIRECTION ( 'NONE',  ( -0.3620778797217456546, 0.000000000000000000, -0.9321478471874540261 ) ) ;
#44834 = DIRECTION ( 'NONE',  ( 0.005002170337468016433, -0.7660444431189770143, -0.6427681459581293666 ) ) ;
#44835 = EDGE_LOOP ( 'NONE', ( #11449, #34251, #31120, #29064 ) ) ;
#44836 = DIRECTION ( 'NONE',  ( -0.005002170337468016433, -0.7660444431189770143, 0.6427681459581293666 ) ) ;
#44837 = ORIENTED_EDGE ( 'NONE', *, *, #46327, .T. ) ;
#44838 = EDGE_CURVE ( 'NONE', #30294, #50472, #32688, .T. ) ;
#44839 = LINE ( 'NONE', #31524, #1073 ) ;
#44840 = DIRECTION ( 'NONE',  ( 0.007781995580012663651, 0.000000000000000000, -0.9999697198139515519 ) ) ;
#44841 = DIRECTION ( 'NONE',  ( 0.000000000000000000, 0.000000000000000000, 1.000000000000000000 ) ) ;
#44842 = CARTESIAN_POINT ( 'NONE',  ( -13.95308603416844484, 0.000000000000000000, 6.019823249336194948 ) ) ;
#44843 = PLANE ( 'NONE',  #34131 ) ;
#44844 = FACE_OUTER_BOUND ( 'NONE', #35735, .T. ) ;
#44845 = CARTESIAN_POINT ( 'NONE',  ( -17.02012697683945319, -0.3560938001956556742, 3.481155184349101539 ) ) ;
#44846 = VECTOR ( 'NONE', #32415, 1000.000000000000114 ) ;
#44847 = EDGE_CURVE ( 'NONE', #12550, #41644, #32444, .T. ) ;
#44848 = PLANE ( 'NONE',  #13809 ) ;
#44849 = VECTOR ( 'NONE', #44055, 1000.000000000000227 ) ;
#44850 = LINE ( 'NONE', #49100, #36507 ) ;
#44851 = ORIENTED_EDGE ( 'NONE', *, *, #25149, .F. ) ;
#44852 = PLANE ( 'NONE',  #29353 ) ;
#44853 = CARTESIAN_POINT ( 'NONE',  ( -28.92982233430281980, 0.000000000000000000, 7.919257187036034651 ) ) ;
#44854 = FACE_OUTER_BOUND ( 'NONE', #8201, .T. ) ;
#44855 = AXIS2_PLACEMENT_3D ( 'NONE', #4541, #13067, #20745 ) ;
#44856 = LINE ( 'NONE', #48850, #41390 ) ;
#44857 = CARTESIAN_POINT ( 'NONE',  ( -14.10280672071693431, -0.1191753592594197858, 12.40843558753103792 ) ) ;
#44858 = CARTESIAN_POINT ( 'NONE',  ( -16.81190032086591302, 0.000000000000000000, 3.212244750653343583 ) ) ;
#44859 = LINE ( 'NONE', #32087, #47374 ) ;
#44860 = ORIENTED_EDGE ( 'NONE', *, *, #39728, .T. ) ;
#44861 = VECTOR ( 'NONE', #27445, 1000.000000000000227 ) ;
#44862 = VERTEX_POINT ( 'NONE', #54530 ) ;
#44863 = FACE_OUTER_BOUND ( 'NONE', #10113, .T. ) ;
#44864 = VECTOR ( 'NONE', #35987, 1000.000000000000227 ) ;
#44865 = FACE_OUTER_BOUND ( 'NONE', #19047, .T. ) ;
#44866 = VECTOR ( 'NONE', #28140, 999.9999999999998863 ) ;
#44867 = ORIENTED_EDGE ( 'NONE', *, *, #36572, .F. ) ;
#44868 = LINE ( 'NONE', #40041, #51239 ) ;
#44869 = ADVANCED_FACE ( 'NONE', ( #6576 ), #44626, .F. ) ;
#44870 = VERTEX_POINT ( 'NONE', #11106 ) ;
#44871 = CARTESIAN_POINT ( 'NONE',  ( -10.21719013929205566, 0.000000000000000000, 3.632898379970893821 ) ) ;
#44872 = VECTOR ( 'NONE', #44716, 999.9999999999998863 ) ;
#44873 = ORIENTED_EDGE ( 'NONE', *, *, #49746, .T. ) ;
#44874 = AXIS2_PLACEMENT_3D ( 'NONE', #21732, #39042, #39631 ) ;
#44875 = EDGE_LOOP ( 'NONE', ( #21194, #45928, #42002, #54617 ) ) ;
#44876 = EDGE_CURVE ( 'NONE', #45468, #34418, #40391, .T. ) ;
#44877 = ORIENTED_EDGE ( 'NONE', *, *, #9982, .T. ) ;
#44878 = EDGE_CURVE ( 'NONE', #11770, #11704, #1489, .T. ) ;
#44879 = DIRECTION ( 'NONE',  ( -0.5449076811759708816, 0.6444004775717707689, 0.5364919789714475140 ) ) ;
#44880 = CARTESIAN_POINT ( 'NONE',  ( -25.20200914511100265, -0.1191753592594197858, 6.570942640130446932 ) ) ;
#44881 = CARTESIAN_POINT ( 'NONE',  ( -12.55761894452918170, 0.000000000000000000, 5.830677040677434420 ) ) ;
#44882 = ADVANCED_FACE ( 'NONE', ( #19349, #15637 ), #6872, .F. ) ;
#44883 = EDGE_CURVE ( 'NONE', #29528, #14368, #36146, .T. ) ;
#44884 = EDGE_CURVE ( 'NONE', #31703, #10496, #54277, .T. ) ;
#44885 = DIRECTION ( 'NONE',  ( 0.005961354470445682716, -0.6427876096865404731, -0.7660212471507180654 ) ) ;
#44886 = ORIENTED_EDGE ( 'NONE', *, *, #36477, .F. ) ;
#44887 = ORIENTED_EDGE ( 'NONE', *, *, #11419, .F. ) ;
#44888 = AXIS2_PLACEMENT_3D ( 'NONE', #20950, #24649, #51361 ) ;
#44889 = CARTESIAN_POINT ( 'NONE',  ( -14.42478869240937378, 0.000000000000000000, 6.924142503378688751 ) ) ;
#44890 = AXIS2_PLACEMENT_3D ( 'NONE', #11832, #33162, #16115 ) ;
#44891 = ORIENTED_EDGE ( 'NONE', *, *, #47714, .T. ) ;
#44892 = PLANE ( 'NONE',  #3034 ) ;
#44893 = ORIENTED_EDGE ( 'NONE', *, *, #51691, .F. ) ;
#44894 = AXIS2_PLACEMENT_3D ( 'NONE', #37035, #2645, #6941 ) ;
#44895 = FACE_OUTER_BOUND ( 'NONE', #33689, .T. ) ;
#44896 = CARTESIAN_POINT ( 'NONE',  ( 2.072287782118878319, 0.000000000000000000, -2.950529333540147015 ) ) ;
#44897 = ORIENTED_EDGE ( 'NONE', *, *, #38223, .F. ) ;
#44898 = DIRECTION ( 'NONE',  ( 0.9999697198139515519, 0.000000000000000000, 0.007781995580013368816 ) ) ;
#44899 = EDGE_CURVE ( 'NONE', #47831, #15979, #36397, .T. ) ;
#44900 = VECTOR ( 'NONE', #30739, 999.9999999999998863 ) ;
#44901 = VERTEX_POINT ( 'NONE', #31860 ) ;
#44902 = EDGE_CURVE ( 'NONE', #18997, #6604, #49171, .T. ) ;
#44903 = CARTESIAN_POINT ( 'NONE',  ( -18.59370689556874012, 0.000000000000000000, 5.245044725140569852 ) ) ;
#44904 = VECTOR ( 'NONE', #37547, 1000.000000000000227 ) ;
#44905 = AXIS2_PLACEMENT_3D ( 'NONE', #36451, #54332, #18584 ) ;
#44906 = EDGE_LOOP ( 'NONE', ( #22844, #34424, #8998, #31488 ) ) ;
#44907 = DIRECTION ( 'NONE',  ( 0.000000000000000000, -1.000000000000000000, 0.000000000000000000 ) ) ;
#44908 = FACE_OUTER_BOUND ( 'NONE', #44875, .T. ) ;
#44909 = EDGE_CURVE ( 'NONE', #23765, #1914, #40679, .T. ) ;
#44910 = VECTOR ( 'NONE', #2313, 1000.000000000000227 ) ;
#44911 = CARTESIAN_POINT ( 'NONE',  ( -18.86354292863559579, 0.000000000000000000, 14.21804678658176080 ) ) ;
#44912 = ORIENTED_EDGE ( 'NONE', *, *, #27211, .T. ) ;
#44913 = AXIS2_PLACEMENT_3D ( 'NONE', #37424, #12723, #56168 ) ;
#44914 = EDGE_CURVE ( 'NONE', #28441, #6152, #15123, .T. ) ;
#44915 = DIRECTION ( 'NONE',  ( 0.9321478471874540261, 0.000000000000000000, -0.3620778797217456546 ) ) ;
#44916 = DIRECTION ( 'NONE',  ( 0.005961354470445682716, -0.6427876096865404731, -0.7660212471507180654 ) ) ;
#44917 = CARTESIAN_POINT ( 'NONE',  ( -17.70211622298184651, 0.000000000000000000, 10.09447668306734514 ) ) ;
#44918 = LINE ( 'NONE', #44075, #31376 ) ;
#44919 = DIRECTION ( 'NONE',  ( -0.6427681459581293666, -0.7660444431189770143, -0.005002170337467561935 ) ) ;
#44920 = DIRECTION ( 'NONE',  ( -0.5364919789714478471, 0.6444004775717705469, -0.5449076811759709926 ) ) ;
#44921 = VECTOR ( 'NONE', #17213, 1000.000000000000114 ) ;
#44922 = VECTOR ( 'NONE', #3216, 1000.000000000000227 ) ;
#44923 = CARTESIAN_POINT ( 'NONE',  ( -66.59666794111869592, -11.34462593484436077, -7.222001337329467141 ) ) ;
#44924 = ORIENTED_EDGE ( 'NONE', *, *, #52505, .F. ) ;
#44925 = FACE_OUTER_BOUND ( 'NONE', #9558, .T. ) ;
#44926 = CARTESIAN_POINT ( 'NONE',  ( -14.88080342873461248, 0.000000000000000000, 5.812597481837387114 ) ) ;
#44927 = CARTESIAN_POINT ( 'NONE',  ( -68.86577260744199691, -0.6013940400650622520, -6.479403174770926199 ) ) ;
#44928 = ORIENTED_EDGE ( 'NONE', *, *, #32084, .F. ) ;
#44929 = DIRECTION ( 'NONE',  ( 0.9999697198139515519, 0.000000000000000000, 0.007781995580013368816 ) ) ;
#44930 = CARTESIAN_POINT ( 'NONE',  ( 5.454418722303246092, 0.000000000000000000, -2.500028562687453437 ) ) ;
#44931 = VERTEX_POINT ( 'NONE', #12534 ) ;
#44932 = CARTESIAN_POINT ( 'NONE',  ( -25.20123094555300369, 0.000000000000000000, 6.470945668149052032 ) ) ;
#44933 = PLANE ( 'NONE',  #21502 ) ;
#44934 = DIRECTION ( 'NONE',  ( -0.7660212471507179544, -0.6427876096865405842, -0.005961354470445141482 ) ) ;
#44935 = VECTOR ( 'NONE', #34728, 1000.000000000000114 ) ;
#44936 = ORIENTED_EDGE ( 'NONE', *, *, #26913, .F. ) ;
#44937 = VERTEX_POINT ( 'NONE', #28733 ) ;
#44938 = VECTOR ( 'NONE', #24293, 1000.000000000000114 ) ;
#44939 = LINE ( 'NONE', #19355, #34074 ) ;
#44940 = PLANE ( 'NONE',  #14191 ) ;
#44941 = VECTOR ( 'NONE', #56038, 999.9999999999998863 ) ;
#44942 = PLANE ( 'NONE',  #11206 ) ;
#44943 = CARTESIAN_POINT ( 'NONE',  ( -15.08810187882396825, 0.000000000000000000, 6.749654433199698822 ) ) ;
#44944 = EDGE_LOOP ( 'NONE', ( #28507, #51250, #18708, #47535 ) ) ;
#44945 = DIRECTION ( 'NONE',  ( 0.007781995580012663651, -3.146120232559066537E-19, -0.9999697198139514409 ) ) ;
#44946 = VECTOR ( 'NONE', #46089, 1000.000000000000114 ) ;
#44947 = ADVANCED_FACE ( 'NONE', ( #33812 ), #7995, .F. ) ;
#44948 = EDGE_LOOP ( 'NONE', ( #38032, #41155, #7152, #15068 ) ) ;
#44949 = DIRECTION ( 'NONE',  ( -0.5449076811759708816, 0.6444004775717707689, 0.5364919789714475140 ) ) ;
#44950 = CARTESIAN_POINT ( 'NONE',  ( -27.99767448711536133, 0.000000000000000000, 7.557179307314289218 ) ) ;
#44951 = VECTOR ( 'NONE', #29312, 999.9999999999998863 ) ;
#44953 = ORIENTED_EDGE ( 'NONE', *, *, #7882, .F. ) ;
#44952 = VECTOR ( 'NONE', #25558, 999.9999999999998863 ) ;
#44954 = DIRECTION ( 'NONE',  ( -0.5449076811759708816, 0.6444004775717707689, 0.5364919789714475140 ) ) ;
#44955 = CARTESIAN_POINT ( 'NONE',  ( -14.85162214859956897, 1.419719901456505617, 2.405509639311967263 ) ) ;
#44956 = DIRECTION ( 'NONE',  ( 0.005002170337468016433, -0.7660444431189770143, -0.6427681459581293666 ) ) ;
#44957 = EDGE_CURVE ( 'NONE', #23998, #2328, #46042, .T. ) ;
#44958 = VECTOR ( 'NONE', #33662, 999.9999999999998863 ) ;
#44959 = EDGE_CURVE ( 'NONE', #44744, #55546, #50586, .T. ) ;
#44960 = EDGE_CURVE ( 'NONE', #21098, #27295, #33281, .T. ) ;
#44961 = VERTEX_POINT ( 'NONE', #11403 ) ;
#44962 = VECTOR ( 'NONE', #46617, 999.9999999999998863 ) ;
#44963 = CARTESIAN_POINT ( 'NONE',  ( -31.72704407542318350, -0.1191753592594197858, 9.105487798182664960 ) ) ;
#44964 = VECTOR ( 'NONE', #9892, 1000.000000000000000 ) ;
#44965 = ORIENTED_EDGE ( 'NONE', *, *, #3134, .F. ) ;
#44966 = EDGE_CURVE ( 'NONE', #9919, #50834, #42351, .T. ) ;
#44967 = VECTOR ( 'NONE', #29683, 999.9999999999998863 ) ;
#44968 = ORIENTED_EDGE ( 'NONE', *, *, #18053, .T. ) ;
#44969 = VECTOR ( 'NONE', #55823, 1000.000000000000227 ) ;
#44970 = ORIENTED_EDGE ( 'NONE', *, *, #9058, .F. ) ;
#44971 = DIRECTION ( 'NONE',  ( 0.5364919789714477361, 0.6444004775717706579, 0.5449076811759711036 ) ) ;
#44972 = ORIENTED_EDGE ( 'NONE', *, *, #27786, .F. ) ;
#44973 = LINE ( 'NONE', #10035, #9415 ) ;
#44974 = VERTEX_POINT ( 'NONE', #38347 ) ;
#44975 = CARTESIAN_POINT ( 'NONE',  ( -27.99845268667336384, -0.1191753592594197858, 7.657176279295684118 ) ) ;
#44976 = DIRECTION ( 'NONE',  ( 0.2426528472758542054, 0.7422098413412800966, 0.6246952433987894571 ) ) ;
#44977 = ORIENTED_EDGE ( 'NONE', *, *, #19061, .T. ) ;
#44978 = DIRECTION ( 'NONE',  ( 0.5364919789714477361, 0.6444004775717706579, 0.5449076811759711036 ) ) ;
#44979 = ORIENTED_EDGE ( 'NONE', *, *, #12090, .T. ) ;
#44980 = EDGE_CURVE ( 'NONE', #39202, #10472, #51433, .T. ) ;
#44981 = AXIS2_PLACEMENT_3D ( 'NONE', #38356, #47437, #34964 ) ;
#44982 = CARTESIAN_POINT ( 'NONE',  ( -14.37032732058113993, 24.36156349900039331, 3.880826686532125258 ) ) ;
#44983 = CARTESIAN_POINT ( 'NONE',  ( -24.26986129792355129, -0.1191753592594197858, 6.208864760408702388 ) ) ;
#44984 = CARTESIAN_POINT ( 'NONE',  ( -23.29661994227107868, 19.01267450544941084, 4.488313114961025363 ) ) ;
#44985 = CARTESIAN_POINT ( 'NONE',  ( -58.00000000000000711, -9.250000000000000000, -3.457106781186546129 ) ) ;
#44986 = ADVANCED_FACE ( 'NONE', ( #29850 ), #20759, .F. ) ;
#44987 = CARTESIAN_POINT ( 'NONE',  ( -21.06965149344186372, 20.49370688441071664, 4.356723378946029790 ) ) ;
#44988 = DIRECTION ( 'NONE',  ( -0.005961354470445682716, -0.6427876096865404731, 0.7660212471507180654 ) ) ;
#44989 = DIRECTION ( 'NONE',  ( 0.000000000000000000, -0.000000000000000000, -1.000000000000000000 ) ) ;
#44990 = VECTOR ( 'NONE', #12389, 999.9999999999998863 ) ;
#44991 = ORIENTED_EDGE ( 'NONE', *, *, #5228, .T. ) ;
#44993 = ORIENTED_EDGE ( 'NONE', *, *, #4348, .T. ) ;
#44992 = ADVANCED_FACE ( 'NONE', ( #25566 ), #15941, .F. ) ;
#44994 = DIRECTION ( 'NONE',  ( -0.000000000000000000, -0.000000000000000000, -1.000000000000000000 ) ) ;
#44995 = DIRECTION ( 'NONE',  ( 0.000000000000000000, -1.000000000000000000, 0.000000000000000000 ) ) ;
#44996 = VECTOR ( 'NONE', #6033, 999.9999999999998863 ) ;
#44997 = EDGE_CURVE ( 'NONE', #13033, #47531, #38651, .T. ) ;
#44998 = CARTESIAN_POINT ( 'NONE',  ( -19.60834386242827776, 0.000000000000000000, 4.298478389818581213 ) ) ;
#44999 = VECTOR ( 'NONE', #23805, 1000.000000000000227 ) ;
#45000 = VECTOR ( 'NONE', #14588, 1000.000000000000227 ) ;
#45001 = LINE ( 'NONE', #6113, #30403 ) ;
#45002 = VERTEX_POINT ( 'NONE', #7402 ) ;
#45003 = CARTESIAN_POINT ( 'NONE',  ( -12.26998356360862452, 0.000000000000000000, 2.878258927267324463 ) ) ;
#45004 = CARTESIAN_POINT ( 'NONE',  ( -11.62834515084701081, 0.000000000000000000, 5.837908864213453342 ) ) ;
#45005 = ORIENTED_EDGE ( 'NONE', *, *, #7507, .T. ) ;
#45006 = CARTESIAN_POINT ( 'NONE',  ( 2.072287782118878319, 0.000000000000000000, -2.950529333540147015 ) ) ;
#45007 = DIRECTION ( 'NONE',  ( -0.5449076811759708816, 0.6444004775717707689, 0.5364919789714475140 ) ) ;
#45008 = ORIENTED_EDGE ( 'NONE', *, *, #27070, .F. ) ;
#45009 = VECTOR ( 'NONE', #32278, 999.9999999999998863 ) ;
#45010 = CARTESIAN_POINT ( 'NONE',  ( -67.44329683095881478, -8.823711483744059336, 4.584835828370195543 ) ) ;
#45011 = DIRECTION ( 'NONE',  ( 0.007781995580012663651, -3.146120232559066537E-19, -0.9999697198139514409 ) ) ;
#45012 = VECTOR ( 'NONE', #48816, 1000.000000000000227 ) ;
#45013 = DIRECTION ( 'NONE',  ( -0.5364919789714478471, 0.6444004775717705469, -0.5449076811759709926 ) ) ;
#45014 = LINE ( 'NONE', #10665, #52262 ) ;
#45015 = VECTOR ( 'NONE', #45481, 1000.000000000000227 ) ;
#45016 = PLANE ( 'NONE',  #48285 ) ;
#45017 = EDGE_LOOP ( 'NONE', ( #284, #37654, #20411, #35673 ) ) ;
#45018 = VECTOR ( 'NONE', #16863, 1000.000000000000227 ) ;
#45019 = ORIENTED_EDGE ( 'NONE', *, *, #31051, .F. ) ;
#45020 = CARTESIAN_POINT ( 'NONE',  ( -14.89098198836645892, 0.000000000000000000, 7.120520535573467313 ) ) ;
#45021 = PLANE ( 'NONE',  #49428 ) ;
#45022 = LINE ( 'NONE', #6130, #48769 ) ;
#45023 = CARTESIAN_POINT ( 'NONE',  ( 5.558065690504402134, 8.867811663421879681E-06, -2.260478214935544017 ) ) ;
#45024 = DIRECTION ( 'NONE',  ( 0.5449076811759707706, 0.6444004775717708799, -0.5364919789714476250 ) ) ;
#45025 = EDGE_LOOP ( 'NONE', ( #37322, #32583, #9971, #3786 ) ) ;
#45026 = PLANE ( 'NONE',  #40116 ) ;
#45027 = DIRECTION ( 'NONE',  ( 0.000000000000000000, -1.000000000000000000, 0.000000000000000000 ) ) ;
#45028 = VECTOR ( 'NONE', #10527, 999.9999999999998863 ) ;
#45029 = CARTESIAN_POINT ( 'NONE',  ( -14.52556386394876853, -0.1191753592594177180, 7.023361275802077586 ) ) ;
#45030 = CARTESIAN_POINT ( 'NONE',  ( -19.77061338776520216, 21.24370688441071664, -4.270683379717145733 ) ) ;
#45031 = ORIENTED_EDGE ( 'NONE', *, *, #35516, .T. ) ;
#45032 = CARTESIAN_POINT ( 'NONE',  ( -20.06177075545399191, 0.000000000000000000, 14.76272000528038220 ) ) ;
#45033 = VERTEX_POINT ( 'NONE', #55974 ) ;
#45034 = DIRECTION ( 'NONE',  ( 0.005002170337468016433, -0.7660444431189770143, -0.6427681459581293666 ) ) ;
#45035 = AXIS2_PLACEMENT_3D ( 'NONE', #34714, #9742, #52592 ) ;
#45036 = FACE_OUTER_BOUND ( 'NONE', #44948, .T. ) ;
#45037 = EDGE_CURVE ( 'NONE', #40714, #49849, #17070, .T. ) ;
#45038 = EDGE_LOOP ( 'NONE', ( #12977, #24282, #5302, #22605 ) ) ;
#45039 = DIRECTION ( 'NONE',  ( -0.005961354470445682716, -0.6427876096865404731, 0.7660212471507180654 ) ) ;
#45040 = AXIS2_PLACEMENT_3D ( 'NONE', #34050, #12739, #55915 ) ;
#45041 = EDGE_LOOP ( 'NONE', ( #51386, #23624, #40006, #22820 ) ) ;
#45042 = ADVANCED_FACE ( 'NONE', ( #12235 ), #24448, .F. ) ;
#45043 = EDGE_CURVE ( 'NONE', #51697, #10299, #20484, .T. ) ;
#45044 = ORIENTED_EDGE ( 'NONE', *, *, #38717, .F. ) ;
#45045 = VECTOR ( 'NONE', #49090, 1000.000000000000227 ) ;
#45046 = ORIENTED_EDGE ( 'NONE', *, *, #44914, .F. ) ;
#45047 = FACE_OUTER_BOUND ( 'NONE', #30266, .T. ) ;
#45048 = VERTEX_POINT ( 'NONE', #55383 ) ;
#45049 = ORIENTED_EDGE ( 'NONE', *, *, #17358, .T. ) ;
#45050 = CARTESIAN_POINT ( 'NONE',  ( -16.10199555257484860, 4.495856970884009485, 10.51435023889596643 ) ) ;
#45051 = LINE ( 'NONE', #27724, #17669 ) ;
#45052 = ORIENTED_EDGE ( 'NONE', *, *, #49057, .T. ) ;
#45053 = VECTOR ( 'NONE', #52928, 1000.000000000000227 ) ;
#45054 = ORIENTED_EDGE ( 'NONE', *, *, #28097, .T. ) ;
#45055 = DIRECTION ( 'NONE',  ( 0.9999697198139515519, 0.000000000000000000, 0.007781995580013368816 ) ) ;
#45056 = ORIENTED_EDGE ( 'NONE', *, *, #4468, .T. ) ;
#45057 = ORIENTED_EDGE ( 'NONE', *, *, #5695, .F. ) ;
#45058 = VECTOR ( 'NONE', #3947, 1000.000000000000000 ) ;
#45059 = VECTOR ( 'NONE', #43205, 1000.000000000000000 ) ;
#45060 = DIRECTION ( 'NONE',  ( -0.005002170337468016433, -0.7660444431189770143, 0.6427681459581293666 ) ) ;
#45061 = CARTESIAN_POINT ( 'NONE',  ( -13.53673582514181106, 0.000000000000000000, 12.22817484722816772 ) ) ;
#45062 = CARTESIAN_POINT ( 'NONE',  ( -25.20200914511100265, -0.1191753592594197858, 6.570942640130446932 ) ) ;
#45063 = CARTESIAN_POINT ( 'NONE',  ( -24.26908309836554878, 0.000000000000000000, 6.108867788427308376 ) ) ;
#45064 = ORIENTED_EDGE ( 'NONE', *, *, #3656, .T. ) ;
#45065 = CARTESIAN_POINT ( 'NONE',  ( -18.59746678161252476, -2.784623065533160524, 4.016364732897353740 ) ) ;
#45066 = ORIENTED_EDGE ( 'NONE', *, *, #12544, .T. ) ;
#45067 = FACE_OUTER_BOUND ( 'NONE', #49800, .T. ) ;
#45068 = EDGE_CURVE ( 'NONE', #1446, #16052, #55127, .T. ) ;
#45069 = VECTOR ( 'NONE', #15729, 999.9999999999998863 ) ;
#45070 = CARTESIAN_POINT ( 'NONE',  ( -17.36532418587302473, -0.1191753592594177458, 13.67570816655714516 ) ) ;
#45071 = DIRECTION ( 'NONE',  ( 0.9999697198139515519, 0.000000000000000000, 0.007781995580013368816 ) ) ;
#45072 = CARTESIAN_POINT ( 'NONE',  ( -9.075990533167328067, 0.000000000000000000, 10.41622904950343909 ) ) ;
#45073 = EDGE_CURVE ( 'NONE', #1575, #37986, #37511, .T. ) ;
#45074 = PLANE ( 'NONE',  #23011 ) ;
#45075 = DIRECTION ( 'NONE',  ( -0.5449076811759708816, 0.6444004775717707689, 0.5364919789714475140 ) ) ;
#45076 = EDGE_LOOP ( 'NONE', ( #26234, #45170, #49216, #41035 ) ) ;
#45077 = DIRECTION ( 'NONE',  ( 0.9321478471874541372, 0.000000000000000000, -0.3620778797217453771 ) ) ;
#45078 = PRODUCT_DEFINITION_SHAPE ( 'NONE', 'NONE',  #56237 ) ;
#45079 = ORIENTED_EDGE ( 'NONE', *, *, #15912, .F. ) ;
#45080 = DIRECTION ( 'NONE',  ( 0.9999697198139515519, 0.000000000000000000, 0.007781995580013368816 ) ) ;
#45081 = LINE ( 'NONE', #54150, #30536 ) ;
#45083 = FACE_OUTER_BOUND ( 'NONE', #8588, .T. ) ;
#45082 = AXIS2_PLACEMENT_3D ( 'NONE', #35126, #5291, #22329 ) ;
#45084 = ADVANCED_FACE ( 'NONE', ( #54832 ), #25304, .F. ) ;
#45085 = DIRECTION ( 'NONE',  ( 0.005002170337468016433, -0.7660444431189770143, -0.6427681459581293666 ) ) ;
#45086 = PLANE ( 'NONE',  #43193 ) ;
#45087 = VECTOR ( 'NONE', #16275, 1000.000000000000000 ) ;
#45088 = CARTESIAN_POINT ( 'NONE',  ( -67.50725361308181505, -1.000000000000000444, 2.158836163547857900 ) ) ;
#45089 = ORIENTED_EDGE ( 'NONE', *, *, #16092, .T. ) ;
#45090 = CYLINDRICAL_SURFACE ( 'NONE', #34832, 0.5000000000000004441 ) ;
#45091 = DIRECTION ( 'NONE',  ( 0.5364919789714477361, 0.6444004775717706579, 0.5449076811759711036 ) ) ;
#45092 = CARTESIAN_POINT ( 'NONE',  ( -19.25715946501773956, -2.460819163488159766, 4.282942814164549361 ) ) ;
#45093 = AXIS2_PLACEMENT_3D ( 'NONE', #40294, #31516, #10184 ) ;
#45094 = CARTESIAN_POINT ( 'NONE',  ( -69.63446883681038457, 1.041039752757419556, -7.493887922408439373 ) ) ;
#45095 = CARTESIAN_POINT ( 'NONE',  ( -20.63663870328428374, 20.74370693537071020, -4.329125112780540796 ) ) ;
#45096 = CARTESIAN_POINT ( 'NONE',  ( 0.3240706152708103804, -3.670543518250629855, 2.124999999999998668 ) ) ;
#45097 = CARTESIAN_POINT ( 'NONE',  ( -18.66354898467281132, 0.000000000000000000, 14.21960318569776582 ) ) ;
#45098 = VECTOR ( 'NONE', #10151, 999.9999999999998863 ) ;
#45099 = CARTESIAN_POINT ( 'NONE',  ( -68.87050791938486327, -8.585715889274698753, -6.450409451741323075 ) ) ;
#45100 = CARTESIAN_POINT ( 'NONE',  ( -19.61264301455797465, 3.200641362704010007, 4.198031109838099795 ) ) ;
#45101 = EDGE_CURVE ( 'NONE', #30427, #47379, #39772, .T. ) ;
#45102 = ORIENTED_EDGE ( 'NONE', *, *, #31290, .F. ) ;
#45103 = ADVANCED_FACE ( 'NONE', ( #588 ), #34957, .F. ) ;
#45104 = ADVANCED_FACE ( 'NONE', ( #4301 ), #9373, .F. ) ;
#45105 = ORIENTED_EDGE ( 'NONE', *, *, #28616, .F. ) ;
#45106 = ORIENTED_EDGE ( 'NONE', *, *, #25886, .T. ) ;
#45107 = EDGE_LOOP ( 'NONE', ( #25607, #20751, #42766, #55427 ) ) ;
#45108 = ORIENTED_EDGE ( 'NONE', *, *, #54741, .F. ) ;
#45109 = DIRECTION ( 'NONE',  ( -0.9999697198139514409, -0.000000000000000000, -0.007781995580013368816 ) ) ;
#45110 = DIRECTION ( 'NONE',  ( -0.9999697198139514409, -0.000000000000000000, -0.007781995580013368816 ) ) ;
#45111 = PRODUCT_RELATED_PRODUCT_CATEGORY ( 'part', '', ( #22810 ) ) ;
#45112 = EDGE_LOOP ( 'NONE', ( #53953, #2489, #21537, #32660 ) ) ;
#45113 = VERTEX_POINT ( 'NONE', #18168 ) ;
#45114 = VERTEX_POINT ( 'NONE', #21614 ) ;
#45115 = EDGE_CURVE ( 'NONE', #56197, #47765, #17917, .T. ) ;
#45116 = VECTOR ( 'NONE', #45539, 999.9999999999998863 ) ;
#45117 = DIRECTION ( 'NONE',  ( -0.7660212471507179544, -0.6427876096865405842, -0.005961354470445141482 ) ) ;
#45118 = DIRECTION ( 'NONE',  ( 0.007781995580012662783, 0.000000000000000000, -0.9999697198139514409 ) ) ;
#45119 = DIRECTION ( 'NONE',  ( 0.9999697198139515519, 0.000000000000000000, 0.007781995580013368816 ) ) ;
#45120 = ORIENTED_EDGE ( 'NONE', *, *, #44876, .F. ) ;
#45121 = CARTESIAN_POINT ( 'NONE',  ( -10.74029228357944987, 0.000000000000000000, 11.14194120806293320 ) ) ;
#45122 = ORIENTED_EDGE ( 'NONE', *, *, #30, .F. ) ;
#45123 = VECTOR ( 'NONE', #9588, 1000.000000000000227 ) ;
#45124 = LINE ( 'NONE', #19252, #16439 ) ;
#45125 = DIRECTION ( 'NONE',  ( 0.000000000000000000, -1.000000000000000000, 0.000000000000000000 ) ) ;
#45126 = DIRECTION ( 'NONE',  ( 0.000000000000000000, 0.000000000000000000, 1.000000000000000000 ) ) ;
#45127 = DIRECTION ( 'NONE',  ( -0.6427681459581293666, -0.7660444431189770143, -0.005002170337467561935 ) ) ;
#45128 = DIRECTION ( 'NONE',  ( 0.005002170337468016433, -0.7660444431189770143, -0.6427681459581293666 ) ) ;
#45129 = CARTESIAN_POINT ( 'NONE',  ( -15.40103151951671734, 0.000000000000000000, 12.95233060667165681 ) ) ;
#45130 = CARTESIAN_POINT ( 'NONE',  ( -12.80458192191714595, 0.000000000000000000, 11.86454056839041726 ) ) ;
#45131 = CARTESIAN_POINT ( 'NONE',  ( -16.26190025084746082, 0.000000000000000000, 4.155195174207322317 ) ) ;
#45132 = EDGE_LOOP ( 'NONE', ( #38598, #26644, #18338, #32270 ) ) ;
#45133 = DIRECTION ( 'NONE',  ( 0.005002170337468016433, -0.7660444431189770143, -0.6427681459581293666 ) ) ;
#45134 = ORIENTED_EDGE ( 'NONE', *, *, #3677, .T. ) ;
#45135 = DIRECTION ( 'NONE',  ( -0.5449076811759708816, 0.6444004775717707689, 0.5364919789714475140 ) ) ;
#45136 = DIRECTION ( 'NONE',  ( -0.7660212471507179544, -0.6427876096865405842, -0.005961354470445141482 ) ) ;
#45137 = DIRECTION ( 'NONE',  ( -0.6427681459581293666, -0.7660444431189770143, -0.005002170337467561935 ) ) ;
#45138 = CARTESIAN_POINT ( 'NONE',  ( -31.72626587586518099, 0.000000000000000000, 9.005490826201270949 ) ) ;
#45139 = ADVANCED_FACE ( 'NONE', ( #35240 ), #8542, .F. ) ;
#45140 = CARTESIAN_POINT ( 'NONE',  ( -16.81190032086591302, 0.000000000000000000, 3.212244750653343583 ) ) ;
#45141 = DIRECTION ( 'NONE',  ( -0.5364919789714478471, 0.6444004775717705469, -0.5449076811759709926 ) ) ;
#45142 = DIRECTION ( 'NONE',  ( -0.7660212471507179544, -0.6427876096865405842, -0.005961354470445141482 ) ) ;
#45143 = PLANE ( 'NONE',  #22093 ) ;
#45144 = DIRECTION ( 'NONE',  ( -0.005002170337468016433, -0.7660444431189770143, 0.6427681459581293666 ) ) ;
#45145 = VERTEX_POINT ( 'NONE', #17619 ) ;
#45146 = LINE ( 'NONE', #14481, #22100 ) ;
#45147 = DIRECTION ( 'NONE',  ( -0.7660212471507179544, -0.6427876096865405842, -0.005961354470445141482 ) ) ;
#45148 = DIRECTION ( 'NONE',  ( 0.2426528472758541499, 0.7422098413412800966, 0.6246952433987894571 ) ) ;
#45149 = CARTESIAN_POINT ( 'NONE',  ( -10.74029228357944987, 0.000000000000000000, 11.14194120806293320 ) ) ;
#45150 = EDGE_CURVE ( 'NONE', #19093, #27501, #43457, .T. ) ;
#45151 = CARTESIAN_POINT ( 'NONE',  ( -14.63340479688801032, 0.000000000000000000, 8.030515214035977678 ) ) ;
#45152 = CARTESIAN_POINT ( 'NONE',  ( -9.391565570654567097, -0.1191753592594177180, 4.108658679188065932 ) ) ;
#45153 = ADVANCED_FACE ( 'NONE', ( #848 ), #26694, .F. ) ;
#45154 = DIRECTION ( 'NONE',  ( -0.005961354470445682716, -0.6427876096865404731, 0.7660212471507180654 ) ) ;
#45155 = EDGE_CURVE ( 'NONE', #12359, #24475, #13908, .T. ) ;
#45156 = LINE ( 'NONE', #49937, #23820 ) ;
#45157 = VERTEX_POINT ( 'NONE', #9093 ) ;
#45158 = VERTEX_POINT ( 'NONE', #9679 ) ;
#45159 = CARTESIAN_POINT ( 'NONE',  ( -16.73647696259367024, 0.000000000000000000, 5.428824131507583139 ) ) ;
#45160 = CARTESIAN_POINT ( 'NONE',  ( -14.46438462897659250, 2.067327705546506689, 2.234431356499322341 ) ) ;
#45161 = ADVANCED_FACE ( 'NONE', ( #44305 ), #31237, .F. ) ;
#45162 = AXIS2_PLACEMENT_3D ( 'NONE', #31591, #17965, #30995 ) ;
#45163 = VERTEX_POINT ( 'NONE', #35491 ) ;
#45164 = EDGE_CURVE ( 'NONE', #14416, #21318, #40030, .T. ) ;
#45165 = LINE ( 'NONE', #1430, #46740 ) ;
#45166 = EDGE_LOOP ( 'NONE', ( #15462, #84, #25692, #54548, #23099 ) ) ;
#45167 = LINE ( 'NONE', #19297, #39272 ) ;
#45168 = EDGE_CURVE ( 'NONE', #38799, #46492, #1116, .T. ) ;
#45169 = ORIENTED_EDGE ( 'NONE', *, *, #13133, .F. ) ;
#45170 = ORIENTED_EDGE ( 'NONE', *, *, #2621, .T. ) ;
#45171 = ORIENTED_EDGE ( 'NONE', *, *, #29182, .T. ) ;
#45172 = LINE ( 'NONE', #31259, #45626 ) ;
#45173 = FACE_OUTER_BOUND ( 'NONE', #33855, .T. ) ;
#45174 = FACE_OUTER_BOUND ( 'NONE', #384, .T. ) ;
#45175 = EDGE_CURVE ( 'NONE', #44358, #2142, #9781, .T. ) ;
#45176 = ORIENTED_EDGE ( 'NONE', *, *, #42546, .F. ) ;
#45177 = ORIENTED_EDGE ( 'NONE', *, *, #34237, .T. ) ;
#45178 = EDGE_CURVE ( 'NONE', #37328, #31229, #22714, .T. ) ;
#45179 = CARTESIAN_POINT ( 'NONE',  ( -10.27421835998572064, 0.000000000000000000, 10.96090226820206048 ) ) ;
#45180 = VERTEX_POINT ( 'NONE', #4555 ) ;
#45181 = PLANE ( 'NONE',  #22795 ) ;
#45182 = ORIENTED_EDGE ( 'NONE', *, *, #55791, .T. ) ;
#45183 = DIRECTION ( 'NONE',  ( 0.9999697198139515519, 0.000000000000000000, 0.007781995580013368816 ) ) ;
#45184 = CARTESIAN_POINT ( 'NONE',  ( -14.30671182103509054, 0.7721120973665049902, 2.214510042402868972 ) ) ;
#45185 = ORIENTED_EDGE ( 'NONE', *, *, #27610, .F. ) ;
#45186 = DIRECTION ( 'NONE',  ( 0.9999697198139515519, 0.000000000000000000, 0.007781995580013368816 ) ) ;
#45187 = CARTESIAN_POINT ( 'NONE',  ( -17.02322106989970507, -0.3560938001956550081, 3.878739497874950093 ) ) ;
#45188 = ORIENTED_EDGE ( 'NONE', *, *, #14705, .F. ) ;
#45189 = CARTESIAN_POINT ( 'NONE',  ( -49.27554558092695913, 2.476975532698160620, 5.000000000000000000 ) ) ;
#45190 = DIRECTION ( 'NONE',  ( 0.000000000000000000, -1.000000000000000000, 0.000000000000000000 ) ) ;
#45191 = DIRECTION ( 'NONE',  ( 0.9999697198139515519, 0.000000000000000000, 0.007781995580013368816 ) ) ;
#45192 = EDGE_LOOP ( 'NONE', ( #47208, #51158, #10630, #54115 ) ) ;
#45193 = VECTOR ( 'NONE', #53634, 1000.000000000000114 ) ;
#45194 = PLANE ( 'NONE',  #32829 ) ;
#45195 = CARTESIAN_POINT ( 'NONE',  ( -14.87948577434532815, 0.000000000000000000, 5.643281722542411671 ) ) ;
#45196 = CARTESIAN_POINT ( 'NONE',  ( -16.38411145131311031, -0.1191753592594183703, 7.008897628730038853 ) ) ;
#45197 = EDGE_CURVE ( 'NONE', #9219, #41657, #47735, .T. ) ;
#45198 = PLANE ( 'NONE',  #25949 ) ;
#45199 = CARTESIAN_POINT ( 'NONE',  ( -9.342070512798265725, 0.000000000000000000, 10.59882438848031505 ) ) ;
#45200 = LINE ( 'NONE', #50276, #42440 ) ;
#45201 = CARTESIAN_POINT ( 'NONE',  ( -64.93522747905139170, -11.15410157257325885, 3.192571262229372930 ) ) ;
#45202 = EDGE_LOOP ( 'NONE', ( #47016, #42526, #7104, #16867 ) ) ;
#45203 = DIRECTION ( 'NONE',  ( 0.5449076811759707706, 0.6444004775717708799, -0.5364919789714476250 ) ) ;
#45204 = CARTESIAN_POINT ( 'NONE',  ( -13.03375205539139969, 0.000000000000000000, 7.304299941940480601 ) ) ;
#45205 = CARTESIAN_POINT ( 'NONE',  ( -67.13674736183641301, -0.6010214343564760364, -1.700609907706588375 ) ) ;
#45206 = EDGE_LOOP ( 'NONE', ( #10161, #30322, #22876, #17484 ) ) ;
#45207 = PLANE ( 'NONE',  #16616 ) ;
#45208 = CARTESIAN_POINT ( 'NONE',  ( -13.92853720701018183, 0.000000000000000000, 2.865351679311290756 ) ) ;
#45209 = EDGE_CURVE ( 'NONE', #12681, #25987, #12794, .T. ) ;
#45210 = EDGE_CURVE ( 'NONE', #18030, #5375, #17322, .T. ) ;
#45211 = LINE ( 'NONE', #49997, #42184 ) ;
#45212 = DIRECTION ( 'NONE',  ( 0.9999697198139515519, 0.000000000000000000, 0.007781995580013368816 ) ) ;
#45213 = EDGE_CURVE ( 'NONE', #29102, #42137, #2529, .T. ) ;
#45214 = DIRECTION ( 'NONE',  ( -0.5364919789714478471, 0.6444004775717705469, -0.5449076811759709926 ) ) ;
#45215 = ORIENTED_EDGE ( 'NONE', *, *, #41667, .T. ) ;
#45216 = ORIENTED_EDGE ( 'NONE', *, *, #48178, .T. ) ;
#45217 = DIRECTION ( 'NONE',  ( 0.5364919789714477361, 0.6444004775717706579, 0.5449076811759711036 ) ) ;
#45218 = CARTESIAN_POINT ( 'NONE',  ( -65.70692426961275601, 2.000000000000016875, 3.244935472805978272 ) ) ;
#45219 = CARTESIAN_POINT ( 'NONE',  ( -22.40634380310664397, 0.000000000000000000, 5.584705972946605534 ) ) ;
#45220 = ORIENTED_EDGE ( 'NONE', *, *, #32348, .T. ) ;
#45221 = EDGE_CURVE ( 'NONE', #40778, #23767, #6510, .T. ) ;
#45222 = DIRECTION ( 'NONE',  ( 0.7660212471507180654, -0.6427876096865404731, 0.005961354470445141482 ) ) ;
#45223 = VERTEX_POINT ( 'NONE', #45151 ) ;
#45224 = DIRECTION ( 'NONE',  ( 0.6427681459581294776, -0.7660444431189769032, 0.005002170337467562802 ) ) ;
#45225 = EDGE_CURVE ( 'NONE', #23847, #55136, #5675, .T. ) ;
#45226 = VERTEX_POINT ( 'NONE', #18761 ) ;
#45227 = PLANE ( 'NONE',  #12028 ) ;
#45228 = LINE ( 'NONE', #36163, #49551 ) ;
#45229 = DIRECTION ( 'NONE',  ( -0.7660212471507179544, -0.6427876096865405842, -0.005961354470445141482 ) ) ;
#45230 = ORIENTED_EDGE ( 'NONE', *, *, #24107, .F. ) ;
#45231 = EDGE_CURVE ( 'NONE', #29572, #23095, #5977, .T. ) ;
#45232 = VECTOR ( 'NONE', #35862, 1000.000000000000000 ) ;
#45233 = LINE ( 'NONE', #24213, #43910 ) ;
#45234 = EDGE_LOOP ( 'NONE', ( #9051, #22597, #44326, #24231, #3709, #10397 ) ) ;
#45235 = ORIENTED_EDGE ( 'NONE', *, *, #27467, .T. ) ;
#45236 = EDGE_LOOP ( 'NONE', ( #41131, #26291, #32719, #20009 ) ) ;
#45237 = DIRECTION ( 'NONE',  ( -0.7660212471507179544, -0.6427876096865405842, -0.005961354470445141482 ) ) ;
#45238 = VERTEX_POINT ( 'NONE', #53644 ) ;
#45239 = DIRECTION ( 'NONE',  ( 0.000000000000000000, -0.000000000000000000, -1.000000000000000000 ) ) ;
#45240 = ORIENTED_EDGE ( 'NONE', *, *, #3479, .F. ) ;
#45241 = CARTESIAN_POINT ( 'NONE',  ( -19.73901266685368938, -4.079838673713159558, 11.04494491366336995 ) ) ;
#45242 = CARTESIAN_POINT ( 'NONE',  ( -9.542064456761055524, 0.000000000000000000, 10.59726798936431180 ) ) ;
#45243 = ORIENTED_EDGE ( 'NONE', *, *, #38262, .F. ) ;
#45244 = CARTESIAN_POINT ( 'NONE',  ( -15.57145852836868549, -4.727446477803165514, 2.778974125015922336 ) ) ;
#45245 = VERTEX_POINT ( 'NONE', #19281 ) ;
#45246 = DIRECTION ( 'NONE',  ( -0.005002170337468016433, -0.7660444431189770143, 0.6427681459581293666 ) ) ;
#45247 = DIRECTION ( 'NONE',  ( -0.005002170337468016433, -0.7660444431189770143, 0.6427681459581293666 ) ) ;
#45248 = PLANE ( 'NONE',  #27778 ) ;
#45249 = CARTESIAN_POINT ( 'NONE',  ( -17.74482636761137044, -0.1191753592594197858, 3.674319602356483916 ) ) ;
#45250 = DIRECTION ( 'NONE',  ( 0.6427681459581294776, -0.7660444431189769032, 0.005002170337467562802 ) ) ;
#45251 = CARTESIAN_POINT ( 'NONE',  ( -15.60102546347950536, 0.000000000000000000, 12.95077420755565356 ) ) ;
#45252 = LINE ( 'NONE', #27362, #31056 ) ;
#45253 = ORIENTED_EDGE ( 'NONE', *, *, #54692, .T. ) ;
#45254 = EDGE_CURVE ( 'NONE', #8803, #50386, #27537, .T. ) ;
#45255 = EDGE_LOOP ( 'NONE', ( #38831, #55410, #8066, #7245 ) ) ;
#45256 = CARTESIAN_POINT ( 'NONE',  ( 2.072287782118878319, 0.000000000000000000, -2.950529333540147015 ) ) ;
#45257 = LINE ( 'NONE', #10055, #19432 ) ;
#45258 = ADVANCED_FACE ( 'NONE', ( #6254 ), #6796, .F. ) ;
#45259 = DIRECTION ( 'NONE',  ( 0.005002170337468016433, -0.7660444431189770143, -0.6427681459581293666 ) ) ;
#45260 = CARTESIAN_POINT ( 'NONE',  ( -24.27063949748155380, 0.000000000000000000, 6.308861732390097288 ) ) ;
#45261 = CARTESIAN_POINT ( 'NONE',  ( -11.25011315801890532, -0.1191753592594183703, 4.094195032116028976 ) ) ;
#45262 = EDGE_LOOP ( 'NONE', ( #5159, #48222, #45713, #14397 ) ) ;
#45263 = EDGE_CURVE ( 'NONE', #25181, #49693, #23557, .T. ) ;
#45264 = FACE_OUTER_BOUND ( 'NONE', #19625, .T. ) ;
#45265 = LINE ( 'NONE', #23417, #23230 ) ;
#45266 = ORIENTED_EDGE ( 'NONE', *, *, #41298, .F. ) ;
#45267 = DIRECTION ( 'NONE',  ( 0.007781995580012662783, 0.000000000000000000, -0.9999697198139514409 ) ) ;
#45268 = CARTESIAN_POINT ( 'NONE',  ( -12.62677952751046995, -0.1191753592594201328, 1.867489077265416908 ) ) ;
#45269 = ORIENTED_EDGE ( 'NONE', *, *, #47669, .T. ) ;
#45270 = EDGE_CURVE ( 'NONE', #49166, #44182, #36918, .T. ) ;
#45271 = EDGE_CURVE ( 'NONE', #32587, #42240, #14756, .T. ) ;
#45272 = ADVANCED_FACE ( 'NONE', ( #15316 ), #11037, .F. ) ;
#45273 = VECTOR ( 'NONE', #19065, 999.9999999999998863 ) ;
#45274 = CARTESIAN_POINT ( 'NONE',  ( -69.18604761972393646, -0.9999999999995233813, 6.394134653913046584 ) ) ;
#45275 = CARTESIAN_POINT ( 'NONE',  ( -25.20278734466900517, 0.000000000000000000, 6.670939612111840944 ) ) ;
#45276 = PLANE ( 'NONE',  #30456 ) ;
#45277 = EDGE_CURVE ( 'NONE', #45990, #40411, #49400, .T. ) ;
#45278 = FACE_OUTER_BOUND ( 'NONE', #29747, .T. ) ;
#45279 = CARTESIAN_POINT ( 'NONE',  ( -16.40332474553500575, -2.946525016555659793, 3.158919932820265064 ) ) ;
#45280 = ORIENTED_EDGE ( 'NONE', *, *, #31360, .F. ) ;
#45281 = EDGE_LOOP ( 'NONE', ( #49990, #53259, #5559, #21262 ) ) ;
#45282 = CARTESIAN_POINT ( 'NONE',  ( -12.13851405436063047, 0.000000000000000000, 11.68505802764555135 ) ) ;
#45283 = DIRECTION ( 'NONE',  ( -0.5364919789714478471, 0.6444004775717705469, -0.5449076811759709926 ) ) ;
#45284 = LINE ( 'NONE', #39901, #26073 ) ;
#45285 = LINE ( 'NONE', #40179, #51828 ) ;
#45286 = EDGE_CURVE ( 'NONE', #23729, #30483, #1950, .T. ) ;
#45287 = FACE_OUTER_BOUND ( 'NONE', #26713, .T. ) ;
#45288 = ORIENTED_EDGE ( 'NONE', *, *, #38149, .F. ) ;
#45289 = CARTESIAN_POINT ( 'NONE',  ( -16.29926294641613538, 0.000000000000000000, 8.956221316558263368 ) ) ;
#45290 = EDGE_CURVE ( 'NONE', #30787, #23833, #32381, .T. ) ;
#45291 = CARTESIAN_POINT ( 'NONE',  ( -31.72626587586518099, 0.000000000000000000, 9.005490826201270949 ) ) ;
#45292 = CARTESIAN_POINT ( 'NONE',  ( -12.11256978495757330, 0.9340140483890051470, 1.357065242325779408 ) ) ;
#45293 = ORIENTED_EDGE ( 'NONE', *, *, #6459, .T. ) ;
#45294 = EDGE_CURVE ( 'NONE', #7889, #22392, #45399, .T. ) ;
#45295 = LINE ( 'NONE', #6397, #45593 ) ;
#45296 = ORIENTED_EDGE ( 'NONE', *, *, #4251, .F. ) ;
#45297 = FACE_OUTER_BOUND ( 'NONE', #24152, .T. ) ;
#45298 = LINE ( 'NONE', #6400, #23899 ) ;
#45299 = ORIENTED_EDGE ( 'NONE', *, *, #19245, .F. ) ;
#45300 = EDGE_CURVE ( 'NONE', #33876, #39389, #48853, .T. ) ;
#45301 = CARTESIAN_POINT ( 'NONE',  ( -17.74482636761137044, -0.1191753592594197858, 3.674319602356483916 ) ) ;
#45302 = ORIENTED_EDGE ( 'NONE', *, *, #49320, .F. ) ;
#45303 = ADVANCED_FACE ( 'NONE', ( #19580 ), #28358, .T. ) ;
#45304 = EDGE_LOOP ( 'NONE', ( #19978, #5231, #41248, #46941 ) ) ;
#45305 = ORIENTED_EDGE ( 'NONE', *, *, #8804, .F. ) ;
#45306 = FACE_OUTER_BOUND ( 'NONE', #34, .T. ) ;
#45307 = ORIENTED_EDGE ( 'NONE', *, *, #39241, .F. ) ;
#45308 = ORIENTED_EDGE ( 'NONE', *, *, #12763, .T. ) ;
#45309 = CARTESIAN_POINT ( 'NONE',  ( -14.63208714249872955, 0.000000000000000000, 7.861199454741004899 ) ) ;
#45310 = EDGE_LOOP ( 'NONE', ( #16485, #13974, #6846, #48802 ) ) ;
#45311 = EDGE_LOOP ( 'NONE', ( #34626, #37833, #42080, #7419 ) ) ;
#45312 = DIRECTION ( 'NONE',  ( -0.5449076811759708816, 0.6444004775717707689, 0.5364919789714475140 ) ) ;
#45313 = ORIENTED_EDGE ( 'NONE', *, *, #26268, .F. ) ;
#45314 = VERTEX_POINT ( 'NONE', #14487 ) ;
#45315 = CARTESIAN_POINT ( 'NONE',  ( 2.072287782118878319, 0.000000000000000000, -2.950529333540147015 ) ) ;
#45316 = CARTESIAN_POINT ( 'NONE',  ( -11.72049816187055882, -0.1191753592594181482, 4.829198526863549112 ) ) ;
#45317 = PLANE ( 'NONE',  #49544 ) ;
#45318 = CARTESIAN_POINT ( 'NONE',  ( -18.67619601524082285, 0.000000000000000000, 3.936400510096834893 ) ) ;
#45319 = ORIENTED_EDGE ( 'NONE', *, *, #33159, .T. ) ;
#45320 = CARTESIAN_POINT ( 'NONE',  ( -14.50257143590650699, -0.1191753592594186895, 4.068883649739962749 ) ) ;
#45321 = ORIENTED_EDGE ( 'NONE', *, *, #43920, .F. ) ;
#45322 = ORIENTED_EDGE ( 'NONE', *, *, #36509, .T. ) ;
#45323 = FACE_OUTER_BOUND ( 'NONE', #19177, .T. ) ;
#45324 = CARTESIAN_POINT ( 'NONE',  ( -37.79788887702321176, 10.83565452793198425, -4.935543081462775206 ) ) ;
#45325 = LINE ( 'NONE', #6436, #8590 ) ;
#45326 = DIRECTION ( 'NONE',  ( 0.2426528472758542054, 0.7422098413412800966, 0.6246952433987894571 ) ) ;
#45327 = CARTESIAN_POINT ( 'NONE',  ( -9.342070512798265725, 0.000000000000000000, 10.59882438848031505 ) ) ;
#45328 = EDGE_LOOP ( 'NONE', ( #12687, #32859, #3446, #23432 ) ) ;
#45329 = CARTESIAN_POINT ( 'NONE',  ( -11.20636620717317378, 0.000000000000000000, 11.32298014792380414 ) ) ;
#45330 = ORIENTED_EDGE ( 'NONE', *, *, #52288, .T. ) ;
#45331 = ADVANCED_FACE ( 'NONE', ( #31798 ), #49109, .F. ) ;
#45332 = EDGE_CURVE ( 'NONE', #21088, #37252, #29501, .T. ) ;
#45333 = DIRECTION ( 'NONE',  ( 0.007781995580012663651, 0.000000000000000000, -0.9999697198139515519 ) ) ;
#45334 = LINE ( 'NONE', #14675, #6054 ) ;
#45335 = DIRECTION ( 'NONE',  ( -0.005002170337468016433, -0.7660444431189770143, 0.6427681459581293666 ) ) ;
#45336 = DIRECTION ( 'NONE',  ( 0.6427681459581294776, -0.7660444431189769032, 0.005002170337467562802 ) ) ;
#45337 = EDGE_CURVE ( 'NONE', #46574, #29949, #50219, .T. ) ;
#45338 = DIRECTION ( 'NONE',  ( 0.9999697198139515519, 0.000000000000000000, 0.007781995580013368816 ) ) ;
#45339 = VERTEX_POINT ( 'NONE', #55321 ) ;
#45340 = CARTESIAN_POINT ( 'NONE',  ( -17.90272870724953691, 0.000000000000000000, 10.17240138478555878 ) ) ;
#45341 = FACE_OUTER_BOUND ( 'NONE', #53908, .T. ) ;
#45342 = CARTESIAN_POINT ( 'NONE',  ( -9.969791507445457057, 0.000000000000000000, 5.850816112169488825 ) ) ;
#45343 = CARTESIAN_POINT ( 'NONE',  ( -69.95828321977570852, 0.4135283891523413025, -7.500828395702385798 ) ) ;
#45344 = PLANE ( 'NONE',  #17635 ) ;
#45345 = CARTESIAN_POINT ( 'NONE',  ( -17.43559644546093779, 0.000000000000000000, 9.855368259716744461 ) ) ;
#45346 = CARTESIAN_POINT ( 'NONE',  ( -14.01545677930355183, 0.000000000000000000, 2.126011111488108174 ) ) ;
#45347 = DIRECTION ( 'NONE',  ( 0.000000000000000000, -0.000000000000000000, -1.000000000000000000 ) ) ;
#45348 = CARTESIAN_POINT ( 'NONE',  ( -14.69713173337877166, 0.1245042932765033361, 2.794518955481596567 ) ) ;
#45349 = ORIENTED_EDGE ( 'NONE', *, *, #50318, .F. ) ;
#45350 = ADVANCED_FACE ( 'NONE', ( #25245 ), #11330, .F. ) ;
#45351 = ORIENTED_EDGE ( 'NONE', *, *, #44539, .T. ) ;
#45352 = ORIENTED_EDGE ( 'NONE', *, *, #16464, .T. ) ;
#45353 = ORIENTED_EDGE ( 'NONE', *, *, #55921, .T. ) ;
#45354 = EDGE_CURVE ( 'NONE', #19918, #47531, #45983, .T. ) ;
#45355 = EDGE_LOOP ( 'NONE', ( #29788, #55946, #50744, #24224 ) ) ;
#45356 = DIRECTION ( 'NONE',  ( 0.007781995580012663651, -3.146120232559066537E-19, -0.9999697198139514409 ) ) ;
#45357 = EDGE_CURVE ( 'NONE', #23572, #21327, #7090, .T. ) ;
#45358 = CARTESIAN_POINT ( 'NONE',  ( -10.86137571651779510, 0.000000000000000000, 1.000553606503651771 ) ) ;
#45359 = VERTEX_POINT ( 'NONE', #16414 ) ;
#45360 = FACE_OUTER_BOUND ( 'NONE', #20857, .T. ) ;
#45361 = ADVANCED_FACE ( 'NONE', ( #46509 ), #42281, .F. ) ;
#45362 = ORIENTED_EDGE ( 'NONE', *, *, #42502, .T. ) ;
#45363 = ORIENTED_EDGE ( 'NONE', *, *, #32558, .F. ) ;
#45364 = VECTOR ( 'NONE', #27993, 1000.000000000000227 ) ;
#45365 = PLANE ( 'NONE',  #20182 ) ;
#45366 = DIRECTION ( 'NONE',  ( 0.000000000000000000, -0.000000000000000000, -1.000000000000000000 ) ) ;
#45367 = CARTESIAN_POINT ( 'NONE',  ( -16.96233738810400737, 0.000000000000000000, 8.751055061711459970 ) ) ;
#45368 = ORIENTED_EDGE ( 'NONE', *, *, #27316, .F. ) ;
#45369 = CARTESIAN_POINT ( 'NONE',  ( -11.92213221946999724, 2.876837460659007473, 6.233662532057125283 ) ) ;
#45370 = LINE ( 'NONE', #25222, #27313 ) ;
#45371 = LINE ( 'NONE', #5641, #5783 ) ;
#45372 = CARTESIAN_POINT ( 'NONE',  ( -18.16068458728576118, 0.000000000000000000, 9.311067372743988102 ) ) ;
#45373 = LINE ( 'NONE', #33180, #33289 ) ;
#45374 = DIRECTION ( 'NONE',  ( -0.9999697198139514409, -0.000000000000000000, -0.007781995580013368816 ) ) ;
#45375 = LINE ( 'NONE', #6490, #41989 ) ;
#45376 = DIRECTION ( 'NONE',  ( 0.000000000000000000, -1.000000000000000000, 0.000000000000000000 ) ) ;
#45377 = DIRECTION ( 'NONE',  ( -0.5449076811759708816, 0.6444004775717707689, 0.5364919789714475140 ) ) ;
#45378 = ORIENTED_EDGE ( 'NONE', *, *, #23980, .F. ) ;
#45379 = LINE ( 'NONE', #32360, #38293 ) ;
#45380 = VERTEX_POINT ( 'NONE', #41972 ) ;
#45381 = ADVANCED_FACE ( 'NONE', ( #12475 ), #16710, .F. ) ;
#45382 = LINE ( 'NONE', #6496, #26551 ) ;
#45383 = DIRECTION ( 'NONE',  ( 0.5449076811759707706, 0.6444004775717708799, -0.5364919789714476250 ) ) ;
#45384 = LINE ( 'NONE', #46731, #14054 ) ;
#45385 = CARTESIAN_POINT ( 'NONE',  ( -11.20636620717317378, 0.000000000000000000, 11.32298014792380414 ) ) ;
#45386 = DIRECTION ( 'NONE',  ( 0.9999697198139515519, 0.000000000000000000, 0.007781995580013368816 ) ) ;
#45387 = DIRECTION ( 'NONE',  ( -0.005961354470445682716, -0.6427876096865404731, 0.7660212471507180654 ) ) ;
#45388 = ADVANCED_FACE ( 'NONE', ( #50779 ), #37748, .F. ) ;
#45389 = EDGE_CURVE ( 'NONE', #33376, #30431, #11873, .T. ) ;
#45390 = LINE ( 'NONE', #6502, #35239 ) ;
#45391 = DIRECTION ( 'NONE',  ( -0.005961354470445682716, -0.6427876096865404731, 0.7660212471507180654 ) ) ;
#45392 = CARTESIAN_POINT ( 'NONE',  ( -6.170713071148341555, -0.3214166768897696591, 3.252606517456513302E-16 ) ) ;
#45393 = CARTESIAN_POINT ( 'NONE',  ( -21.59278666343760733, 5.467268677019012202, 14.24141207810885668 ) ) ;
#45394 = CARTESIAN_POINT ( 'NONE',  ( -21.42872037518206696, -2.784623065533158304, 9.575615298689720944 ) ) ;
#45395 = FACE_OUTER_BOUND ( 'NONE', #51595, .T. ) ;
#45396 = CARTESIAN_POINT ( 'NONE',  ( -15.91085239395617634, -0.1191753592594211320, 5.904584430724759692 ) ) ;
#45397 = DIRECTION ( 'NONE',  ( 0.000000000000000000, -0.000000000000000000, -1.000000000000000000 ) ) ;
#45398 = VECTOR ( 'NONE', #1160, 999.9999999999998863 ) ;
#45399 = LINE ( 'NONE', #31539, #26414 ) ;
#45400 = DIRECTION ( 'NONE',  ( -0.5449076811759708816, 0.6444004775717707689, 0.5364919789714475140 ) ) ;
#45401 = LINE ( 'NONE', #6513, #44061 ) ;
#45402 = CARTESIAN_POINT ( 'NONE',  ( -18.23586646982717951, 4.333955019861511992, 3.627085705124660997 ) ) ;
#45403 = EDGE_CURVE ( 'NONE', #6183, #2694, #34041, .T. ) ;
#45404 = ORIENTED_EDGE ( 'NONE', *, *, #22246, .T. ) ;
#45405 = AXIS2_PLACEMENT_3D ( 'NONE', #15940, #46293, #8249 ) ;
#45406 = LINE ( 'NONE', #37174, #33976 ) ;
#45407 = VERTEX_POINT ( 'NONE', #29792 ) ;
#45408 = CARTESIAN_POINT ( 'NONE',  ( 2.072287782118878319, 0.000000000000000000, -2.950529333540147015 ) ) ;
#45409 = PLANE ( 'NONE',  #31267 ) ;
#45410 = ORIENTED_EDGE ( 'NONE', *, *, #37111, .T. ) ;
#45411 = PLANE ( 'NONE',  #42200 ) ;
#45412 = ORIENTED_EDGE ( 'NONE', *, *, #10507, .T. ) ;
#45413 = FACE_OUTER_BOUND ( 'NONE', #46788, .T. ) ;
#45414 = ORIENTED_EDGE ( 'NONE', *, *, #5917, .F. ) ;
#45415 = ORIENTED_EDGE ( 'NONE', *, *, #34688, .F. ) ;
#45416 = ORIENTED_EDGE ( 'NONE', *, *, #42309, .F. ) ;
#45417 = CARTESIAN_POINT ( 'NONE',  ( -22.40634380310664397, 0.000000000000000000, 5.584705972946605534 ) ) ;
#45418 = CARTESIAN_POINT ( 'NONE',  ( -21.93567466420777379, 19.99370817364452790, -4.408991681665293427 ) ) ;
#45419 = CARTESIAN_POINT ( 'NONE',  ( -17.75008747281315280, -0.1166911823299055240, 3.676363194284736124 ) ) ;
#45420 = VECTOR ( 'NONE', #8474, 999.9999999999998863 ) ;
#45421 = AXIS2_PLACEMENT_3D ( 'NONE', #50457, #40818, #11263 ) ;
#45422 = VERTEX_POINT ( 'NONE', #55068 ) ;
#45423 = EDGE_CURVE ( 'NONE', #11772, #36118, #47089, .T. ) ;
#45424 = EDGE_LOOP ( 'NONE', ( #24789, #21375, #37074, #27151 ) ) ;
#45425 = LINE ( 'NONE', #20138, #28202 ) ;
#45426 = EDGE_LOOP ( 'NONE', ( #584, #19641, #18352, #21215 ) ) ;
#45427 = CARTESIAN_POINT ( 'NONE',  ( -16.74090741521495929, 0.000000000000000000, 5.998127778728137294 ) ) ;
#45428 = ORIENTED_EDGE ( 'NONE', *, *, #34854, .T. ) ;
#45429 = DIRECTION ( 'NONE',  ( 0.005961354470445682716, -0.6427876096865404731, -0.7660212471507180654 ) ) ;
#45430 = FACE_OUTER_BOUND ( 'NONE', #49774, .T. ) ;
#45431 = EDGE_CURVE ( 'NONE', #52348, #39606, #15571, .T. ) ;
#45432 = ORIENTED_EDGE ( 'NONE', *, *, #1140, .F. ) ;
#45433 = VECTOR ( 'NONE', #41417, 1000.000000000000114 ) ;
#45434 = CARTESIAN_POINT ( 'NONE',  ( -27.22333567087903461, 16.65220053346459750, 4.407440554554201917 ) ) ;
#45435 = ADVANCED_FACE ( 'NONE', ( #50523 ), #20701, .F. ) ;
#45436 = EDGE_CURVE ( 'NONE', #18658, #1854, #51057, .T. ) ;
#45437 = AXIS2_PLACEMENT_3D ( 'NONE', #53385, #19847, #54464 ) ;
#45438 = DIRECTION ( 'NONE',  ( 0.007781995580012662783, 0.000000000000000000, -0.9999697198139514409 ) ) ;
#45439 = ORIENTED_EDGE ( 'NONE', *, *, #8058, .T. ) ;
#45440 = CARTESIAN_POINT ( 'NONE',  ( -14.00280974873554030, 0.000000000000000000, 12.40921378708904044 ) ) ;
#45441 = CARTESIAN_POINT ( 'NONE',  ( -22.40556560354864146, -0.1191753592594197858, 5.484709000965211523 ) ) ;
#45442 = CARTESIAN_POINT ( 'NONE',  ( -15.40103151951671734, 0.000000000000000000, 12.95233060667165681 ) ) ;
#45443 = EDGE_CURVE ( 'NONE', #38354, #55994, #46232, .T. ) ;
#45444 = ORIENTED_EDGE ( 'NONE', *, *, #43077, .T. ) ;
#45445 = EDGE_CURVE ( 'NONE', #24462, #41178, #32904, .T. ) ;
#45446 = DIRECTION ( 'NONE',  ( 0.000000000000000000, -0.000000000000000000, -1.000000000000000000 ) ) ;
#45447 = DIRECTION ( 'NONE',  ( -0.7660212471507179544, -0.6427876096865405842, -0.005961354470445141482 ) ) ;
#45448 = DIRECTION ( 'NONE',  ( 0.005961354470445682716, -0.6427876096865404731, -0.7660212471507180654 ) ) ;
#45449 = DIRECTION ( 'NONE',  ( 0.005002170337468016433, -0.7660444431189770143, -0.6427681459581293666 ) ) ;
#45450 = DIRECTION ( 'NONE',  ( -0.9999697198139514409, -0.000000000000000000, -0.007781995580013368816 ) ) ;
#45451 = EDGE_CURVE ( 'NONE', #40926, #50934, #34326, .T. ) ;
#45452 = DIRECTION ( 'NONE',  ( 0.5364919789714477361, 0.6444004775717706579, 0.5449076811759711036 ) ) ;
#45453 = CARTESIAN_POINT ( 'NONE',  ( -64.59009247688742050, -11.11452349097115366, 0.8132580553616088892 ) ) ;
#45454 = ORIENTED_EDGE ( 'NONE', *, *, #31253, .T. ) ;
#45455 = DIRECTION ( 'NONE',  ( -0.005961354470445682716, -0.6427876096865404731, 0.7660212471507180654 ) ) ;
#45456 = LINE ( 'NONE', #19643, #37668 ) ;
#45457 = CARTESIAN_POINT ( 'NONE',  ( -66.62196108082586932, 2.602085213965210642E-15, -5.205015551671701601 ) ) ;
#45458 = ORIENTED_EDGE ( 'NONE', *, *, #39415, .T. ) ;
#45459 = PLANE ( 'NONE',  #50129 ) ;
#45460 = DIRECTION ( 'NONE',  ( 0.5449076811759707706, 0.6444004775717708799, -0.5364919789714476250 ) ) ;
#45461 = EDGE_CURVE ( 'NONE', #29027, #46912, #34583, .T. ) ;
#45462 = AXIS2_PLACEMENT_3D ( 'NONE', #21483, #26030, #12941 ) ;
#45463 = VECTOR ( 'NONE', #30672, 1000.000000000000114 ) ;
#45464 = CARTESIAN_POINT ( 'NONE',  ( -18.65485795953289028, -2.298917212465660054, 4.054153975076401295 ) ) ;
#45465 = DIRECTION ( 'NONE',  ( -0.7660212471507179544, -0.6427876096865405842, -0.005961354470445141482 ) ) ;
#45466 = FACE_OUTER_BOUND ( 'NONE', #40570, .T. ) ;
#45467 = EDGE_CURVE ( 'NONE', #22414, #51971, #5070, .T. ) ;
#45468 = VERTEX_POINT ( 'NONE', #17554 ) ;
#45469 = VECTOR ( 'NONE', #22567, 999.9999999999998863 ) ;
#45470 = ORIENTED_EDGE ( 'NONE', *, *, #28773, .F. ) ;
#45471 = PLANE ( 'NONE',  #53129 ) ;
#45472 = LINE ( 'NONE', #5759, #32049 ) ;
#45473 = ORIENTED_EDGE ( 'NONE', *, *, #52470, .T. ) ;
#45474 = LINE ( 'NONE', #23904, #38551 ) ;
#45475 = ORIENTED_EDGE ( 'NONE', *, *, #37584, .F. ) ;
#45476 = DIRECTION ( 'NONE',  ( -0.7660212471507179544, -0.6427876096865405842, -0.005961354470445141482 ) ) ;
#45477 = VECTOR ( 'NONE', #26960, 1000.000000000000000 ) ;
#45478 = ORIENTED_EDGE ( 'NONE', *, *, #23129, .T. ) ;
#45479 = ORIENTED_EDGE ( 'NONE', *, *, #49650, .F. ) ;
#45480 = CARTESIAN_POINT ( 'NONE',  ( -15.06668613446144356, 2.229229656569007734, 2.463220195587470407 ) ) ;
#45481 = DIRECTION ( 'NONE',  ( -0.5449076811759708816, 0.6444004775717707689, 0.5364919789714475140 ) ) ;
#45482 = CARTESIAN_POINT ( 'NONE',  ( -11.24149099750305858, -0.1191753592594186895, 2.986265922342736356 ) ) ;
#45483 = ORIENTED_EDGE ( 'NONE', *, *, #45231, .T. ) ;
#45484 = LINE ( 'NONE', #49500, #12039 ) ;
#45485 = EDGE_CURVE ( 'NONE', #35767, #22808, #21552, .T. ) ;
#45486 = ORIENTED_EDGE ( 'NONE', *, *, #21152, .F. ) ;
#45487 = ORIENTED_EDGE ( 'NONE', *, *, #18134, .T. ) ;
#45488 = ORIENTED_EDGE ( 'NONE', *, *, #39448, .F. ) ;
#45489 = CARTESIAN_POINT ( 'NONE',  ( -17.59803301417029076, -3.756034771668160577, 9.681898340685158644 ) ) ;
#45490 = ORIENTED_EDGE ( 'NONE', *, *, #11508, .T. ) ;
#45491 = DIRECTION ( 'NONE',  ( 0.005961354470445682716, -0.6427876096865404731, -0.7660212471507180654 ) ) ;
#45492 = ORIENTED_EDGE ( 'NONE', *, *, #9103, .T. ) ;
#45493 = CARTESIAN_POINT ( 'NONE',  ( -8.509919637592204822, -0.1191753592594197858, 10.23596830920056711 ) ) ;
#45494 = DIRECTION ( 'NONE',  ( 0.005002170337468016433, -0.7660444431189770143, -0.6427681459581293666 ) ) ;
#45495 = VECTOR ( 'NONE', #47289, 999.9999999999998863 ) ;
#45496 = AXIS2_PLACEMENT_3D ( 'NONE', #13422, #5187, #4599 ) ;
#45497 = ORIENTED_EDGE ( 'NONE', *, *, #13209, .F. ) ;
#45498 = LINE ( 'NONE', #6617, #49491 ) ;
#45499 = VERTEX_POINT ( 'NONE', #30640 ) ;
#45500 = EDGE_CURVE ( 'NONE', #48900, #20306, #30884, .T. ) ;
#45501 = LINE ( 'NONE', #11148, #1977 ) ;
#45502 = CARTESIAN_POINT ( 'NONE',  ( -14.46888367232926420, 0.000000000000000000, 12.59025272694991315 ) ) ;
#45503 = VECTOR ( 'NONE', #35120, 1000.000000000000227 ) ;
#45504 = DIRECTION ( 'NONE',  ( 0.6427681459581294776, -0.7660444431189769032, 0.005002170337467562802 ) ) ;
#45505 = CARTESIAN_POINT ( 'NONE',  ( -19.10263103866113354, 2.553033558614007603, 8.491394756296369195 ) ) ;
#45506 = CARTESIAN_POINT ( 'NONE',  ( -12.48530657876094985, 3.038739411681508518, 1.434697112697735255 ) ) ;
#45507 = DIRECTION ( 'NONE',  ( -0.6427681459581293666, -0.7660444431189770143, -0.005002170337467561935 ) ) ;
#45508 =( LENGTH_UNIT ( ) NAMED_UNIT ( * ) SI_UNIT ( .MILLI., .METRE. ) );
#45509 = ORIENTED_EDGE ( 'NONE', *, *, #4451, .F. ) ;
#45510 = VERTEX_POINT ( 'NONE', #30054 ) ;
#45511 = EDGE_CURVE ( 'NONE', #41874, #13391, #47941, .T. ) ;
#45512 = CARTESIAN_POINT ( 'NONE',  ( -56.15805904048855979, 3.811595058059581209, 2.044864594757502818 ) ) ;
#45513 = LINE ( 'NONE', #3207, #48462 ) ;
#45514 = VECTOR ( 'NONE', #45948, 999.9999999999998863 ) ;
#45515 = CARTESIAN_POINT ( 'NONE',  ( -11.24723910451362485, -0.1191753592594192307, 3.724885328858265954 ) ) ;
#45516 = VECTOR ( 'NONE', #20221, 1000.000000000000000 ) ;
#45517 = ADVANCED_FACE ( 'NONE', ( #39128 ), #8783, .F. ) ;
#45518 = LINE ( 'NONE', #23412, #17927 ) ;
#45519 = CARTESIAN_POINT ( 'NONE',  ( -18.12463954610636563, 0.000000000000000000, 4.679356989688026935 ) ) ;
#45520 = ORIENTED_EDGE ( 'NONE', *, *, #21478, .F. ) ;
#45521 = CARTESIAN_POINT ( 'NONE',  ( -15.98995279184259388, 0.000000000000000000, 3.218641336381011353 ) ) ;
#45522 = DIRECTION ( 'NONE',  ( 0.000000000000000000, -0.000000000000000000, -1.000000000000000000 ) ) ;
#45523 = EDGE_LOOP ( 'NONE', ( #20623, #49074, #20192, #35443 ) ) ;
#45524 = LINE ( 'NONE', #29055, #6647 ) ;
#45525 = DIRECTION ( 'NONE',  ( -0.7660212471507179544, -0.6427876096865405842, -0.005961354470445141482 ) ) ;
#45526 = VERTEX_POINT ( 'NONE', #12732 ) ;
#45527 = EDGE_CURVE ( 'NONE', #873, #26892, #43401, .T. ) ;
#45528 = CARTESIAN_POINT ( 'NONE',  ( -69.30403031588791407, -1.000000000000000222, -6.450409451741321298 ) ) ;
#45529 = FACE_OUTER_BOUND ( 'NONE', #26270, .T. ) ;
#45530 = CARTESIAN_POINT ( 'NONE',  ( -12.60458797795435615, 0.000000000000000000, 11.86609696750642229 ) ) ;
#45531 = CARTESIAN_POINT ( 'NONE',  ( -20.54049170961573267, 0.000000000000000000, 4.660556269540326646 ) ) ;
#45532 = CARTESIAN_POINT ( 'NONE',  ( -58.00000000000000711, 8.000000000000000000, -2.749999999999994671 ) ) ;
#45533 = EDGE_CURVE ( 'NONE', #43351, #17923, #4500, .T. ) ;
#45534 = ORIENTED_EDGE ( 'NONE', *, *, #40906, .F. ) ;
#45535 = ORIENTED_EDGE ( 'NONE', *, *, #18097, .F. ) ;
#45536 = CARTESIAN_POINT ( 'NONE',  ( -12.33850799832341849, 0.000000000000000000, 11.68350162852954632 ) ) ;
#45537 = CARTESIAN_POINT ( 'NONE',  ( -9.962725746045613562, 0.000000000000000000, 4.942880946358983785 ) ) ;
#45538 = VECTOR ( 'NONE', #3065, 1000.000000000000000 ) ;
#45539 = DIRECTION ( 'NONE',  ( -0.3620778797217457656, 0.000000000000000000, -0.9321478471874539151 ) ) ;
#45540 = VECTOR ( 'NONE', #43806, 999.9999999999998863 ) ;
#45541 = CARTESIAN_POINT ( 'NONE',  ( -19.59569683186026268, 0.000000000000000000, 14.58168106541950948 ) ) ;
#45542 = AXIS2_PLACEMENT_3D ( 'NONE', #16394, #20685, #28920 ) ;
#45543 = CARTESIAN_POINT ( 'NONE',  ( -14.48163787323972684, -3.432230869623162928, 2.396974931197724423 ) ) ;
#45544 = DIRECTION ( 'NONE',  ( 0.007781995580012663651, 0.000000000000000000, -0.9999697198139515519 ) ) ;
#45545 = ORIENTED_EDGE ( 'NONE', *, *, #43466, .F. ) ;
#45546 = LINE ( 'NONE', #1823, #48289 ) ;
#45547 = PLANE ( 'NONE',  #6036 ) ;
#45548 = VECTOR ( 'NONE', #24335, 1000.000000000000227 ) ;
#45549 = CARTESIAN_POINT ( 'NONE',  ( -15.03495456790438389, -0.1191753592594197858, 12.77051346725278158 ) ) ;
#45550 = AXIS2_PLACEMENT_3D ( 'NONE', #40914, #33519, #45446 ) ;
#45551 = ORIENTED_EDGE ( 'NONE', *, *, #19874, .F. ) ;
#45552 = FACE_OUTER_BOUND ( 'NONE', #14937, .T. ) ;
#45553 = PLANE ( 'NONE',  #36828 ) ;
#45554 = EDGE_CURVE ( 'NONE', #11685, #9839, #34883, .T. ) ;
#45555 = DIRECTION ( 'NONE',  ( 0.000000000000000000, -1.000000000000000000, 0.000000000000000000 ) ) ;
#45556 = ORIENTED_EDGE ( 'NONE', *, *, #28012, .T. ) ;
#45557 = CARTESIAN_POINT ( 'NONE',  ( -16.16356523649682231, -2.622721114510657703, 7.264741553452760847 ) ) ;
#45558 = AXIS2_PLACEMENT_3D ( 'NONE', #25156, #34242, #25412 ) ;
#45559 = EDGE_CURVE ( 'NONE', #36400, #26435, #18110, .T. ) ;
#45560 = EDGE_LOOP ( 'NONE', ( #22947, #13146, #18332, #20712 ) ) ;
#45561 = ORIENTED_EDGE ( 'NONE', *, *, #12956, .F. ) ;
#45562 = ORIENTED_EDGE ( 'NONE', *, *, #26889, .T. ) ;
#45563 = EDGE_CURVE ( 'NONE', #45990, #29528, #52202, .T. ) ;
#45564 = ORIENTED_EDGE ( 'NONE', *, *, #19239, .T. ) ;
#45565 = EDGE_CURVE ( 'NONE', #48717, #31783, #43656, .T. ) ;
#45566 = VERTEX_POINT ( 'NONE', #48492 ) ;
#45567 = PLANE ( 'NONE',  #23875 ) ;
#45569 = ADVANCED_FACE ( 'NONE', ( #39424 ), #21247, .F. ) ;
#45568 = ORIENTED_EDGE ( 'NONE', *, *, #31886, .F. ) ;
#45570 = EDGE_CURVE ( 'NONE', #16052, #43303, #17858, .T. ) ;
#45571 = EDGE_CURVE ( 'NONE', #9917, #39727, #31858, .T. ) ;
#45572 = ORIENTED_EDGE ( 'NONE', *, *, #29591, .F. ) ;
#45573 = DIRECTION ( 'NONE',  ( 0.5364919789714477361, 0.6444004775717706579, 0.5449076811759711036 ) ) ;
#45574 = ORIENTED_EDGE ( 'NONE', *, *, #6342, .F. ) ;
#45575 = VECTOR ( 'NONE', #50653, 999.9999999999998863 ) ;
#45576 = ORIENTED_EDGE ( 'NONE', *, *, #47172, .T. ) ;
#45577 = ORIENTED_EDGE ( 'NONE', *, *, #27782, .T. ) ;
#45578 = PLANE ( 'NONE',  #8543 ) ;
#45579 = CARTESIAN_POINT ( 'NONE',  ( -10.00813838035478298, 0.000000000000000000, 10.77830692922518452 ) ) ;
#45580 = PLANE ( 'NONE',  #44102 ) ;
#45581 = CARTESIAN_POINT ( 'NONE',  ( -13.08330893211609869, 0.000000000000000000, 1.763933231766363630 ) ) ;
#45582 = VECTOR ( 'NONE', #32771, 999.9999999999998863 ) ;
#45583 = ORIENTED_EDGE ( 'NONE', *, *, #12676, .F. ) ;
#45584 = CARTESIAN_POINT ( 'NONE',  ( -11.21979143729918960, -0.1191753592594197858, 1.139774444304266554 ) ) ;
#45585 = EDGE_LOOP ( 'NONE', ( #15495, #50936, #4205, #20708 ) ) ;
#45586 = VECTOR ( 'NONE', #49111, 1000.000000000000227 ) ;
#45587 = VECTOR ( 'NONE', #18366, 1000.000000000000000 ) ;
#45588 = ORIENTED_EDGE ( 'NONE', *, *, #11401, .F. ) ;
#45589 = EDGE_CURVE ( 'NONE', #40704, #53976, #3924, .T. ) ;
#45590 = FACE_OUTER_BOUND ( 'NONE', #17318, .T. ) ;
#45591 = EDGE_CURVE ( 'NONE', #5666, #18978, #26629, .T. ) ;
#45592 = CARTESIAN_POINT ( 'NONE',  ( -37.34829856057490360, 11.09522561815848007, -4.928657742077421133 ) ) ;
#45593 = VECTOR ( 'NONE', #48732, 999.9999999999998863 ) ;
#45594 = AXIS2_PLACEMENT_3D ( 'NONE', #53023, #9289, #23218 ) ;
#45595 = CARTESIAN_POINT ( 'NONE',  ( -13.13096402496594983, 3.200641362704009119, 7.234631225313592928 ) ) ;
#45596 = EDGE_CURVE ( 'NONE', #51597, #34934, #14691, .T. ) ;
#45597 = DIRECTION ( 'NONE',  ( -0.005002170337468016433, -0.7660444431189770143, 0.6427681459581293666 ) ) ;
#45598 = LINE ( 'NONE', #36833, #1392 ) ;
#45599 = VERTEX_POINT ( 'NONE', #41081 ) ;
#45600 = LINE ( 'NONE', #24034, #3876 ) ;
#45601 = ORIENTED_EDGE ( 'NONE', *, *, #37510, .F. ) ;
#45602 = ADVANCED_FACE ( 'NONE', ( #32312 ), #18687, .F. ) ;
#45603 = DIRECTION ( 'NONE',  ( 0.7660212471507180654, -0.6427876096865404731, 0.005961354470445141482 ) ) ;
#45604 = PLANE ( 'NONE',  #37778 ) ;
#45605 = CARTESIAN_POINT ( 'NONE',  ( -10.24173896645031867, 0.000000000000000000, 6.787369949995797569 ) ) ;
#45606 = VECTOR ( 'NONE', #8519, 999.9999999999998863 ) ;
#45607 = CARTESIAN_POINT ( 'NONE',  ( -58.00000000000000711, 0.000000000000000000, 7.102951435054649637E-15 ) ) ;
#45608 = VECTOR ( 'NONE', #50173, 1000.000000000000114 ) ;
#45609 = DIRECTION ( 'NONE',  ( -0.5364919789714478471, 0.6444004775717705469, -0.5449076811759709926 ) ) ;
#45610 = ORIENTED_EDGE ( 'NONE', *, *, #21050, .T. ) ;
#45611 = CARTESIAN_POINT ( 'NONE',  ( -11.15951654611136057, 0.000000000000000000, 5.302899313428722117 ) ) ;
#45612 = FACE_OUTER_BOUND ( 'NONE', #51926, .T. ) ;
#45613 = DIRECTION ( 'NONE',  ( 0.005002170337468016433, -0.7660444431189770143, -0.6427681459581293666 ) ) ;
#45614 = VECTOR ( 'NONE', #31204, 1000.000000000000114 ) ;
#45615 = DIRECTION ( 'NONE',  ( 0.000000000000000000, 1.000000000000000000, 0.000000000000000000 ) ) ;
#45616 = CARTESIAN_POINT ( 'NONE',  ( -29.93654370153088706, -1.000000000000000000, 22.35628214185738116 ) ) ;
#45617 = AXIS2_PLACEMENT_3D ( 'NONE', #36984, #24451, #54279 ) ;
#45618 = LINE ( 'NONE', #28040, #23660 ) ;
#45619 = CARTESIAN_POINT ( 'NONE',  ( -10.82493838822988153, -0.1941918491731542684, 1.079899066930483320 ) ) ;
#45620 = CARTESIAN_POINT ( 'NONE',  ( -17.26532721389163072, 0.000000000000000000, 13.67648636611514590 ) ) ;
#45621 = AXIS2_PLACEMENT_3D ( 'NONE', #51702, #9, #4851 ) ;
#45622 = FACE_OUTER_BOUND ( 'NONE', #22030, .T. ) ;
#45623 = VECTOR ( 'NONE', #17478, 1000.000000000000000 ) ;
#45624 = VECTOR ( 'NONE', #47989, 999.9999999999998863 ) ;
#45625 = EDGE_LOOP ( 'NONE', ( #19796, #45230, #39826, #52756 ) ) ;
#45626 = VECTOR ( 'NONE', #5692, 999.9999999999998863 ) ;
#45627 = EDGE_LOOP ( 'NONE', ( #17152, #15672, #48928, #12601 ) ) ;
#45628 = VERTEX_POINT ( 'NONE', #36852 ) ;
#45629 = AXIS2_PLACEMENT_3D ( 'NONE', #6574, #20756, #38071 ) ;
#45630 = ORIENTED_EDGE ( 'NONE', *, *, #52659, .T. ) ;
#45631 = ORIENTED_EDGE ( 'NONE', *, *, #53852, .F. ) ;
#45632 = DIRECTION ( 'NONE',  ( 0.007781995580012663651, -3.146120232559066537E-19, -0.9999697198139514409 ) ) ;
#45633 = CARTESIAN_POINT ( 'NONE',  ( -15.45483765763093764, -0.1191753592594179401, 7.016129452266057775 ) ) ;
#45634 = ADVANCED_FACE ( 'NONE', ( #19505 ), #14154, .F. ) ;
#45635 = EDGE_CURVE ( 'NONE', #13109, #4654, #10448, .T. ) ;
#45636 = EDGE_LOOP ( 'NONE', ( #5088, #20087 ) ) ;
#45637 = LINE ( 'NONE', #41404, #45765 ) ;
#45638 = EDGE_LOOP ( 'NONE', ( #37590, #48473, #13611, #46776 ) ) ;
#45639 = ADVANCED_FACE ( 'NONE', ( #44793 ), #31741, .F. ) ;
#45640 = ORIENTED_EDGE ( 'NONE', *, *, #51842, .T. ) ;
#45641 = CARTESIAN_POINT ( 'NONE',  ( -65.90562112943153750, -9.252273468653816835, -0.3573205173235035614 ) ) ;
#45642 = DIRECTION ( 'NONE',  ( 0.007781995580012662783, 0.000000000000000000, -0.9999697198139514409 ) ) ;
#45643 = LINE ( 'NONE', #6763, #28663 ) ;
#45644 = EDGE_LOOP ( 'NONE', ( #5691, #12148, #37966, #7351 ) ) ;
#45645 = LINE ( 'NONE', #45369, #29186 ) ;
#45646 = VECTOR ( 'NONE', #14125, 1000.000000000000227 ) ;
#45647 = DIRECTION ( 'NONE',  ( 0.6427681459581294776, -0.7660444431189769032, 0.005002170337467562802 ) ) ;
#45649 = VECTOR ( 'NONE', #42900, 999.9999999999998863 ) ;
#45648 = LINE ( 'NONE', #20926, #52019 ) ;
#45650 = EDGE_CURVE ( 'NONE', #32512, #1529, #1668, .T. ) ;
#45651 = PLANE ( 'NONE',  #51693 ) ;
#45652 = LINE ( 'NONE', #41418, #27865 ) ;
#45653 = CARTESIAN_POINT ( 'NONE',  ( -11.64304826722810660, 25.38767603887884050, 5.000000000059520389 ) ) ;
#45654 = FACE_OUTER_BOUND ( 'NONE', #748, .T. ) ;
#45655 = CARTESIAN_POINT ( 'NONE',  ( -17.76365187430995718, -0.1191753592594196748, 5.151501377137190474 ) ) ;
#45656 = EDGE_CURVE ( 'NONE', #9765, #34966, #22655, .T. ) ;
#45657 = AXIS2_PLACEMENT_3D ( 'NONE', #5552, #27712, #39361 ) ;
#45658 = DIRECTION ( 'NONE',  ( 0.005002170337468016433, -0.7660444431189770143, -0.6427681459581293666 ) ) ;
#45659 = EDGE_LOOP ( 'NONE', ( #49186, #15025, #14615, #28842 ) ) ;
#45660 = CARTESIAN_POINT ( 'NONE',  ( -10.00813838035478298, 0.000000000000000000, 10.77830692922518452 ) ) ;
#45661 = ORIENTED_EDGE ( 'NONE', *, *, #5348, .F. ) ;
#45662 = VECTOR ( 'NONE', #28778, 1000.000000000000227 ) ;
#45663 = VECTOR ( 'NONE', #22391, 1000.000000000000227 ) ;
#45664 = ADVANCED_FACE ( 'NONE', ( #39967 ), #23757, .F. ) ;
#45665 = CARTESIAN_POINT ( 'NONE',  ( -26.13337879274045505, 0.000000000000000000, 6.833023547870798353 ) ) ;
#45666 = LINE ( 'NONE', #6237, #21407 ) ;
#45667 = DIRECTION ( 'NONE',  ( 0.005961354470445682716, -0.6427876096865404731, -0.7660212471507180654 ) ) ;
#45668 = FACE_OUTER_BOUND ( 'NONE', #50305, .T. ) ;
#45669 = DIRECTION ( 'NONE',  ( 0.005002170337468016433, -0.7660444431189770143, -0.6427681459581293666 ) ) ;
#45670 = EDGE_CURVE ( 'NONE', #42137, #713, #53859, .T. ) ;
#45671 = AXIS2_PLACEMENT_3D ( 'NONE', #48444, #42568, #55342 ) ;
#45672 = DIRECTION ( 'NONE',  ( -0.2588190451025176864, -0.9659258262890692004, 0.000000000000000000 ) ) ;
#45673 = AXIS2_PLACEMENT_3D ( 'NONE', #40314, #19012, #27837 ) ;
#45674 = LINE ( 'NONE', #31533, #19268 ) ;
#45675 = CARTESIAN_POINT ( 'NONE',  ( -15.56842669758074571, 0.000000000000000000, 8.761902797015491018 ) ) ;
#45676 = PLANE ( 'NONE',  #23131 ) ;
#45677 = CARTESIAN_POINT ( 'NONE',  ( -20.54126990917373519, -0.1191753592594197858, 4.760553241521720658 ) ) ;
#45678 = CARTESIAN_POINT ( 'NONE',  ( -9.858694684501937644, -9.497542338669614281, 0.6110782424775126342 ) ) ;
#45679 = CARTESIAN_POINT ( 'NONE',  ( -19.45503627000849889, -1.000000000000000000, 7.556996783084074742 ) ) ;
#45680 = FACE_OUTER_BOUND ( 'NONE', #31268, .T. ) ;
#45681 = DIRECTION ( 'NONE',  ( -0.5364919789714478471, 0.6444004775717705469, -0.5449076811759709926 ) ) ;
#45682 = CARTESIAN_POINT ( 'NONE',  ( -20.54049170961573267, 0.000000000000000000, 4.660556269540326646 ) ) ;
#45683 = ORIENTED_EDGE ( 'NONE', *, *, #32776, .T. ) ;
#45684 = CARTESIAN_POINT ( 'NONE',  ( -18.39746900504187010, 0.000000000000000000, 14.03700784672088808 ) ) ;
#45685 = ORIENTED_EDGE ( 'NONE', *, *, #12676, .T. ) ;
#45686 = AXIS2_PLACEMENT_3D ( 'NONE', #26181, #33847, #38692 ) ;
#45687 = DIRECTION ( 'NONE',  ( -0.5449076811759708816, 0.6444004775717707689, 0.5364919789714475140 ) ) ;
#45688 = CARTESIAN_POINT ( 'NONE',  ( -16.06709938707323460, 0.000000000000000000, 13.13181314741652628 ) ) ;
#45689 = VECTOR ( 'NONE', #30547, 1000.000000000000000 ) ;
#45690 = VERTEX_POINT ( 'NONE', #53037 ) ;
#45691 = VECTOR ( 'NONE', #52176, 1000.000000000000114 ) ;
#45692 = ORIENTED_EDGE ( 'NONE', *, *, #50006, .F. ) ;
#45693 = PLANE ( 'NONE',  #26581 ) ;
#45694 = EDGE_LOOP ( 'NONE', ( #4195, #37133, #18236, #36714 ) ) ;
#45695 = ORIENTED_EDGE ( 'NONE', *, *, #23918, .F. ) ;
#45696 = EDGE_LOOP ( 'NONE', ( #23106, #14788, #3731, #25673 ) ) ;
#45697 = CARTESIAN_POINT ( 'NONE',  ( -17.41416041653468127, 0.000000000000000000, 7.100884577617416760 ) ) ;
#45698 = VECTOR ( 'NONE', #9467, 999.9999999999998863 ) ;
#45699 = PLANE ( 'NONE',  #41359 ) ;
#45700 = DIRECTION ( 'NONE',  ( -0.9999697198139514409, -0.000000000000000000, -0.007781995580013368816 ) ) ;
#45701 = AXIS2_PLACEMENT_3D ( 'NONE', #36666, #49726, #10823 ) ;
#45702 = ADVANCED_FACE ( 'NONE', ( #53336 ), #9889, .F. ) ;
#45703 = EDGE_LOOP ( 'NONE', ( #32480, #1844, #37401, #17025 ) ) ;
#45704 = VERTEX_POINT ( 'NONE', #27468 ) ;
#45705 = EDGE_CURVE ( 'NONE', #33893, #4507, #1637, .T. ) ;
#45706 = EDGE_CURVE ( 'NONE', #40865, #40267, #49334, .T. ) ;
#45707 = VECTOR ( 'NONE', #22657, 1000.000000000000227 ) ;
#45708 = AXIS2_PLACEMENT_3D ( 'NONE', #17198, #25184, #11809 ) ;
#45709 = DIRECTION ( 'NONE',  ( -0.005002170337468016433, -0.7660444431189770143, 0.6427681459581293666 ) ) ;
#45710 = CARTESIAN_POINT ( 'NONE',  ( -16.81190032086591302, 0.000000000000000000, 3.212244750653343583 ) ) ;
#45711 = ORIENTED_EDGE ( 'NONE', *, *, #55792, .T. ) ;
#45712 = DIRECTION ( 'NONE',  ( 0.7660212471507180654, -0.6427876096865404731, 0.005961354470445141482 ) ) ;
#45713 = ORIENTED_EDGE ( 'NONE', *, *, #38698, .F. ) ;
#45714 = CARTESIAN_POINT ( 'NONE',  ( -15.22089569151837196, 4.010151117816510791, 9.374975078733013945 ) ) ;
#45715 = DIRECTION ( 'NONE',  ( 0.5449076811759707706, 0.6444004775717708799, -0.5364919789714476250 ) ) ;
#45716 = ORIENTED_EDGE ( 'NONE', *, *, #45101, .F. ) ;
#45717 = FACE_OUTER_BOUND ( 'NONE', #10996, .T. ) ;
#45718 = VECTOR ( 'NONE', #16064, 1000.000000000000114 ) ;
#45719 = DIRECTION ( 'NONE',  ( 0.5364919789714477361, 0.6444004775717706579, 0.5449076811759711036 ) ) ;
#45720 = EDGE_LOOP ( 'NONE', ( #37768, #52827, #32409, #23103 ) ) ;
#45721 = DIRECTION ( 'NONE',  ( -0.7660212471507179544, -0.6427876096865405842, -0.005961354470445141482 ) ) ;
#45723 = AXIS2_PLACEMENT_3D ( 'NONE', #29621, #38389, #20790 ) ;
#45722 = SURFACE_SIDE_STYLE ('',( #28976 ) ) ;
#45724 = LINE ( 'NONE', #33259, #50079 ) ;
#45725 = ORIENTED_EDGE ( 'NONE', *, *, #24450, .T. ) ;
#45726 = VECTOR ( 'NONE', #48046, 999.9999999999998863 ) ;
#45727 = LINE ( 'NONE', #46566, #9281 ) ;
#45728 = PLANE ( 'NONE',  #27846 ) ;
#45729 = LINE ( 'NONE', #42028, #21260 ) ;
#45730 = B_SPLINE_CURVE_WITH_KNOTS ( 'NONE', 3,
 ( #3346, #37985, #55288, #16378, #33703, #51018, #12129, #29466, #46787, #44759, #31715, #35151, #761, #5034, #27430, #4735 ),
 .UNSPECIFIED., .F., .F.,
 ( 4, 2, 2, 2, 2, 2, 2, 4 ),
 ( 1.734723475976805554E-18, 0.0004228030555968900176, 0.0008456061111937783004, 0.001268409166790666637, 0.001691212222387554866, 0.002114015277984443095, 0.002536818333581331540, 0.003382424444775107997 ),
 .UNSPECIFIED. ) ;
#45731 = FACE_OUTER_BOUND ( 'NONE', #54502, .T. ) ;
#45732 = EDGE_CURVE ( 'NONE', #16069, #17592, #14978, .T. ) ;
#45733 = DIRECTION ( 'NONE',  ( 0.005002170337468016433, -0.7660444431189770143, -0.6427681459581293666 ) ) ;
#45734 = CARTESIAN_POINT ( 'NONE',  ( -16.24565193759350379, -1.651309408375659871, 3.138998618723810363 ) ) ;
#45735 = CARTESIAN_POINT ( 'NONE',  ( -68.36714757807160936, -11.54765427770263742, -6.539696485987661845 ) ) ;
#45736 = VECTOR ( 'NONE', #39881, 1000.000000000000227 ) ;
#45737 = EDGE_LOOP ( 'NONE', ( #23741, #56068, #11831, #4373 ) ) ;
#45738 = EDGE_CURVE ( 'NONE', #17790, #32862, #29428, .T. ) ;
#45739 = LINE ( 'NONE', #37503, #32246 ) ;
#45740 = CARTESIAN_POINT ( 'NONE',  ( -68.22318098944886344, -0.6012227279448117967, -5.285932311688715579 ) ) ;
#45741 = ORIENTED_EDGE ( 'NONE', *, *, #21133, .T. ) ;
#45742 = VECTOR ( 'NONE', #39731, 1000.000000000000114 ) ;
#45743 = DIRECTION ( 'NONE',  ( 0.6427681459581294776, -0.7660444431189769032, 0.005002170337467562802 ) ) ;
#45745 = ADVANCED_FACE ( 'NONE', ( #7027 ), #33416, .F. ) ;
#45744 = FACE_OUTER_BOUND ( 'NONE', #10289, .T. ) ;
#45746 = AXIS2_PLACEMENT_3D ( 'NONE', #36895, #45376, #11015 ) ;
#45747 = ADVANCED_FACE ( 'NONE', ( #16347 ), #51293, .F. ) ;
#45748 = CARTESIAN_POINT ( 'NONE',  ( -15.96710241509184058, -0.1191753592594218814, 13.13259134697452879 ) ) ;
#45749 = DIRECTION ( 'NONE',  ( 0.005002170337468016433, -0.7660444431189770143, -0.6427681459581293666 ) ) ;
#45750 = CARTESIAN_POINT ( 'NONE',  ( -9.936859264498066224, 0.000000000000000000, 1.619093617039103039 ) ) ;
#45751 = ORIENTED_EDGE ( 'NONE', *, *, #54635, .F. ) ;
#45752 = AXIS2_PLACEMENT_3D ( 'NONE', #21107, #55465, #46117 ) ;
#45753 = VECTOR ( 'NONE', #26481, 999.9999999999998863 ) ;
#45754 = ORIENTED_EDGE ( 'NONE', *, *, #32289, .F. ) ;
#45755 = CARTESIAN_POINT ( 'NONE',  ( -25.85160320928759248, 17.67349956316208193, 4.606045228336897779 ) ) ;
#45756 = LINE ( 'NONE', #54841, #14825 ) ;
#45757 = VERTEX_POINT ( 'NONE', #41381 ) ;
#45758 = CARTESIAN_POINT ( 'NONE',  ( -69.66347483736342383, -8.676648739292067702, -7.503912900124009688 ) ) ;
#45759 = ORIENTED_EDGE ( 'NONE', *, *, #2887, .T. ) ;
#45760 = PLANE ( 'NONE',  #9310 ) ;
#45761 = EDGE_CURVE ( 'NONE', #47810, #9986, #33674, .T. ) ;
#45762 = VECTOR ( 'NONE', #15044, 999.9999999999998863 ) ;
#45763 = ORIENTED_EDGE ( 'NONE', *, *, #27439, .F. ) ;
#45764 = ORIENTED_EDGE ( 'NONE', *, *, #45571, .T. ) ;
#45765 = VECTOR ( 'NONE', #2490, 1000.000000000000000 ) ;
#45766 = FACE_OUTER_BOUND ( 'NONE', #35272, .T. ) ;
#45767 = ADVANCED_FACE ( 'NONE', ( #15797 ), #50453, .F. ) ;
#45768 = DIRECTION ( 'NONE',  ( 0.5364919789714477361, 0.6444004775717706579, 0.5449076811759711036 ) ) ;
#45769 = VECTOR ( 'NONE', #22577, 999.9999999999998863 ) ;
#45770 = LINE ( 'NONE', #54294, #43887 ) ;
#45771 = ORIENTED_EDGE ( 'NONE', *, *, #300, .T. ) ;
#45772 = DIRECTION ( 'NONE',  ( 0.5364919789714477361, 0.6444004775717706579, 0.5449076811759711036 ) ) ;
#45773 = EDGE_CURVE ( 'NONE', #34236, #43196, #7868, .T. ) ;
#45774 = VECTOR ( 'NONE', #18731, 1000.000000000000227 ) ;
#45775 = EDGE_LOOP ( 'NONE', ( #1532, #49863, #47119, #33455 ) ) ;
#45776 = EDGE_CURVE ( 'NONE', #8547, #11287, #16637, .T. ) ;
#45777 = ORIENTED_EDGE ( 'NONE', *, *, #39853, .T. ) ;
#45778 = ORIENTED_EDGE ( 'NONE', *, *, #19125, .F. ) ;
#45779 = VECTOR ( 'NONE', #35330, 1000.000000000000000 ) ;
#45780 = DIRECTION ( 'NONE',  ( -0.9999697198139514409, -0.000000000000000000, -0.007781995580013368816 ) ) ;
#45781 = VECTOR ( 'NONE', #3695, 1000.000000000000227 ) ;
#45782 = EDGE_LOOP ( 'NONE', ( #53869, #47355, #47785, #46386 ) ) ;
#45783 = VECTOR ( 'NONE', #23892, 1000.000000000000227 ) ;
#45784 = AXIS2_PLACEMENT_3D ( 'NONE', #46321, #40776, #53543 ) ;
#45785 = CARTESIAN_POINT ( 'NONE',  ( -32.65841372305263235, 0.000000000000000000, 9.367568705923016381 ) ) ;
#45786 = ORIENTED_EDGE ( 'NONE', *, *, #1719, .T. ) ;
#45787 = CARTESIAN_POINT ( 'NONE',  ( -18.39746900504187010, 0.000000000000000000, 14.03700784672088808 ) ) ;
#45788 = FACE_OUTER_BOUND ( 'NONE', #5891, .T. ) ;
#45789 = AXIS2_PLACEMENT_3D ( 'NONE', #39247, #4894, #22218 ) ;
#45790 = EDGE_LOOP ( 'NONE', ( #39602, #42223, #7113 ) ) ;
#45791 = PLANE ( 'NONE',  #15040 ) ;
#45792 = VERTEX_POINT ( 'NONE', #54999 ) ;
#45793 = EDGE_CURVE ( 'NONE', #16632, #16077, #28876, .T. ) ;
#45794 = AXIS2_PLACEMENT_3D ( 'NONE', #39200, #14767, #32098 ) ;
#45795 = DIRECTION ( 'NONE',  ( -0.005002170337468016433, -0.7660444431189770143, 0.6427681459581293666 ) ) ;
#45796 = VECTOR ( 'NONE', #24560, 1000.000000000000000 ) ;
#45797 = FACE_OUTER_BOUND ( 'NONE', #15223, .T. ) ;
#45798 = CARTESIAN_POINT ( 'NONE',  ( -12.38392586161602260, -3.108426967578159061, 6.593727315006988832 ) ) ;
#45799 = LINE ( 'NONE', #7452, #44746 ) ;
#45800 = LINE ( 'NONE', #28779, #10601 ) ;
#45801 = LINE ( 'NONE', #19955, #52755 ) ;
#45802 = ORIENTED_EDGE ( 'NONE', *, *, #2442, .T. ) ;
#45803 = ORIENTED_EDGE ( 'NONE', *, *, #11863, .F. ) ;
#45804 = CARTESIAN_POINT ( 'NONE',  ( -18.19747506107908563, 0.000000000000000000, 14.03856424583689311 ) ) ;
#45805 = PLANE ( 'NONE',  #5832 ) ;
#45806 = DIRECTION ( 'NONE',  ( -0.5364919789714478471, 0.6444004775717705469, -0.5449076811759709926 ) ) ;
#45807 = CARTESIAN_POINT ( 'NONE',  ( -13.33442604019040267, -2.622721114510660367, 1.977186495200478067 ) ) ;
#45808 = AXIS2_PLACEMENT_3D ( 'NONE', #28810, #46112, #7217 ) ;
#45809 = DIRECTION ( 'NONE',  ( 0.007781995580012662783, 0.000000000000000000, -0.9999697198139514409 ) ) ;
#45810 = ORIENTED_EDGE ( 'NONE', *, *, #49426, .T. ) ;
#45811 = AXIS2_PLACEMENT_3D ( 'NONE', #12694, #33696, #3605 ) ;
#45812 = DIRECTION ( 'NONE',  ( -0.5364919789714478471, 0.6444004775717705469, -0.5449076811759709926 ) ) ;
#45813 = CARTESIAN_POINT ( 'NONE',  ( -18.79657489303680507, 0.000000000000000000, 5.612798029282330070 ) ) ;
#45814 = EDGE_LOOP ( 'NONE', ( #38659, #48801, #28394, #36581 ) ) ;
#45815 = CARTESIAN_POINT ( 'NONE',  ( -12.33850799832341849, 0.000000000000000000, 11.68350162852954632 ) ) ;
#45816 = FACE_OUTER_BOUND ( 'NONE', #26166, .T. ) ;
#45817 = VECTOR ( 'NONE', #31150, 1000.000000000000114 ) ;
#45818 = ORIENTED_EDGE ( 'NONE', *, *, #10341, .F. ) ;
#45819 = PLANE ( 'NONE',  #42514 ) ;
#45820 = LINE ( 'NONE', #2648, #50499 ) ;
#45821 = EDGE_CURVE ( 'NONE', #46187, #23847, #25189, .T. ) ;
#45822 = AXIS2_PLACEMENT_3D ( 'NONE', #8757, #22635, #52713 ) ;
#45823 = CARTESIAN_POINT ( 'NONE',  ( -19.41483227295923797, -3.756034771668161909, 4.302864128261002286 ) ) ;
#45824 = FACE_OUTER_BOUND ( 'NONE', #21171, .T. ) ;
#45825 = CARTESIAN_POINT ( 'NONE',  ( -10.28842178966973897, 0.000000000000000000, 0.8776935365639153552 ) ) ;
#45826 = ORIENTED_EDGE ( 'NONE', *, *, #19417, .T. ) ;
#45827 = EDGE_CURVE ( 'NONE', #1558, #52378, #46175, .T. ) ;
#45828 = AXIS2_PLACEMENT_3D ( 'NONE', #16190, #24165, #37789 ) ;
#45829 = VECTOR ( 'NONE', #11446, 1000.000000000000114 ) ;
#45830 = ORIENTED_EDGE ( 'NONE', *, *, #45043, .T. ) ;
#45831 = CARTESIAN_POINT ( 'NONE',  ( -69.18094373452092327, -0.6002176455286792889, -6.959823595413027419 ) ) ;
#45832 = DIRECTION ( 'NONE',  ( 0.9999697198139515519, 0.000000000000000000, 0.007781995580013368816 ) ) ;
#45833 = FACE_OUTER_BOUND ( 'NONE', #8943, .T. ) ;
#45834 = VECTOR ( 'NONE', #32568, 1000.000000000000227 ) ;
#45835 = EDGE_CURVE ( 'NONE', #19669, #45947, #38212, .T. ) ;
#45836 = LINE ( 'NONE', #42132, #35711 ) ;
#45838 = LINE ( 'NONE', #23975, #55516 ) ;
#45837 = VECTOR ( 'NONE', #31504, 1000.000000000000114 ) ;
#45839 = LINE ( 'NONE', #53518, #2209 ) ;
#45841 = EDGE_CURVE ( 'NONE', #7759, #2042, #16094, .T. ) ;
#45840 = EDGE_LOOP ( 'NONE', ( #53203, #19160, #46988, #33665 ) ) ;
#45842 = CARTESIAN_POINT ( 'NONE',  ( 5.540715933951533501, -1.051609115606587652, -2.373726444132762570 ) ) ;
#45843 = ADVANCED_FACE ( 'NONE', ( #7278 ), #3004, .F. ) ;
#45844 = AXIS2_PLACEMENT_3D ( 'NONE', #25131, #42437, #33910 ) ;
#45845 = CARTESIAN_POINT ( 'NONE',  ( -15.72321562200438372, 5.143464774974011888, 11.43005398624366187 ) ) ;
#45846 = VECTOR ( 'NONE', #28494, 1000.000000000000227 ) ;
#45847 = DIRECTION ( 'NONE',  ( 0.000000000000000000, -1.000000000000000000, 0.000000000000000000 ) ) ;
#45848 = EDGE_LOOP ( 'NONE', ( #41179, #48117, #8489, #53835 ) ) ;
#45849 = PLANE ( 'NONE',  #7534 ) ;
#45850 = EDGE_CURVE ( 'NONE', #14352, #54876, #42207, .T. ) ;
#45851 = CARTESIAN_POINT ( 'NONE',  ( -18.62310398945015066, 3.686347215771511365, 3.798163987937305919 ) ) ;
#45852 = DIRECTION ( 'NONE',  ( 0.000000000000000000, -0.000000000000000000, -1.000000000000000000 ) ) ;
#45853 = VERTEX_POINT ( 'NONE', #37950 ) ;
#45854 = FACE_OUTER_BOUND ( 'NONE', #16300, .T. ) ;
#45855 = EDGE_CURVE ( 'NONE', #7829, #44519, #26449, .T. ) ;
#45856 = EDGE_LOOP ( 'NONE', ( #7517, #19521, #30858, #1873 ) ) ;
#45857 = EDGE_CURVE ( 'NONE', #33602, #46316, #6730, .T. ) ;
#45858 = AXIS2_PLACEMENT_3D ( 'NONE', #25572, #26410, #12800 ) ;
#45859 = ORIENTED_EDGE ( 'NONE', *, *, #47299, .T. ) ;
#45860 = ORIENTED_EDGE ( 'NONE', *, *, #4511, .T. ) ;
#45861 = ORIENTED_EDGE ( 'NONE', *, *, #16662, .F. ) ;
#45862 = AXIS2_PLACEMENT_3D ( 'NONE', #38935, #12801, #12245 ) ;
#45863 = ORIENTED_EDGE ( 'NONE', *, *, #37393, .T. ) ;
#45864 = CARTESIAN_POINT ( 'NONE',  ( -24.53375310857961367, 18.49370688441070953, 4.545578210335888159 ) ) ;
#45865 = VECTOR ( 'NONE', #34186, 1000.000000000000227 ) ;
#45866 = ORIENTED_EDGE ( 'NONE', *, *, #27070, .T. ) ;
#45867 = EDGE_CURVE ( 'NONE', #9132, #38515, #54410, .T. ) ;
#45868 = EDGE_LOOP ( 'NONE', ( #43759, #39205, #17101, #52310 ) ) ;
#45869 = CARTESIAN_POINT ( 'NONE',  ( 2.072287782118878319, 0.000000000000000000, -2.950529333540147015 ) ) ;
#45870 = ORIENTED_EDGE ( 'NONE', *, *, #8182, .F. ) ;
#45871 = VECTOR ( 'NONE', #48550, 1000.000000000000227 ) ;
#45872 = ORIENTED_EDGE ( 'NONE', *, *, #34447, .T. ) ;
#45873 = ORIENTED_EDGE ( 'NONE', *, *, #22648, .F. ) ;
#45874 = ADVANCED_FACE ( 'NONE', ( #26556 ), #47879, .F. ) ;
#45875 = VECTOR ( 'NONE', #38266, 1000.000000000000114 ) ;
#45876 = AXIS2_PLACEMENT_3D ( 'NONE', #14522, #10259, #5185 ) ;
#45877 = CARTESIAN_POINT ( 'NONE',  ( -14.56888064431065821, -0.1191753592594197858, 12.58947452739191064 ) ) ;
#45878 = DIRECTION ( 'NONE',  ( 1.000000000000000000, 0.000000000000000000, 0.000000000000000000 ) ) ;
#45879 = DIRECTION ( 'NONE',  ( 0.9999697198139515519, 0.000000000000000000, 0.007781995580013368816 ) ) ;
#45880 = CARTESIAN_POINT ( 'NONE',  ( -15.25049964999576524, 0.7721120973665037690, 4.072300582551036996 ) ) ;
#45881 = VECTOR ( 'NONE', #14412, 999.9999999999998863 ) ;
#45882 = LINE ( 'NONE', #50115, #13789 ) ;
#45883 = ORIENTED_EDGE ( 'NONE', *, *, #23891, .F. ) ;
#45884 = AXIS2_PLACEMENT_3D ( 'NONE', #272, #9092, #26401 ) ;
#45885 = ORIENTED_EDGE ( 'NONE', *, *, #7006, .T. ) ;
#45886 = VECTOR ( 'NONE', #15826, 999.9999999999998863 ) ;
#45887 = LINE ( 'NONE', #7001, #24044 ) ;
#45888 = CARTESIAN_POINT ( 'NONE',  ( -26.13415699229845757, -0.1191753592594197858, 6.933020519852192365 ) ) ;
#45889 = AXIS2_PLACEMENT_3D ( 'NONE', #53727, #27334, #1514 ) ;
#45890 = CARTESIAN_POINT ( 'NONE',  ( -28.72987205080237061, 16.07107648356668150, -4.716090232257376336 ) ) ;
#45891 = VECTOR ( 'NONE', #35714, 999.9999999999998863 ) ;
#45892 = FACE_OUTER_BOUND ( 'NONE', #48091, .T. ) ;
#45893 = CARTESIAN_POINT ( 'NONE',  ( 4.854282358214435433, 0.000000000000000000, -1.997863978257567785 ) ) ;
#45894 = PLANE ( 'NONE',  #8672 ) ;
#45895 = ORIENTED_EDGE ( 'NONE', *, *, #19239, .F. ) ;
#45896 = CARTESIAN_POINT ( 'NONE',  ( -30.79567442779373110, 0.000000000000000000, 8.843406890442315316 ) ) ;
#45897 = ORIENTED_EDGE ( 'NONE', *, *, #27978, .F. ) ;
#45898 = CARTESIAN_POINT ( 'NONE',  ( -15.54986472215976967, 0.000000000000000000, 6.376728818173926783 ) ) ;
#45899 = CARTESIAN_POINT ( 'NONE',  ( -22.48440822228507585, -4.565544526780660917, 12.90847583326981507 ) ) ;
#45900 = DIRECTION ( 'NONE',  ( 0.6427681459581294776, -0.7660444431189769032, 0.005002170337467562802 ) ) ;
#45901 = EDGE_CURVE ( 'NONE', #26799, #3531, #52417, .T. ) ;
#45902 = CARTESIAN_POINT ( 'NONE',  ( -13.96101589989143932, 4.172053068839010059, 9.151303665917755126 ) ) ;
#45903 = CARTESIAN_POINT ( 'NONE',  ( -14.50544548941179102, -0.1191753592594190225, 4.438193352997728880 ) ) ;
#45904 = VECTOR ( 'NONE', #12948, 999.9999999999998863 ) ;
#45905 = EDGE_LOOP ( 'NONE', ( #13407, #47895, #14540, #43302 ) ) ;
#45906 = CARTESIAN_POINT ( 'NONE',  ( -57.52614991588065152, -8.291364278369167451, 5.150256511358686722E-15 ) ) ;
#45907 = PLANE ( 'NONE',  #36702 ) ;
#45908 = DIRECTION ( 'NONE',  ( -0.005961354470445682716, -0.6427876096865404731, 0.7660212471507180654 ) ) ;
#45909 = VECTOR ( 'NONE', #46354, 1000.000000000000114 ) ;
#45910 = EDGE_CURVE ( 'NONE', #15181, #24601, #30271, .T. ) ;
#45911 = EDGE_CURVE ( 'NONE', #55181, #54422, #35499, .T. ) ;
#45912 = DIRECTION ( 'NONE',  ( 0.007781995580012663651, 0.000000000000000000, -0.9999697198139515519 ) ) ;
#45913 = AXIS2_PLACEMENT_3D ( 'NONE', #9757, #5757, #48649 ) ;
#45914 = DIRECTION ( 'NONE',  ( 0.007781995580012663651, -3.146120232559066537E-19, -0.9999697198139514409 ) ) ;
#45915 = DIRECTION ( 'NONE',  ( -0.005002170337468016433, -0.7660444431189770143, 0.6427681459581293666 ) ) ;
#45916 = CARTESIAN_POINT ( 'NONE',  ( -27.06552663992790997, 0.000000000000000000, 7.195101427592543786 ) ) ;
#45917 = EDGE_CURVE ( 'NONE', #608, #46062, #4440, .T. ) ;
#45918 = VECTOR ( 'NONE', #24038, 999.9999999999998863 ) ;
#45919 = CARTESIAN_POINT ( 'NONE',  ( -14.40910077049367821, 0.000000000000000000, 4.908278227794890647 ) ) ;
#45920 = CARTESIAN_POINT ( 'NONE',  ( -24.27063949748155380, 0.000000000000000000, 6.308861732390097288 ) ) ;
#45921 = ORIENTED_EDGE ( 'NONE', *, *, #41680, .F. ) ;
#45922 = VECTOR ( 'NONE', #22895, 999.9999999999998863 ) ;
#45923 = ORIENTED_EDGE ( 'NONE', *, *, #44562, .T. ) ;
#45924 = VECTOR ( 'NONE', #20800, 1000.000000000000000 ) ;
#45925 = EDGE_CURVE ( 'NONE', #41663, #26368, #21750, .T. ) ;
#45926 = VECTOR ( 'NONE', #2733, 999.9999999999998863 ) ;
#45927 = ADVANCED_FACE ( 'NONE', ( #8980 ), #29984, .F. ) ;
#45928 = ORIENTED_EDGE ( 'NONE', *, *, #12449, .T. ) ;
#45929 = AXIS2_PLACEMENT_3D ( 'NONE', #5822, #48974, #10908 ) ;
#45930 = ORIENTED_EDGE ( 'NONE', *, *, #37041, .F. ) ;
#45931 = ORIENTED_EDGE ( 'NONE', *, *, #54706, .F. ) ;
#45932 = ADVANCED_FACE ( 'NONE', ( #16942 ), #43593, .T. ) ;
#45933 = EDGE_LOOP ( 'NONE', ( #20651, #24186, #1775, #52008 ) ) ;
#45934 = LINE ( 'NONE', #28609, #55912 ) ;
#45935 = LINE ( 'NONE', #7044, #35652 ) ;
#45936 = LINE ( 'NONE', #42770, #55770 ) ;
#45937 = EDGE_CURVE ( 'NONE', #14383, #36112, #52123, .T. ) ;
#45938 = EDGE_LOOP ( 'NONE', ( #34404, #28781, #36364, #50392 ) ) ;
#45939 = LINE ( 'NONE', #2739, #34035 ) ;
#45940 = ORIENTED_EDGE ( 'NONE', *, *, #1772, .F. ) ;
#45941 = FACE_OUTER_BOUND ( 'NONE', #4732, .T. ) ;
#45942 = ORIENTED_EDGE ( 'NONE', *, *, #5350, .T. ) ;
#45943 = AXIS2_PLACEMENT_3D ( 'NONE', #7741, #55709, #25912 ) ;
#45944 = CARTESIAN_POINT ( 'NONE',  ( -65.92143918783402512, -9.254087391918899286, 0.7134948435226668995 ) ) ;
#45945 = CARTESIAN_POINT ( 'NONE',  ( -13.20213141079607766, 0.000000000000000000, 3.240336806989069451 ) ) ;
#45946 = DIRECTION ( 'NONE',  ( -0.5364919789714478471, 0.6444004775717705469, -0.5449076811759709926 ) ) ;
#45947 = VERTEX_POINT ( 'NONE', #729 ) ;
#45948 = DIRECTION ( 'NONE',  ( 0.007781995580012663651, 0.000000000000000000, -0.9999697198139515519 ) ) ;
#45949 = ORIENTED_EDGE ( 'NONE', *, *, #7231, .F. ) ;
#45950 = LINE ( 'NONE', #42249, #42747 ) ;
#45951 = VECTOR ( 'NONE', #42691, 1000.000000000000227 ) ;
#45952 = FACE_OUTER_BOUND ( 'NONE', #4106, .T. ) ;
#45953 = DIRECTION ( 'NONE',  ( -0.9999697198139514409, -0.000000000000000000, -0.007781995580013368816 ) ) ;
#45954 = FACE_OUTER_BOUND ( 'NONE', #11335, .T. ) ;
#45955 = VECTOR ( 'NONE', #42120, 1000.000000000000227 ) ;
#45956 = DIRECTION ( 'NONE',  ( 1.000000000000000000, 0.000000000000000000, 0.000000000000000000 ) ) ;
#45957 = CARTESIAN_POINT ( 'NONE',  ( -19.71292464457911109, 4.981562823951513508, 4.180163181755506052 ) ) ;
#45958 = CARTESIAN_POINT ( 'NONE',  ( -15.54862763595785147, 3.848249166794009746, 9.236568611826525554 ) ) ;
#45959 = DIRECTION ( 'NONE',  ( -0.5449076811759708816, 0.6444004775717707689, 0.5364919789714475140 ) ) ;
#45960 = CARTESIAN_POINT ( 'NONE',  ( -11.22999478348192959, -0.1191753592594201883, 1.509027109311680270 ) ) ;
#45961 = ORIENTED_EDGE ( 'NONE', *, *, #53591, .F. ) ;
#45962 = DIRECTION ( 'NONE',  ( 1.000000000000000000, 0.000000000000000000, 0.000000000000000000 ) ) ;
#45963 = VERTEX_POINT ( 'NONE', #18049 ) ;
#45964 = EDGE_CURVE ( 'NONE', #43762, #50088, #56115, .T. ) ;
#45965 = VECTOR ( 'NONE', #24931, 1000.000000000000227 ) ;
#45966 = PLANE ( 'NONE',  #12936 ) ;
#45967 = CARTESIAN_POINT ( 'NONE',  ( -26.13337879274045505, 0.000000000000000000, 6.833023547870798353 ) ) ;
#45968 = DIRECTION ( 'NONE',  ( 0.5364919789714477361, 0.6444004775717706579, 0.5449076811759711036 ) ) ;
#45969 = EDGE_CURVE ( 'NONE', #34227, #47810, #17473, .T. ) ;
#45970 = LINE ( 'NONE', #32368, #39567 ) ;
#45971 = FACE_OUTER_BOUND ( 'NONE', #21330, .T. ) ;
#45972 = AXIS2_PLACEMENT_3D ( 'NONE', #6051, #26769, #5210 ) ;
#45973 = DIRECTION ( 'NONE',  ( 0.9999697198139515519, 0.000000000000000000, 0.007781995580013368816 ) ) ;
#45974 = ORIENTED_EDGE ( 'NONE', *, *, #41523, .F. ) ;
#45975 = LINE ( 'NONE', #20399, #41042 ) ;
#45976 = DIRECTION ( 'NONE',  ( 0.000000000000000000, -0.000000000000000000, -1.000000000000000000 ) ) ;
#45977 = CARTESIAN_POINT ( 'NONE',  ( -19.73004039461353543, 0.000000000000000000, 6.144191668299053610 ) ) ;
#45978 = CARTESIAN_POINT ( 'NONE',  ( -12.95637603891941581, 1.905425754524005200, 5.041145850896452174 ) ) ;
#45979 = EDGE_CURVE ( 'NONE', #9978, #940, #47032, .T. ) ;
#45980 = DIRECTION ( 'NONE',  ( -0.005002170337468016433, -0.7660444431189770143, 0.6427681459581293666 ) ) ;
#45981 = EDGE_CURVE ( 'NONE', #682, #4092, #11819, .T. ) ;
#45982 = ADVANCED_FACE ( 'NONE', ( #21177 ), #55832, .F. ) ;
#45983 = LINE ( 'NONE', #38277, #40929 ) ;
#45984 = CARTESIAN_POINT ( 'NONE',  ( -11.80534666676753908, 0.000000000000000000, 2.881874839035335256 ) ) ;
#45985 = EDGE_CURVE ( 'NONE', #41838, #47834, #51572, .T. ) ;
#45986 = FACE_OUTER_BOUND ( 'NONE', #15687, .T. ) ;
#45987 = CARTESIAN_POINT ( 'NONE',  ( -19.98606118697598788, 0.000000000000000000, 5.034203045873751670 ) ) ;
#45988 = ORIENTED_EDGE ( 'NONE', *, *, #25657, .T. ) ;
#45989 = LINE ( 'NONE', #24392, #20341 ) ;
#45990 = VERTEX_POINT ( 'NONE', #8398 ) ;
#45991 = CARTESIAN_POINT ( 'NONE',  ( -19.22961988024793101, -0.1191753592594177458, 14.39986392600063603 ) ) ;
#45992 = LINE ( 'NONE', #7101, #30160 ) ;
#45993 = ORIENTED_EDGE ( 'NONE', *, *, #10139, .F. ) ;
#45994 = VECTOR ( 'NONE', #48073, 1000.000000000000000 ) ;
#45995 = ORIENTED_EDGE ( 'NONE', *, *, #17800, .T. ) ;
#45996 = DIRECTION ( 'NONE',  ( 0.007781995580012663651, 0.000000000000000000, -0.9999697198139515519 ) ) ;
#45997 = ADVANCED_FACE ( 'NONE', ( #25725 ), #22021, .F. ) ;
#45998 = EDGE_CURVE ( 'NONE', #36664, #37392, #8709, .T. ) ;
#45999 = VECTOR ( 'NONE', #40250, 999.9999999999998863 ) ;
#46000 = EDGE_LOOP ( 'NONE', ( #7732, #15530, #29939, #32713 ) ) ;
#46001 = ORIENTED_EDGE ( 'NONE', *, *, #14063, .F. ) ;
#46002 = ORIENTED_EDGE ( 'NONE', *, *, #8154, .T. ) ;
#46003 = EDGE_CURVE ( 'NONE', #29224, #28898, #14076, .T. ) ;
#46004 = LINE ( 'NONE', #45417, #44754 ) ;
#46005 = CARTESIAN_POINT ( 'NONE',  ( -65.30511315870414535, -9.183410695202670837, -2.610734445418878558 ) ) ;
#46006 = CARTESIAN_POINT ( 'NONE',  ( -9.342070512798265725, 0.000000000000000000, 10.59882438848031505 ) ) ;
#46007 = ADVANCED_FACE ( 'NONE', ( #44435 ), #27129, .F. ) ;
#46008 = VECTOR ( 'NONE', #9215, 1000.000000000000227 ) ;
#46009 = VERTEX_POINT ( 'NONE', #31407 ) ;
#46010 = VERTEX_POINT ( 'NONE', #10081 ) ;
#46011 = ADVANCED_FACE ( 'NONE', ( #5284 ), #19146, .F. ) ;
#46012 = CARTESIAN_POINT ( 'NONE',  ( 2.072287782118878319, 0.000000000000000000, -2.950529333540147015 ) ) ;
#46013 = LINE ( 'NONE', #7116, #12765 ) ;
#46014 = EDGE_LOOP ( 'NONE', ( #9245, #39595, #45280, #21202 ) ) ;
#46015 = DIRECTION ( 'NONE',  ( 0.000000000000000000, -0.000000000000000000, -1.000000000000000000 ) ) ;
#46016 = ORIENTED_EDGE ( 'NONE', *, *, #31942, .F. ) ;
#46017 = LINE ( 'NONE', #45714, #37589 ) ;
#46018 = PLANE ( 'NONE',  #21257 ) ;
#46019 = ORIENTED_EDGE ( 'NONE', *, *, #22198, .T. ) ;
#46020 = CARTESIAN_POINT ( 'NONE',  ( 5.283695459130013816, -1.082272386734702607, -2.393428169181708309 ) ) ;
#46021 = DIRECTION ( 'NONE',  ( 0.000000000000000000, -1.000000000000000000, 0.000000000000000000 ) ) ;
#46022 = ORIENTED_EDGE ( 'NONE', *, *, #41605, .T. ) ;
#46023 = DIRECTION ( 'NONE',  ( 0.7660212471507180654, -0.6427876096865404731, 0.005961354470445141482 ) ) ;
#46024 = CARTESIAN_POINT ( 'NONE',  ( -13.96877395608413863, 0.000000000000000000, 8.035687524919993052 ) ) ;
#46025 = VERTEX_POINT ( 'NONE', #9537 ) ;
#46026 = FACE_OUTER_BOUND ( 'NONE', #35494, .T. ) ;
#46027 = CARTESIAN_POINT ( 'NONE',  ( -24.26908309836554878, 0.000000000000000000, 6.108867788427308376 ) ) ;
#46028 = DIRECTION ( 'NONE',  ( -0.5364919789714478471, 0.6444004775717705469, -0.5449076811759709926 ) ) ;
#46029 = PLANE ( 'NONE',  #516 ) ;
#46030 = DIRECTION ( 'NONE',  ( 0.5449076811759707706, 0.6444004775717708799, -0.5364919789714476250 ) ) ;
#46031 = DIRECTION ( 'NONE',  ( -0.6427681459581293666, -0.7660444431189770143, -0.005002170337467561935 ) ) ;
#46032 = VECTOR ( 'NONE', #27976, 999.9999999999998863 ) ;
#46033 = DIRECTION ( 'NONE',  ( 0.007781995580012662783, 0.000000000000000000, -0.9999697198139514409 ) ) ;
#46034 = VERTEX_POINT ( 'NONE', #5540 ) ;
#46035 = LINE ( 'NONE', #7143, #35006 ) ;
#46036 = DIRECTION ( 'NONE',  ( 0.5364919789714477361, 0.6444004775717706579, 0.5449076811759711036 ) ) ;
#46037 = ORIENTED_EDGE ( 'NONE', *, *, #3553, .T. ) ;
#46038 = LINE ( 'NONE', #7146, #20209 ) ;
#46039 = DIRECTION ( 'NONE',  ( 0.005961354470445682716, -0.6427876096865404731, -0.7660212471507180654 ) ) ;
#46040 = EDGE_CURVE ( 'NONE', #17429, #10323, #45285, .T. ) ;
#46041 = VECTOR ( 'NONE', #50638, 999.9999999999998863 ) ;
#46042 = LINE ( 'NONE', #16215, #17715 ) ;
#46043 = ADVANCED_FACE ( 'NONE', ( #22858 ), #35647, .F. ) ;
#46044 = DIRECTION ( 'NONE',  ( 0.5364919789714477361, 0.6444004775717706579, 0.5449076811759711036 ) ) ;
#46045 = CARTESIAN_POINT ( 'NONE',  ( -13.73672976910459909, 0.000000000000000000, 12.22661844811216270 ) ) ;
#46046 = VERTEX_POINT ( 'NONE', #40755 ) ;
#46047 = EDGE_LOOP ( 'NONE', ( #19460, #17080, #40466, #42997 ) ) ;
#46048 = DIRECTION ( 'NONE',  ( 0.005002170337468016433, -0.7660444431189770143, -0.6427681459581293666 ) ) ;
#46049 = DIRECTION ( 'NONE',  ( -0.7660212471507179544, -0.6427876096865405842, -0.005961354470445141482 ) ) ;
#46050 = LINE ( 'NONE', #14625, #55600 ) ;
#46051 = ORIENTED_EDGE ( 'NONE', *, *, #8032, .T. ) ;
#46052 = DIRECTION ( 'NONE',  ( 0.6427681459581294776, -0.7660444431189769032, 0.005002170337467562802 ) ) ;
#46053 = ORIENTED_EDGE ( 'NONE', *, *, #42472, .T. ) ;
#46054 = CARTESIAN_POINT ( 'NONE',  ( -19.22961988024793101, -0.1191753592594177458, 14.39986392600063603 ) ) ;
#46055 = ORIENTED_EDGE ( 'NONE', *, *, #54915, .F. ) ;
#46056 = VERTEX_POINT ( 'NONE', #44178 ) ;
#46057 = PLANE ( 'NONE',  #30250 ) ;
#46058 = DIRECTION ( 'NONE',  ( 0.000000000000000000, -1.000000000000000000, 0.000000000000000000 ) ) ;
#46059 = CARTESIAN_POINT ( 'NONE',  ( 2.072287782118878319, 0.000000000000000000, -2.950529333540147015 ) ) ;
#46060 = EDGE_LOOP ( 'NONE', ( #41367, #20972, #14830, #47396 ) ) ;
#46061 = LINE ( 'NONE', #7171, #22025 ) ;
#46062 = VERTEX_POINT ( 'NONE', #36474 ) ;
#46063 = EDGE_CURVE ( 'NONE', #47902, #11899, #18611, .T. ) ;
#46064 = ORIENTED_EDGE ( 'NONE', *, *, #55907, .F. ) ;
#46065 = ORIENTED_EDGE ( 'NONE', *, *, #27782, .F. ) ;
#46066 = LINE ( 'NONE', #10868, #31340 ) ;
#46067 = EDGE_CURVE ( 'NONE', #51780, #32296, #2098, .T. ) ;
#46068 = LINE ( 'NONE', #53297, #32185 ) ;
#46069 = ORIENTED_EDGE ( 'NONE', *, *, #52923, .T. ) ;
#46070 = DIRECTION ( 'NONE',  ( -0.005961354470445682716, -0.6427876096865404731, 0.7660212471507180654 ) ) ;
#46071 = EDGE_LOOP ( 'NONE', ( #8463, #34428, #10646, #34655, #41995 ) ) ;
#46072 = DIRECTION ( 'NONE',  ( 0.007781995580012663651, -3.146120232559066537E-19, -0.9999697198139514409 ) ) ;
#46073 = LINE ( 'NONE', #7181, #34051 ) ;
#46074 = VECTOR ( 'NONE', #2834, 1000.000000000000114 ) ;
#46075 = ORIENTED_EDGE ( 'NONE', *, *, #21812, .F. ) ;
#46076 = EDGE_CURVE ( 'NONE', #49857, #14113, #14907, .T. ) ;
#46077 = FACE_OUTER_BOUND ( 'NONE', #31316, .T. ) ;
#46078 = VERTEX_POINT ( 'NONE', #14366 ) ;
#46079 = LINE ( 'NONE', #32725, #44589 ) ;
#46080 = CARTESIAN_POINT ( 'NONE',  ( -16.79925329029790149, 0.000000000000000000, 13.49544742625427496 ) ) ;
#46081 = FACE_OUTER_BOUND ( 'NONE', #44835, .T. ) ;
#46082 = LINE ( 'NONE', #41802, #7568 ) ;
#46083 = DIRECTION ( 'NONE',  ( -0.9999697198139514409, -0.000000000000000000, -0.007781995580013368816 ) ) ;
#46084 = DIRECTION ( 'NONE',  ( 0.007781995580012663651, -3.146120232559066537E-19, -0.9999697198139514409 ) ) ;
#46085 = EDGE_LOOP ( 'NONE', ( #26812, #11877, #16379, #20771 ) ) ;
#46086 = ORIENTED_EDGE ( 'NONE', *, *, #51919, .T. ) ;
#46087 = DIRECTION ( 'NONE',  ( 0.000000000000000000, -0.000000000000000000, -1.000000000000000000 ) ) ;
#46088 = CARTESIAN_POINT ( 'NONE',  ( -19.12407506631472032, 5.305366725996512045, 13.01677197203713554 ) ) ;
#46089 = DIRECTION ( 'NONE',  ( 0.5449076811759707706, 0.6444004775717708799, -0.5364919789714476250 ) ) ;
#46090 = DIRECTION ( 'NONE',  ( -0.5449076811759708816, 0.6444004775717707689, 0.5364919789714475140 ) ) ;
#46091 = PLANE ( 'NONE',  #52416 ) ;
#46092 = PLANE ( 'NONE',  #53054 ) ;
#46093 = VERTEX_POINT ( 'NONE', #31677 ) ;
#46094 = DIRECTION ( 'NONE',  ( -0.005002170337468016433, -0.7660444431189770143, 0.6427681459581293666 ) ) ;
#46095 = CARTESIAN_POINT ( 'NONE',  ( -13.94290747453659485, 0.000000000000000000, 4.711900195600111196 ) ) ;
#46096 = VERTEX_POINT ( 'NONE', #48982 ) ;
#46097 = LINE ( 'NONE', #46356, #50164 ) ;
#46098 = ADVANCED_FACE ( 'NONE', ( #52669 ), #18309, .F. ) ;
#46099 = CARTESIAN_POINT ( 'NONE',  ( -19.87054375134978557, -1.588720260541462981, 6.487297621897504030 ) ) ;
#46100 = EDGE_LOOP ( 'NONE', ( #35078, #23768, #44021, #35690 ) ) ;
#46101 = EDGE_CURVE ( 'NONE', #7825, #18, #4407, .T. ) ;
#46102 = CARTESIAN_POINT ( 'NONE',  ( -68.84530413953069683, 2.000000000000001776, -6.094799798532269719 ) ) ;
#46103 = DIRECTION ( 'NONE',  ( -0.5364919789714478471, 0.6444004775717705469, -0.5449076811759709926 ) ) ;
#46104 = CARTESIAN_POINT ( 'NONE',  ( -9.503836956215090837, 0.000000000000000000, 5.685116264642521955 ) ) ;
#46105 = EDGE_CURVE ( 'NONE', #547, #30844, #23689, .T. ) ;
#46106 = EDGE_CURVE ( 'NONE', #50616, #4253, #13773, .T. ) ;
#46107 = DIRECTION ( 'NONE',  ( 0.000000000000000000, -1.000000000000000000, 0.000000000000000000 ) ) ;
#46108 = LINE ( 'NONE', #50068, #39214 ) ;
#46109 = EDGE_LOOP ( 'NONE', ( #10262, #13719, #50654, #50178 ) ) ;
#46110 = ORIENTED_EDGE ( 'NONE', *, *, #28232, .F. ) ;
#46111 = CARTESIAN_POINT ( 'NONE',  ( -16.23115121177390208, -4.403642575758163424, 3.045552206283119734 ) ) ;
#46112 = DIRECTION ( 'NONE',  ( -0.005961354470445682716, -0.6427876096865404731, 0.7660212471507180654 ) ) ;
#46113 = CARTESIAN_POINT ( 'NONE',  ( -19.67789331192963331, -0.1191753592594191058, 6.983264656678034754 ) ) ;
#46114 = DIRECTION ( 'NONE',  ( -0.005961354470445682716, -0.6427876096865404731, 0.7660212471507180654 ) ) ;
#46115 = VECTOR ( 'NONE', #17968, 1000.000000000000227 ) ;
#46116 = CARTESIAN_POINT ( 'NONE',  ( -16.94796712057759080, 0.000000000000000000, 6.904506545422637309 ) ) ;
#46117 = DIRECTION ( 'NONE',  ( -1.000000000000000000, 0.000000000000000000, 0.000000000000000000 ) ) ;
#46118 = EDGE_LOOP ( 'NONE', ( #40569, #37139, #6317 ) ) ;
#46119 = LINE ( 'NONE', #7223, #45582 ) ;
#46120 = EDGE_CURVE ( 'NONE', #40102, #1292, #10371, .T. ) ;
#46121 = DIRECTION ( 'NONE',  ( 0.9999697198139515519, 0.000000000000000000, 0.007781995580013368816 ) ) ;
#46122 = DIRECTION ( 'NONE',  ( 0.007781995580012662783, 0.000000000000000000, -0.9999697198139514409 ) ) ;
#46123 = ORIENTED_EDGE ( 'NONE', *, *, #49439, .F. ) ;
#46124 = DIRECTION ( 'NONE',  ( 0.5449076811759707706, 0.6444004775717708799, -0.5364919789714476250 ) ) ;
#46125 = CARTESIAN_POINT ( 'NONE',  ( -12.70458494993575194, -0.1191753592594197858, 11.86531876794841978 ) ) ;
#46126 = CARTESIAN_POINT ( 'NONE',  ( -14.39249272523662704, 5.305366725996514710, 2.103195701879582824 ) ) ;
#46127 = ORIENTED_EDGE ( 'NONE', *, *, #46284, .T. ) ;
#46128 = LINE ( 'NONE', #45557, #47673 ) ;
#46129 = ORIENTED_EDGE ( 'NONE', *, *, #45277, .T. ) ;
#46130 = ORIENTED_EDGE ( 'NONE', *, *, #31232, .F. ) ;
#46131 = EDGE_LOOP ( 'NONE', ( #47812, #39085, #2625, #33105 ) ) ;
#46132 = ORIENTED_EDGE ( 'NONE', *, *, #475, .F. ) ;
#46133 = ORIENTED_EDGE ( 'NONE', *, *, #172, .F. ) ;
#46134 = CARTESIAN_POINT ( 'NONE',  ( -10.84028925556084388, -0.1191753592594197858, 11.14116300850493246 ) ) ;
#46135 = ORIENTED_EDGE ( 'NONE', *, *, #16828, .F. ) ;
#46136 = ORIENTED_EDGE ( 'NONE', *, *, #35590, .F. ) ;
#46137 = CARTESIAN_POINT ( 'NONE',  ( -18.58508473505288805, 0.000000000000000000, 4.137115615367276789 ) ) ;
#46138 = EDGE_CURVE ( 'NONE', #7759, #20365, #6133, .T. ) ;
#46139 = ORIENTED_EDGE ( 'NONE', *, *, #29580, .F. ) ;
#46140 = ORIENTED_EDGE ( 'NONE', *, *, #38678, .T. ) ;
#46141 = DIRECTION ( 'NONE',  ( 0.9999697198139515519, 0.000000000000000000, 0.007781995580013368816 ) ) ;
#46142 = DIRECTION ( 'NONE',  ( 0.000000000000000000, 0.000000000000000000, 1.000000000000000000 ) ) ;
#46143 = FACE_OUTER_BOUND ( 'NONE', #50255, .T. ) ;
#46144 = CARTESIAN_POINT ( 'NONE',  ( -13.01908042430739698, -0.03228989815065527735, 1.937343867007571330 ) ) ;
#46145 = DIRECTION ( 'NONE',  ( -0.6246952433987893460, -0.7422098413412802076, 0.2426528472758542054 ) ) ;
#46146 = VERTEX_POINT ( 'NONE', #37600 ) ;
#46147 = EDGE_CURVE ( 'NONE', #9627, #12842, #41836, .T. ) ;
#46148 = PRESENTATION_LAYER_ASSIGNMENT (  '', '', ( #56136 ) ) ;
#46149 = ORIENTED_EDGE ( 'NONE', *, *, #44572, .T. ) ;
#46150 = CARTESIAN_POINT ( 'NONE',  ( -19.28279667285536902, 3.362543313726509719, 4.064742069204503316 ) ) ;
#46151 = CARTESIAN_POINT ( 'NONE',  ( -15.07373161129755346, 0.000000000000000000, 4.903105916910880602 ) ) ;
#46152 = EDGE_CURVE ( 'NONE', #5277, #25140, #16032, .T. ) ;
#46153 = EDGE_CURVE ( 'NONE', #42919, #2132, #2662, .T. ) ;
#46154 = CARTESIAN_POINT ( 'NONE',  ( -37.92083312653435456, 10.76467263238142635, -4.937384707706697462 ) ) ;
#46155 = DIRECTION ( 'NONE',  ( -0.9999697198139514409, -0.000000000000000000, -0.007781995580013368816 ) ) ;
#46156 = FACE_OUTER_BOUND ( 'NONE', #17796, .T. ) ;
#46157 = PLANE ( 'NONE',  #20444 ) ;
#46158 = VERTEX_POINT ( 'NONE', #19726 ) ;
#46159 = CARTESIAN_POINT ( 'NONE',  ( -27.06708303904391144, 0.000000000000000000, 7.395095371555332697 ) ) ;
#46160 = ADVANCED_FACE ( 'NONE', ( #24816 ), #3520, .F. ) ;
#46161 = VERTEX_POINT ( 'NONE', #46116 ) ;
#46162 = PLANE ( 'NONE',  #7496 ) ;
#46163 = CARTESIAN_POINT ( 'NONE',  ( -14.79106777481693058, 5.143464774974011888, 11.06797610652191644 ) ) ;
#46164 = EDGE_CURVE ( 'NONE', #6174, #38693, #54614, .T. ) ;
#46165 = FACE_OUTER_BOUND ( 'NONE', #47874, .T. ) ;
#46166 = LINE ( 'NONE', #32303, #34055 ) ;
#46167 = EDGE_CURVE ( 'NONE', #3767, #9065, #7220, .T. ) ;
#46168 = CARTESIAN_POINT ( 'NONE',  ( -11.87243407472968926, 0.000000000000000000, 11.50246268866867361 ) ) ;
#46169 = ORIENTED_EDGE ( 'NONE', *, *, #4480, .T. ) ;
#46170 = ORIENTED_EDGE ( 'NONE', *, *, #24588, .F. ) ;
#46171 = LINE ( 'NONE', #2714, #14843 ) ;
#46172 = PLANE ( 'NONE',  #16797 ) ;
#46173 = LINE ( 'NONE', #7277, #38797 ) ;
#46174 = EDGE_CURVE ( 'NONE', #44242, #53889, #48255, .T. ) ;
#46175 = LINE ( 'NONE', #42491, #21019 ) ;
#46176 = FACE_OUTER_BOUND ( 'NONE', #3160, .T. ) ;
#46177 = CARTESIAN_POINT ( 'NONE',  ( -22.40556560354864146, -0.1191753592594197858, 5.484709000965211523 ) ) ;
#46178 = DIRECTION ( 'NONE',  ( -0.9321478471874540261, 0.000000000000000000, 0.3620778797217457656 ) ) ;
#46179 = EDGE_CURVE ( 'NONE', #23956, #40778, #10915, .T. ) ;
#46180 = CARTESIAN_POINT ( 'NONE',  ( -66.26160924740132430, -9.293096122682349858, -3.456045872278597830 ) ) ;
#46181 = CARTESIAN_POINT ( 'NONE',  ( -21.99342978027240392, 19.77817019059910564, 4.416855414988919648 ) ) ;
#46182 = STYLED_ITEM ( 'NONE', ( #49924 ), #26591 ) ;
#46183 = ORIENTED_EDGE ( 'NONE', *, *, #50713, .F. ) ;
#46184 = ORIENTED_EDGE ( 'NONE', *, *, #31474, .F. ) ;
#46185 = EDGE_LOOP ( 'NONE', ( #17425, #22410, #55269, #46972 ) ) ;
#46186 = ORIENTED_EDGE ( 'NONE', *, *, #31442, .T. ) ;
#46187 = VERTEX_POINT ( 'NONE', #19983 ) ;
#46188 = CARTESIAN_POINT ( 'NONE',  ( -13.03243440100211892, 0.000000000000000000, 7.134984182645506046 ) ) ;
#46189 = DIRECTION ( 'NONE',  ( 0.005961354470445682716, -0.6427876096865404731, -0.7660212471507180654 ) ) ;
#46190 = CARTESIAN_POINT ( 'NONE',  ( -10.74029228357944987, 0.000000000000000000, 11.14194120806293320 ) ) ;
#46191 = ORIENTED_EDGE ( 'NONE', *, *, #35865, .T. ) ;
#46192 = CARTESIAN_POINT ( 'NONE',  ( 5.558065546916891364, 8.867787166497208620E-06, 2.260478567416572826 ) ) ;
#46193 = EDGE_CURVE ( 'NONE', #9089, #41560, #37304, .T. ) ;
#46194 = EDGE_LOOP ( 'NONE', ( #8300, #54630, #28149, #8578 ) ) ;
#46195 = CARTESIAN_POINT ( 'NONE',  ( -15.96710241509184058, -0.1191753592594218814, 13.13259134697452879 ) ) ;
#46196 = EDGE_LOOP ( 'NONE', ( #28048, #23159, #15074, #29799 ) ) ;
#46197 = CARTESIAN_POINT ( 'NONE',  ( -68.43013375671482379, -9.541769944318687635, 7.657917462034228073 ) ) ;
#46198 = CARTESIAN_POINT ( 'NONE',  ( 2.072287782118878319, 0.000000000000000000, -2.950529333540147015 ) ) ;
#46199 = DIRECTION ( 'NONE',  ( 0.007781995580012663651, 0.000000000000000000, -0.9999697198139515519 ) ) ;
#46200 = VERTEX_POINT ( 'NONE', #42133 ) ;
#46201 = CARTESIAN_POINT ( 'NONE',  ( -22.40634380310664397, 0.000000000000000000, 5.584705972946605534 ) ) ;
#46202 = ORIENTED_EDGE ( 'NONE', *, *, #39999, .F. ) ;
#46203 = CARTESIAN_POINT ( 'NONE',  ( -32.65841372305263235, 0.000000000000000000, 9.367568705923016381 ) ) ;
#46204 = CARTESIAN_POINT ( 'NONE',  ( -14.56888064431065821, -0.1191753592594197858, 12.58947452739191064 ) ) ;
#46205 = EDGE_CURVE ( 'NONE', #29912, #25311, #52799, .T. ) ;
#46206 = LINE ( 'NONE', #41671, #31479 ) ;
#46207 = DIRECTION ( 'NONE',  ( -0.005002170337468016433, -0.7660444431189770143, 0.6427681459581293666 ) ) ;
#46208 = CARTESIAN_POINT ( 'NONE',  ( -61.21055533376208047, 7.871010810323351592, 2.999999999999993339 ) ) ;
#46209 = DIRECTION ( 'NONE',  ( -0.7660212471507179544, -0.6427876096865405842, -0.005961354470445141482 ) ) ;
#46210 = CARTESIAN_POINT ( 'NONE',  ( -14.66887761629205222, 0.000000000000000000, 12.58869632783390990 ) ) ;
#46211 = CARTESIAN_POINT ( 'NONE',  ( -15.88130887279446490, 0.000000000000000000, 3.050160814894388839 ) ) ;
#46212 = VERTEX_POINT ( 'NONE', #33062 ) ;
#46213 = PLANE ( 'NONE',  #51944 ) ;
#46214 = ORIENTED_EDGE ( 'NONE', *, *, #1623, .T. ) ;
#46215 = CARTESIAN_POINT ( 'NONE',  ( 2.072287782118878319, 0.000000000000000000, -2.950529333540147015 ) ) ;
#46216 = CARTESIAN_POINT ( 'NONE',  ( -11.36657625147399386, 0.000000000000000000, 6.209278080123224797 ) ) ;
#46217 = ADVANCED_FACE ( 'NONE', ( #55198 ), #54926, .F. ) ;
#46218 = DIRECTION ( 'NONE',  ( 0.5364919789714477361, 0.6444004775717706579, 0.5449076811759711036 ) ) ;
#46219 = CARTESIAN_POINT ( 'NONE',  ( -14.20280369269832832, 0.000000000000000000, 12.40765738797303719 ) ) ;
#46220 = DIRECTION ( 'NONE',  ( 0.005961354470445682716, -0.6427876096865404731, -0.7660212471507180654 ) ) ;
#46221 = EDGE_CURVE ( 'NONE', #1131, #45245, #33355, .T. ) ;
#46222 = ADVANCED_FACE ( 'NONE', ( #33607 ), #41579, .F. ) ;
#46223 = CARTESIAN_POINT ( 'NONE',  ( -13.78642791384490529, 2.876837460659008805, 6.957818291500617924 ) ) ;
#46224 = DIRECTION ( 'NONE',  ( 0.000000000000000000, 1.000000000000000000, 0.000000000000000000 ) ) ;
#46225 = ORIENTED_EDGE ( 'NONE', *, *, #30109, .T. ) ;
#46226 = FACE_OUTER_BOUND ( 'NONE', #47281, .T. ) ;
#46227 = DIRECTION ( 'NONE',  ( 0.007781995580012663651, 0.000000000000000000, -0.9999697198139515519 ) ) ;
#46228 = CARTESIAN_POINT ( 'NONE',  ( -14.94760462649100496, 0.000000000000000000, 2.488088991209854051 ) ) ;
#46229 = DIRECTION ( 'NONE',  ( 0.5364919789714477361, 0.6444004775717706579, 0.5449076811759711036 ) ) ;
#46230 = DIRECTION ( 'NONE',  ( 0.5449076811759707706, 0.6444004775717708799, -0.5364919789714476250 ) ) ;
#46231 = ADVANCED_FACE ( 'NONE', ( #50917 ), #32767, .F. ) ;
#46232 = LINE ( 'NONE', #19850, #30953 ) ;
#46233 = DIRECTION ( 'NONE',  ( -0.005002170337468016433, -0.7660444431189770143, 0.6427681459581293666 ) ) ;
#46234 = DIRECTION ( 'NONE',  ( -0.6427681459581293666, -0.7660444431189770143, -0.005002170337467561935 ) ) ;
#46235 = CARTESIAN_POINT ( 'NONE',  ( -18.73437280588166942, -1.813211359398155809, 6.934787098642066994 ) ) ;
#46236 = ORIENTED_EDGE ( 'NONE', *, *, #26125, .F. ) ;
#46237 = EDGE_CURVE ( 'NONE', #24506, #4739, #7797, .T. ) ;
#46238 = CARTESIAN_POINT ( 'NONE',  ( -7.673472522921562344, 7.485187178597575652, 6.199010895790313391 ) ) ;
#46239 = CARTESIAN_POINT ( 'NONE',  ( -11.40636015113596180, 0.000000000000000000, 11.32142374880780089 ) ) ;
#46240 = ORIENTED_EDGE ( 'NONE', *, *, #53584, .T. ) ;
#46241 = PLANE ( 'NONE',  #50404 ) ;
#46242 = CARTESIAN_POINT ( 'NONE',  ( -14.00280974873554030, 0.000000000000000000, 12.40921378708904044 ) ) ;
#46243 = ORIENTED_EDGE ( 'NONE', *, *, #13677, .F. ) ;
#46244 = EDGE_LOOP ( 'NONE', ( #18820, #39392, #33501, #45321 ) ) ;
#46245 = LINE ( 'NONE', #47890, #47408 ) ;
#46246 = AXIS2_PLACEMENT_3D ( 'NONE', #48183, #8456, #26331 ) ;
#46247 = ORIENTED_EDGE ( 'NONE', *, *, #47268, .T. ) ;
#46248 = EDGE_LOOP ( 'NONE', ( #128, #24726, #2964, #44199 ) ) ;
#46249 = ORIENTED_EDGE ( 'NONE', *, *, #51458, .T. ) ;
#46250 = LINE ( 'NONE', #11352, #25700 ) ;
#46251 = CARTESIAN_POINT ( 'NONE',  ( -66.91922558340073124, -9.368507752467420957, 6.901237005686191139 ) ) ;
#46252 = PLANE ( 'NONE',  #35797 ) ;
#46253 = EDGE_CURVE ( 'NONE', #30294, #45499, #49819, .T. ) ;
#46254 = ORIENTED_EDGE ( 'NONE', *, *, #10544, .T. ) ;
#46256 = ORIENTED_EDGE ( 'NONE', *, *, #37977, .T. ) ;
#46255 = EDGE_CURVE ( 'NONE', #52840, #38691, #45838, .T. ) ;
#46257 = DIRECTION ( 'NONE',  ( -0.005002170337468016433, -0.7660444431189770143, 0.6427681459581293666 ) ) ;
#46258 = DIRECTION ( 'NONE',  ( -0.005002170337468016433, -0.7660444431189770143, 0.6427681459581293666 ) ) ;
#46260 = EDGE_CURVE ( 'NONE', #5087, #30222, #25962, .T. ) ;
#46259 = ORIENTED_EDGE ( 'NONE', *, *, #3579, .F. ) ;
#46261 = DIRECTION ( 'NONE',  ( 0.007781995580012663651, -3.146120232559066537E-19, -0.9999697198139514409 ) ) ;
#46262 = ORIENTED_EDGE ( 'NONE', *, *, #2039, .F. ) ;
#46263 = PLANE ( 'NONE',  #9460 ) ;
#46264 = DIRECTION ( 'NONE',  ( -0.5449076811759708816, 0.6444004775717707689, 0.5364919789714475140 ) ) ;
#46265 = EDGE_CURVE ( 'NONE', #2953, #46599, #30201, .T. ) ;
#46266 = EDGE_CURVE ( 'NONE', #12870, #45853, #12875, .T. ) ;
#46267 = ADVANCED_FACE ( 'NONE', ( #3783 ), #12609, .F. ) ;
#46268 = EDGE_LOOP ( 'NONE', ( #24682, #5322, #51638, #52865 ) ) ;
#46269 = CARTESIAN_POINT ( 'NONE',  ( -27.06552663992790997, 0.000000000000000000, 7.195101427592543786 ) ) ;
#46270 = DIRECTION ( 'NONE',  ( 0.5449076811759707706, 0.6444004775717708799, -0.5364919789714476250 ) ) ;
#46271 = ORIENTED_EDGE ( 'NONE', *, *, #20775, .F. ) ;
#46272 = CARTESIAN_POINT ( 'NONE',  ( -14.93495759592298988, 0.000000000000000000, 12.77129166681078409 ) ) ;
#46273 =( LENGTH_UNIT ( ) NAMED_UNIT ( * ) SI_UNIT ( .MILLI., .METRE. ) );
#46274 = DIRECTION ( 'NONE',  ( 0.007781995580012662783, 0.000000000000000000, -0.9999697198139514409 ) ) ;
#46275 = ORIENTED_EDGE ( 'NONE', *, *, #40521, .T. ) ;
#46276 = CARTESIAN_POINT ( 'NONE',  ( -18.34630826372213264, 0.000000000000000000, 7.462962457339162192 ) ) ;
#46277 = DIRECTION ( 'NONE',  ( -0.5449076811759708816, 0.6444004775717707689, 0.5364919789714475140 ) ) ;
#46278 = DIRECTION ( 'NONE',  ( -0.005002170337468016433, -0.7660444431189770143, 0.6427681459581293666 ) ) ;
#46279 = EDGE_CURVE ( 'NONE', #18658, #19197, #17145, .T. ) ;
#46280 = LINE ( 'NONE', #28721, #44044 ) ;
#46281 = LINE ( 'NONE', #54268, #9535 ) ;
#46282 = LINE ( 'NONE', #30104, #46074 ) ;
#46283 = VECTOR ( 'NONE', #28426, 1000.000000000000227 ) ;
#46284 = EDGE_CURVE ( 'NONE', #28225, #11772, #46970, .T. ) ;
#46285 = LINE ( 'NONE', #29257, #45781 ) ;
#46286 = ORIENTED_EDGE ( 'NONE', *, *, #48937, .T. ) ;
#46287 = DIRECTION ( 'NONE',  ( 0.7660212471507180654, -0.6427876096865404731, 0.005961354470445141482 ) ) ;
#46288 = CARTESIAN_POINT ( 'NONE',  ( -11.81684288078866807, 0.000000000000000000, 4.359113652066392675 ) ) ;
#46289 = EDGE_CURVE ( 'NONE', #11344, #9180, #4083, .T. ) ;
#46290 = LINE ( 'NONE', #51684, #32345 ) ;
#46291 = ORIENTED_EDGE ( 'NONE', *, *, #39364, .F. ) ;
#46292 = PLANE ( 'NONE',  #41981 ) ;
#46293 = DIRECTION ( 'NONE',  ( 0.000000000000000000, -1.000000000000000000, 0.000000000000000000 ) ) ;
#46294 = EDGE_CURVE ( 'NONE', #37913, #43375, #25652, .T. ) ;
#46295 = DIRECTION ( 'NONE',  ( -0.2426528472758542054, 0.7422098413412800966, -0.6246952433987894571 ) ) ;
#46296 = CARTESIAN_POINT ( 'NONE',  ( -18.19747506107908563, 0.000000000000000000, 14.03856424583689311 ) ) ;
#46297 = EDGE_CURVE ( 'NONE', #16744, #46741, #47223, .T. ) ;
#46298 = CYLINDRICAL_SURFACE ( 'NONE', #18382, 2.749999999999999112 ) ;
#46299 = ORIENTED_EDGE ( 'NONE', *, *, #46592, .F. ) ;
#46300 = ORIENTED_EDGE ( 'NONE', *, *, #14827, .F. ) ;
#46301 = PLANE ( 'NONE',  #24986 ) ;
#46302 = PLANE ( 'NONE',  #6677 ) ;
#46303 = AXIS2_PLACEMENT_3D ( 'NONE', #1890, #20047, #53862 ) ;
#46304 = ORIENTED_EDGE ( 'NONE', *, *, #36191, .F. ) ;
#46305 = LINE ( 'NONE', #46598, #53065 ) ;
#46306 = ORIENTED_EDGE ( 'NONE', *, *, #18343, .T. ) ;
#46307 = DIRECTION ( 'NONE',  ( 0.5449076811759707706, 0.6444004775717708799, -0.5364919789714476250 ) ) ;
#46308 = ORIENTED_EDGE ( 'NONE', *, *, #13164, .F. ) ;
#46309 = EDGE_LOOP ( 'NONE', ( #10547, #45897, #43246, #20371 ) ) ;
#46310 = ORIENTED_EDGE ( 'NONE', *, *, #14509, .F. ) ;
#46311 = CARTESIAN_POINT ( 'NONE',  ( -10.86900711168552291, 0.000000000000000000, 1.981171496760848916 ) ) ;
#46312 = LINE ( 'NONE', #50861, #3289 ) ;
#46313 = CARTESIAN_POINT ( 'NONE',  ( -9.442067484779661513, -0.1191753592594197858, 10.59804618892231254 ) ) ;
#46315 = LINE ( 'NONE', #11128, #39246 ) ;
#46314 = AXIS2_PLACEMENT_3D ( 'NONE', #5183, #6288, #53424 ) ;
#46316 = VERTEX_POINT ( 'NONE', #42682 ) ;
#46317 = AXIS2_PLACEMENT_3D ( 'NONE', #41967, #12473, #55066 ) ;
#46318 = ORIENTED_EDGE ( 'NONE', *, *, #34890, .T. ) ;
#46319 = ORIENTED_EDGE ( 'NONE', *, *, #49474, .F. ) ;
#46320 = CARTESIAN_POINT ( 'NONE',  ( -14.39185644946198295, 0.000000000000000000, 2.692420008248304963 ) ) ;
#46321 = CARTESIAN_POINT ( 'NONE',  ( -21.47419595591918906, 0.000000000000000000, 5.222628093224860102 ) ) ;
#46322 = ORIENTED_EDGE ( 'NONE', *, *, #18702, .T. ) ;
#46323 = DIRECTION ( 'NONE',  ( 0.5364919789714477361, 0.6444004775717706579, 0.5449076811759711036 ) ) ;
#46324 = VERTEX_POINT ( 'NONE', #34457 ) ;
#46325 = DIRECTION ( 'NONE',  ( -0.6427681459581293666, -0.7660444431189770143, -0.005002170337467561935 ) ) ;
#46326 = FACE_OUTER_BOUND ( 'NONE', #30794, .T. ) ;
#46327 = EDGE_CURVE ( 'NONE', #42852, #42669, #4633, .T. ) ;
#46328 = EDGE_CURVE ( 'NONE', #33489, #23596, #55464, .T. ) ;
#46329 = ORIENTED_EDGE ( 'NONE', *, *, #6967, .F. ) ;
#46330 = DIRECTION ( 'NONE',  ( -0.9932609354084158682, -0.1139014070068027351, 0.02142857142857155367 ) ) ;
#46331 = VERTEX_POINT ( 'NONE', #21106 ) ;
#46332 = EDGE_CURVE ( 'NONE', #3951, #11444, #69, .T. ) ;
#46333 = CARTESIAN_POINT ( 'NONE',  ( -20.54049170961573267, 0.000000000000000000, 4.660556269540326646 ) ) ;
#46334 = CARTESIAN_POINT ( 'NONE',  ( -19.60834386242827776, 0.000000000000000000, 4.298478389818581213 ) ) ;
#46335 = FACE_OUTER_BOUND ( 'NONE', #8258, .T. ) ;
#46336 = CARTESIAN_POINT ( 'NONE',  ( -13.14148572275694171, -1.813211359398156919, 4.762319820311594398 ) ) ;
#46337 = PLANE ( 'NONE',  #46861 ) ;
#46338 = FACE_OUTER_BOUND ( 'NONE', #50788, .T. ) ;
#46339 = APPLICATION_CONTEXT ( 'automotive_design' ) ;
#46340 = ORIENTED_EDGE ( 'NONE', *, *, #28270, .T. ) ;
#46341 = AXIS2_PLACEMENT_3D ( 'NONE', #20405, #25503, #24386 ) ;
#46342 = B_SPLINE_CURVE_WITH_KNOTS ( 'NONE', 3,
 ( #9665, #31526, #22984, #5959 ),
 .UNSPECIFIED., .F., .F.,
 ( 4, 4 ),
 ( 0.000000000000000000, 0.0003538274413750522557 ),
 .UNSPECIFIED. ) ;
#46343 = ORIENTED_EDGE ( 'NONE', *, *, #47064, .F. ) ;
#46344 = VECTOR ( 'NONE', #12988, 999.9999999999998863 ) ;
#46345 = LINE ( 'NONE', #7459, #39151 ) ;
#46346 = DIRECTION ( 'NONE',  ( 0.005002170337468016433, -0.7660444431189770143, -0.6427681459581293666 ) ) ;
#46347 = CARTESIAN_POINT ( 'NONE',  ( -67.39308507045382157, 0.1330233015420136389, 1.352000712394435311 ) ) ;
#46348 = DIRECTION ( 'NONE',  ( -0.5449076811759708816, 0.6444004775717707689, 0.5364919789714475140 ) ) ;
#46349 = FACE_OUTER_BOUND ( 'NONE', #37700, .T. ) ;
#46350 = DIRECTION ( 'NONE',  ( 0.007781995580012663651, 0.000000000000000000, -0.9999697198139515519 ) ) ;
#46351 = ORIENTED_EDGE ( 'NONE', *, *, #46040, .T. ) ;
#46352 = CARTESIAN_POINT ( 'NONE',  ( -10.74029228357944987, 0.000000000000000000, 11.14194120806293320 ) ) ;
#46353 = ADVANCED_FACE ( 'NONE', ( #34734 ), #30773, .F. ) ;
#46354 = DIRECTION ( 'NONE',  ( 0.5449076811759707706, 0.6444004775717708799, -0.5364919789714476250 ) ) ;
#46355 = ORIENTED_EDGE ( 'NONE', *, *, #1561, .T. ) ;
#46356 = CARTESIAN_POINT ( 'NONE',  ( -12.70458494993575194, -0.1191753592594197858, 11.86531876794841978 ) ) ;
#46357 = PLANE ( 'NONE',  #32266 ) ;
#46358 = ORIENTED_EDGE ( 'NONE', *, *, #54169, .T. ) ;
#46359 = CARTESIAN_POINT ( 'NONE',  ( -68.93342745996714882, -0.9999999999999978906, -5.847034362371242189 ) ) ;
#46360 = CARTESIAN_POINT ( 'NONE',  ( -16.83070019881521517, 0.4483081953215033444, 3.205243883113554570 ) ) ;
#46361 = ADVANCED_FACE ( 'NONE', ( #34206 ), #16566, .F. ) ;
#46362 = LINE ( 'NONE', #30696, #44056 ) ;
#46363 = EDGE_CURVE ( 'NONE', #30649, #13281, #21947, .T. ) ;
#46364 = DIRECTION ( 'NONE',  ( -0.9999697198139514409, -0.000000000000000000, -0.007781995580013368816 ) ) ;
#46365 = AXIS2_PLACEMENT_3D ( 'NONE', #236, #25535, #42315 ) ;
#46366 = DIRECTION ( 'NONE',  ( 0.9321478471874540261, 0.000000000000000000, -0.3620778797217457101 ) ) ;
#46367 = ORIENTED_EDGE ( 'NONE', *, *, #3039, .F. ) ;
#46368 = EDGE_CURVE ( 'NONE', #46316, #23729, #20829, .T. ) ;
#46369 = ORIENTED_EDGE ( 'NONE', *, *, #50157, .T. ) ;
#46370 = CARTESIAN_POINT ( 'NONE',  ( -67.30190987268471758, -0.6009080523669287910, 2.678990660366964871 ) ) ;
#46371 = LINE ( 'NONE', #33351, #14982 ) ;
#46372 = LINE ( 'NONE', #50915, #50576 ) ;
#46373 = ADVANCED_FACE ( 'NONE', ( #8331 ), #56055, .F. ) ;
#46374 = CARTESIAN_POINT ( 'NONE',  ( -11.20636620717317378, 0.000000000000000000, 11.32298014792380414 ) ) ;
#46375 = DIRECTION ( 'NONE',  ( 0.007781995580012663651, 0.000000000000000000, -0.9999697198139515519 ) ) ;
#46376 = EDGE_CURVE ( 'NONE', #51697, #27027, #29925, .T. ) ;
#46377 = FACE_OUTER_BOUND ( 'NONE', #49614, .T. ) ;
#46378 = ORIENTED_EDGE ( 'NONE', *, *, #48405, .F. ) ;
#46379 = CARTESIAN_POINT ( 'NONE',  ( -19.51723258224034296, 0.000000000000000000, 4.499193495089023109 ) ) ;
#46380 = CARTESIAN_POINT ( 'NONE',  ( -17.23560250149814976, 0.000000000000000000, 9.856924658832747710 ) ) ;
#46381 = DIRECTION ( 'NONE',  ( 0.000000000000000000, -1.000000000000000000, 0.000000000000000000 ) ) ;
#46382 = ORIENTED_EDGE ( 'NONE', *, *, #37078, .F. ) ;
#46383 = CARTESIAN_POINT ( 'NONE',  ( -11.09304826722767956, 24.43504809471621186, -5.000000000000000888 ) ) ;
#46384 = DIRECTION ( 'NONE',  ( 1.007958083594381669E-15, -3.869188571150966625E-16, 1.000000000000000000 ) ) ;
#46385 = DIRECTION ( 'NONE',  ( 0.007781995580012663651, -3.146120232559066537E-19, -0.9999697198139514409 ) ) ;
#46386 = ORIENTED_EDGE ( 'NONE', *, *, #12978, .T. ) ;
#46387 = AXIS2_PLACEMENT_3D ( 'NONE', #34267, #38804, #4159 ) ;
#46388 = VECTOR ( 'NONE', #3890, 999.9999999999998863 ) ;
#46389 = CARTESIAN_POINT ( 'NONE',  ( -17.72271011234543536, -2.298917212465660054, 3.692076095354655418 ) ) ;
#46390 = ORIENTED_EDGE ( 'NONE', *, *, #12671, .T. ) ;
#46391 = B_SPLINE_CURVE_WITH_KNOTS ( 'NONE', 3,
 ( #29836, #42594, #43443, #26134 ),
 .UNSPECIFIED., .F., .F.,
 ( 4, 4 ),
 ( 0.0009679422276756598567, 0.001611251064783924929 ),
 .UNSPECIFIED. ) ;
#46392 = ORIENTED_EDGE ( 'NONE', *, *, #34456, .F. ) ;
#46393 = EDGE_LOOP ( 'NONE', ( #20603, #16993, #31430, #50682 ) ) ;
#46394 = VECTOR ( 'NONE', #46443, 1000.000000000000227 ) ;
#46395 = ORIENTED_EDGE ( 'NONE', *, *, #16802, .F. ) ;
#46396 = CARTESIAN_POINT ( 'NONE',  ( -32.65841372305263235, 0.000000000000000000, 9.367568705923016381 ) ) ;
#46397 = ORIENTED_EDGE ( 'NONE', *, *, #53935, .T. ) ;
#46398 = EDGE_CURVE ( 'NONE', #45566, #9012, #44374, .T. ) ;
#46399 = ORIENTED_EDGE ( 'NONE', *, *, #20942, .F. ) ;
#46400 = DIRECTION ( 'NONE',  ( -0.2426528472758541499, 0.7422098413412800966, -0.6246952433987894571 ) ) ;
#46401 = VERTEX_POINT ( 'NONE', #19858 ) ;
#46402 = VECTOR ( 'NONE', #39991, 999.9999999999998863 ) ;
#46403 = ORIENTED_EDGE ( 'NONE', *, *, #29162, .T. ) ;
#46404 = ADVANCED_FACE ( 'NONE', ( #10015 ), #5475, .F. ) ;
#46405 = EDGE_CURVE ( 'NONE', #37937, #16343, #22790, .T. ) ;
#46406 = VECTOR ( 'NONE', #39232, 1000.000000000000227 ) ;
#46407 = LINE ( 'NONE', #41046, #7514 ) ;
#46408 = DIRECTION ( 'NONE',  ( -0.9999697198139514409, -0.000000000000000000, -0.007781995580013368816 ) ) ;
#46409 = DIRECTION ( 'NONE',  ( 0.9999697198139515519, 0.000000000000000000, 0.007781995580013368816 ) ) ;
#46410 = DIRECTION ( 'NONE',  ( 0.005002170337468016433, -0.7660444431189770143, -0.6427681459581293666 ) ) ;
#46411 = ORIENTED_EDGE ( 'NONE', *, *, #526, .F. ) ;
#46412 = EDGE_LOOP ( 'NONE', ( #3471, #25498, #44591 ) ) ;
#46413 = DIRECTION ( 'NONE',  ( 0.7660212471507180654, -0.6427876096865404731, 0.005961354470445141482 ) ) ;
#46414 = CARTESIAN_POINT ( 'NONE',  ( -20.54049170961573267, 0.000000000000000000, 4.660556269540326646 ) ) ;
#46415 = CARTESIAN_POINT ( 'NONE',  ( -37.71704171767562741, 10.88233165714454920, -4.934322635580619121 ) ) ;
#46416 = CARTESIAN_POINT ( 'NONE',  ( -15.88130887279446490, 0.000000000000000000, 3.050160814894388839 ) ) ;
#46417 = CARTESIAN_POINT ( 'NONE',  ( -11.71187600135471030, -0.1191753592594190225, 3.721269417090256049 ) ) ;
#46418 = CARTESIAN_POINT ( 'NONE',  ( 2.072287782118878319, 0.000000000000000000, -2.950529333540147015 ) ) ;
#46419 = ORIENTED_EDGE ( 'NONE', *, *, #3610, .T. ) ;
#46420 = CARTESIAN_POINT ( 'NONE',  ( 2.072287782118878319, 0.000000000000000000, -2.950529333540147015 ) ) ;
#46421 = DIRECTION ( 'NONE',  ( 0.7660212471507180654, -0.6427876096865404731, 0.005961354470445141482 ) ) ;
#46422 = ORIENTED_EDGE ( 'NONE', *, *, #20827, .T. ) ;
#46423 = VECTOR ( 'NONE', #2538, 999.9999999999998863 ) ;
#46424 = VECTOR ( 'NONE', #30389, 1000.000000000000227 ) ;
#46425 = PLANE ( 'NONE',  #37938 ) ;
#46426 = DIRECTION ( 'NONE',  ( 0.005961354470445682716, -0.6427876096865404731, -0.7660212471507180654 ) ) ;
#46427 = CARTESIAN_POINT ( 'NONE',  ( -30.79567442779373110, 0.000000000000000000, 8.843406890442315316 ) ) ;
#46428 = PLANE ( 'NONE',  #18699 ) ;
#46429 = EDGE_CURVE ( 'NONE', #49589, #12571, #40108, .T. ) ;
#46430 = FACE_OUTER_BOUND ( 'NONE', #45310, .T. ) ;
#46431 = EDGE_LOOP ( 'NONE', ( #22623, #10573, #27995, #1071 ) ) ;
#46432 = VECTOR ( 'NONE', #10454, 999.9999999999998863 ) ;
#46433 = AXIS2_PLACEMENT_3D ( 'NONE', #22140, #10195, #36069 ) ;
#46434 = EDGE_CURVE ( 'NONE', #29543, #29153, #10298, .T. ) ;
#46435 = EDGE_LOOP ( 'NONE', ( #22121, #7073, #12813, #49728 ) ) ;
#46436 = CARTESIAN_POINT ( 'NONE',  ( -12.75218409439548850, 3.848249166794009746, 8.150334972661291033 ) ) ;
#46437 = DIRECTION ( 'NONE',  ( -0.6427681459581293666, -0.7660444431189770143, -0.005002170337467561935 ) ) ;
#46438 = CARTESIAN_POINT ( 'NONE',  ( -26.21622229497770817, 17.48042152905857449, -4.621141326338904065 ) ) ;
#46439 = DIRECTION ( 'NONE',  ( 0.5449076811759707706, 0.6444004775717708799, -0.5364919789714476250 ) ) ;
#46440 = EDGE_CURVE ( 'NONE', #34418, #21379, #22532, .T. ) ;
#46441 = VECTOR ( 'NONE', #43567, 1000.000000000000227 ) ;
#46442 = PLANE ( 'NONE',  #31205 ) ;
#46443 = DIRECTION ( 'NONE',  ( 0.007781995580012663651, -3.146120232559066537E-19, -0.9999697198139514409 ) ) ;
#46444 = CARTESIAN_POINT ( 'NONE',  ( -26.13493519185646008, 0.000000000000000000, 7.033017491833586377 ) ) ;
#46445 = CARTESIAN_POINT ( 'NONE',  ( -67.14101802347384762, -8.387388012353506284, -2.442027903730112026 ) ) ;
#46446 = DIRECTION ( 'NONE',  ( 0.9321478471874540261, 0.000000000000000000, -0.3620778797217456546 ) ) ;
#46447 = ORIENTED_EDGE ( 'NONE', *, *, #28371, .F. ) ;
#46448 = LINE ( 'NONE', #25738, #31298 ) ;
#46449 = EDGE_CURVE ( 'NONE', #9219, #37763, #11342, .T. ) ;
#46450 = ORIENTED_EDGE ( 'NONE', *, *, #20676, .F. ) ;
#46451 = VECTOR ( 'NONE', #8973, 999.9999999999998863 ) ;
#46452 = EDGE_CURVE ( 'NONE', #39023, #3804, #27065, .T. ) ;
#46453 = EDGE_LOOP ( 'NONE', ( #20226, #36791, #35133, #32539 ) ) ;
#46454 = VERTEX_POINT ( 'NONE', #44943 ) ;
#46455 = EDGE_LOOP ( 'NONE', ( #18391, #53052, #7852, #7184 ) ) ;
#46456 = ORIENTED_EDGE ( 'NONE', *, *, #31484, .T. ) ;
#46457 = LINE ( 'NONE', #7580, #23285 ) ;
#46458 = CARTESIAN_POINT ( 'NONE',  ( -21.14709236723027530, 3.362543313726509719, 4.788897828647994181 ) ) ;
#46459 = ADVANCED_FACE ( 'NONE', ( #44637 ), #37177, .F. ) ;
#46460 = CARTESIAN_POINT ( 'NONE',  ( -14.49613859905933211, -0.6798977022406558213, 2.490421343638416829 ) ) ;
#46461 = VECTOR ( 'NONE', #16098, 1000.000000000000114 ) ;
#46462 = VECTOR ( 'NONE', #8450, 999.9999999999998863 ) ;
#46464 = EDGE_CURVE ( 'NONE', #25142, #16114, #23080, .T. ) ;
#46463 = ORIENTED_EDGE ( 'NONE', *, *, #39709, .F. ) ;
#46465 = LINE ( 'NONE', #28897, #39466 ) ;
#46466 = ORIENTED_EDGE ( 'NONE', *, *, #20839, .T. ) ;
#46467 = LINE ( 'NONE', #12435, #8683 ) ;
#46468 = ORIENTED_EDGE ( 'NONE', *, *, #911, .F. ) ;
#46469 = ADVANCED_FACE ( 'NONE', ( #17988 ), #6065, .F. ) ;
#46470 = VECTOR ( 'NONE', #28447, 1000.000000000000000 ) ;
#46471 = AXIS2_PLACEMENT_3D ( 'NONE', #28864, #24573, #49318 ) ;
#46472 = CARTESIAN_POINT ( 'NONE',  ( -68.77136691953549530, -8.975737434388888047, 7.030741166004676579 ) ) ;
#46473 = CARTESIAN_POINT ( 'NONE',  ( -15.13495153988577968, 0.000000000000000000, 12.76973526769478084 ) ) ;
#46474 = DIRECTION ( 'NONE',  ( -0.9999697198139514409, -0.000000000000000000, -0.007781995580013368816 ) ) ;
#46475 = ORIENTED_EDGE ( 'NONE', *, *, #36729, .F. ) ;
#46476 = CARTESIAN_POINT ( 'NONE',  ( -13.20500546430136346, 0.000000000000000000, 3.609646510246834694 ) ) ;
#46477 = ORIENTED_EDGE ( 'NONE', *, *, #11938, .F. ) ;
#46478 = ADVANCED_FACE ( 'NONE', ( #36155 ), #53455, .F. ) ;
#46479 = PLANE ( 'NONE',  #5555 ) ;
#46480 = AXIS2_PLACEMENT_3D ( 'NONE', #17897, #31779, #31519 ) ;
#46481 = LINE ( 'NONE', #15834, #31153 ) ;
#46482 = TOROIDAL_SURFACE ( 'NONE', #35738, 3.457106781186553235, 0.2500000000000000000 ) ;
#46483 = EDGE_CURVE ( 'NONE', #48923, #43832, #32915, .T. ) ;
#46484 = CARTESIAN_POINT ( 'NONE',  ( -10.94028622754223967, 0.000000000000000000, 11.14038480894692995 ) ) ;
#46485 = CARTESIAN_POINT ( 'NONE',  ( -18.29747203306047609, -0.1191753592594177458, 14.03778604627889059 ) ) ;
#46486 = LINE ( 'NONE', #51876, #44715 ) ;
#46487 = CARTESIAN_POINT ( 'NONE',  ( -16.81345671998191449, 0.000000000000000000, 3.412238694616132495 ) ) ;
#46488 = DIRECTION ( 'NONE',  ( 0.5449076811759707706, 0.6444004775717708799, -0.5364919789714476250 ) ) ;
#46489 = FACE_OUTER_BOUND ( 'NONE', #14134, .T. ) ;
#46490 = EDGE_LOOP ( 'NONE', ( #15518, #28424 ) ) ;
#46491 = CARTESIAN_POINT ( 'NONE',  ( -17.43300170430006091, 0.6102101463440035012, 3.434032722201703081 ) ) ;
#46492 = VERTEX_POINT ( 'NONE', #53201 ) ;
#46493 = CIRCLE ( 'NONE', #26570, 2.125000000000000000 ) ;
#46494 = DIRECTION ( 'NONE',  ( -0.9999697198139514409, -0.000000000000000000, -0.007781995580013368816 ) ) ;
#46495 = CARTESIAN_POINT ( 'NONE',  ( -23.33849165029409889, 0.000000000000000000, 5.946783852668351855 ) ) ;
#46496 = CARTESIAN_POINT ( 'NONE',  ( -8.609916609573598834, 0.000000000000000000, 10.23519010964256637 ) ) ;
#46497 = AXIS2_PLACEMENT_3D ( 'NONE', #50223, #28667, #49692 ) ;
#46498 = DIRECTION ( 'NONE',  ( 0.5364919789714477361, 0.6444004775717706579, 0.5449076811759711036 ) ) ;
#46499 = CARTESIAN_POINT ( 'NONE',  ( -15.33681816505984763, 0.000000000000000000, 4.701052460296081925 ) ) ;
#46500 = LINE ( 'NONE', #46223, #49288 ) ;
#46501 = ORIENTED_EDGE ( 'NONE', *, *, #37848, .T. ) ;
#46502 = DIRECTION ( 'NONE',  ( 0.005961354470445682716, -0.6427876096865404731, -0.7660212471507180654 ) ) ;
#46503 = VECTOR ( 'NONE', #24668, 1000.000000000000227 ) ;
#46504 = DIRECTION ( 'NONE',  ( -0.005002170337468016433, -0.7660444431189770143, 0.6427681459581293666 ) ) ;
#46505 = CARTESIAN_POINT ( 'NONE',  ( -10.30359504330503917, -0.1191753592594205352, 1.885568636105463547 ) ) ;
#46506 = CARTESIAN_POINT ( 'NONE',  ( -18.67775241435682432, 0.000000000000000000, 4.136394454059623804 ) ) ;
#46507 = VECTOR ( 'NONE', #52968, 1000.000000000000227 ) ;
#46508 = AXIS2_PLACEMENT_3D ( 'NONE', #27113, #418, #4973 ) ;
#46509 = FACE_OUTER_BOUND ( 'NONE', #52211, .T. ) ;
#46510 = EDGE_CURVE ( 'NONE', #7643, #14573, #50230, .T. ) ;
#46511 = FACE_OUTER_BOUND ( 'NONE', #1782, .T. ) ;
#46512 = FACE_OUTER_BOUND ( 'NONE', #14021, .T. ) ;
#46513 = DIRECTION ( 'NONE',  ( 0.007781995580012663651, 0.000000000000000000, -0.9999697198139515519 ) ) ;
#46514 = ORIENTED_EDGE ( 'NONE', *, *, #29835, .T. ) ;
#46515 = VECTOR ( 'NONE', #1707, 999.9999999999998863 ) ;
#46516 = DIRECTION ( 'NONE',  ( 0.007781995580012662783, 0.000000000000000000, -0.9999697198139514409 ) ) ;
#46517 = AXIS2_PLACEMENT_3D ( 'NONE', #13078, #30408, #7992 ) ;
#46518 = CARTESIAN_POINT ( 'NONE',  ( -19.07403171432551758, 0.000000000000000000, 7.257293088956358496 ) ) ;
#46519 = ORIENTED_EDGE ( 'NONE', *, *, #20239, .F. ) ;
#46520 = ORIENTED_EDGE ( 'NONE', *, *, #52219, .F. ) ;
#46521 = LINE ( 'NONE', #46242, #30114 ) ;
#46522 = EDGE_CURVE ( 'NONE', #6267, #44587, #4921, .T. ) ;
#46523 = ORIENTED_EDGE ( 'NONE', *, *, #18929, .F. ) ;
#46524 = AXIS2_PLACEMENT_3D ( 'NONE', #8813, #47966, #43430 ) ;
#46525 = EDGE_LOOP ( 'NONE', ( #9901, #11323, #31449, #39005 ) ) ;
#46526 = LINE ( 'NONE', #38029, #49237 ) ;
#46527 = EDGE_CURVE ( 'NONE', #15160, #9839, #35309, .T. ) ;
#46528 = VECTOR ( 'NONE', #52692, 999.9999999999998863 ) ;
#46529 = EDGE_CURVE ( 'NONE', #19170, #12202, #48344, .T. ) ;
#46530 = VERTEX_POINT ( 'NONE', #25256 ) ;
#46531 = VERTEX_POINT ( 'NONE', #28950 ) ;
#46532 = ORIENTED_EDGE ( 'NONE', *, *, #47239, .F. ) ;
#46533 = CARTESIAN_POINT ( 'NONE',  ( -14.46888367232926420, 0.000000000000000000, 12.59025272694991315 ) ) ;
#46534 = DIRECTION ( 'NONE',  ( 0.5364919789714477361, 0.6444004775717706579, 0.5449076811759711036 ) ) ;
#46535 = B_SPLINE_CURVE_WITH_KNOTS ( 'NONE', 3,
 ( #2462, #50138, #32566, #15498 ),
 .UNSPECIFIED., .F., .F.,
 ( 4, 4 ),
 ( 0.3513510006676737740, 0.3765591803097264045 ),
 .UNSPECIFIED. ) ;
#46536 = LINE ( 'NONE', #42844, #14916 ) ;
#46537 = VECTOR ( 'NONE', #10637, 1000.000000000000227 ) ;
#46538 = EDGE_CURVE ( 'NONE', #38354, #19178, #46521, .T. ) ;
#46539 = EDGE_LOOP ( 'NONE', ( #538, #42515, #25819, #41116 ) ) ;
#46540 = ORIENTED_EDGE ( 'NONE', *, *, #18074, .F. ) ;
#46541 = AXIS2_PLACEMENT_3D ( 'NONE', #39001, #51765, #12874 ) ;
#46542 = ADVANCED_FACE ( 'NONE', ( #20419 ), #50532, .F. ) ;
#46543 = CARTESIAN_POINT ( 'NONE',  ( -65.69080466243542560, -1.561251128379126069E-14, 1.648866456817433823 ) ) ;
#46544 = DIRECTION ( 'NONE',  ( -0.7660212471507179544, -0.6427876096865405842, -0.005961354470445141482 ) ) ;
#46545 = EDGE_LOOP ( 'NONE', ( #24843, #10103, #13655, #43728 ) ) ;
#46546 = AXIS2_PLACEMENT_3D ( 'NONE', #37063, #24281, #54361 ) ;
#46547 = DIRECTION ( 'NONE',  ( -0.5364919789714478471, 0.6444004775717705469, -0.5449076811759709926 ) ) ;
#46548 = ORIENTED_EDGE ( 'NONE', *, *, #45761, .F. ) ;
#46549 = LINE ( 'NONE', #39387, #54802 ) ;
#46550 = CARTESIAN_POINT ( 'NONE',  ( -19.22790012936460613, -0.06318563913204579274, 8.141745193239319889 ) ) ;
#46551 = VECTOR ( 'NONE', #20799, 1000.000000000000227 ) ;
#46552 = EDGE_CURVE ( 'NONE', #21327, #29513, #24969, .T. ) ;
#46553 = AXIS2_PLACEMENT_3D ( 'NONE', #44786, #31161, #9604 ) ;
#46554 = ORIENTED_EDGE ( 'NONE', *, *, #4962, .T. ) ;
#46555 = DIRECTION ( 'NONE',  ( 0.005961354470445682716, -0.6427876096865404731, -0.7660212471507180654 ) ) ;
#46556 = ADVANCED_FACE ( 'NONE', ( #51068, #38024, #15879 ), #41702, .F. ) ;
#46557 = AXIS2_PLACEMENT_3D ( 'NONE', #24958, #43403, #38867 ) ;
#46558 = LINE ( 'NONE', #7378, #9130 ) ;
#46559 = VECTOR ( 'NONE', #4831, 1000.000000000000114 ) ;
#46560 = ORIENTED_EDGE ( 'NONE', *, *, #24144, .T. ) ;
#46561 = LINE ( 'NONE', #8229, #47621 ) ;
#46562 = CARTESIAN_POINT ( 'NONE',  ( -31.72626587586518099, 0.000000000000000000, 9.005490826201270949 ) ) ;
#46563 = LINE ( 'NONE', #42329, #16695 ) ;
#46564 = CARTESIAN_POINT ( 'NONE',  ( -14.60909471445646979, 0.000000000000000000, 4.906721828678888286 ) ) ;
#46565 = ORIENTED_EDGE ( 'NONE', *, *, #26362, .F. ) ;
#46566 = CARTESIAN_POINT ( 'NONE',  ( -15.19872173456531250, -2.622721114510660367, 2.701342254643969376 ) ) ;
#46567 = DIRECTION ( 'NONE',  ( 0.000000000000000000, -0.000000000000000000, -1.000000000000000000 ) ) ;
#46568 = PLANE ( 'NONE',  #7681 ) ;
#46569 = LINE ( 'NONE', #47723, #53141 ) ;
#46570 = DIRECTION ( 'NONE',  ( 0.005961354470445682716, -0.6427876096865404731, -0.7660212471507180654 ) ) ;
#46571 = LINE ( 'NONE', #33799, #34266 ) ;
#46572 = LINE ( 'NONE', #28419, #6804 ) ;
#46573 = VECTOR ( 'NONE', #26509, 1000.000000000000227 ) ;
#46574 = VERTEX_POINT ( 'NONE', #29516 ) ;
#46575 = CARTESIAN_POINT ( 'NONE',  ( -16.02444143390598796, 0.000000000000000000, 7.650357775474186717 ) ) ;
#46576 = PLANE ( 'NONE',  #33233 ) ;
#46577 = EDGE_LOOP ( 'NONE', ( #21714, #36373, #55665, #54251 ) ) ;
#46578 = DIRECTION ( 'NONE',  ( -0.7660212471507179544, -0.6427876096865405842, -0.005961354470445141482 ) ) ;
#46579 = CARTESIAN_POINT ( 'NONE',  ( -12.19663127273277681, -0.1191753592594185784, 6.302821428126598846 ) ) ;
#46580 = AXIS2_PLACEMENT_3D ( 'NONE', #36888, #9922, #6227 ) ;
#46581 = DIRECTION ( 'NONE',  ( 0.9999697198139515519, 0.000000000000000000, 0.007781995580013368816 ) ) ;
#46582 = EDGE_CURVE ( 'NONE', #46034, #44456, #34337, .T. ) ;
#46583 = VECTOR ( 'NONE', #8760, 1000.000000000000000 ) ;
#46584 = LINE ( 'NONE', #33282, #6112 ) ;
#46585 = DIRECTION ( 'NONE',  ( 0.9999697198139515519, 0.000000000000000000, 0.007781995580013368816 ) ) ;
#46586 = ORIENTED_EDGE ( 'NONE', *, *, #30229, .F. ) ;
#46587 = ADVANCED_FACE ( 'NONE', ( #16427 ), #33749, .F. ) ;
#46588 = VERTEX_POINT ( 'NONE', #12176 ) ;
#46589 = LINE ( 'NONE', #7708, #49479 ) ;
#46590 = VECTOR ( 'NONE', #14247, 999.9999999999998863 ) ;
#46591 = DIRECTION ( 'NONE',  ( -0.2426528472758541499, 0.7422098413412800966, -0.6246952433987894571 ) ) ;
#46592 = EDGE_CURVE ( 'NONE', #53062, #15552, #42562, .T. ) ;
#46593 = EDGE_CURVE ( 'NONE', #29013, #54969, #7944, .T. ) ;
#46594 = EDGE_CURVE ( 'NONE', #37965, #20238, #25513, .T. ) ;
#46595 = VECTOR ( 'NONE', #15918, 999.9999999999998863 ) ;
#46596 = CARTESIAN_POINT ( 'NONE',  ( -20.54204810873173415, 0.000000000000000000, 4.860550213503115558 ) ) ;
#46597 = ORIENTED_EDGE ( 'NONE', *, *, #32908, .F. ) ;
#46598 = CARTESIAN_POINT ( 'NONE',  ( -13.99061985836883437, 0.9340140483890049250, 3.848629169735781730 ) ) ;
#46599 = VERTEX_POINT ( 'NONE', #3651 ) ;
#46600 = CARTESIAN_POINT ( 'NONE',  ( -22.42633980038347730, -4.565544526780663581, 5.446808323701739951 ) ) ;
#46601 = EDGE_CURVE ( 'NONE', #33592, #5503, #55918, .T. ) ;
#46602 = AXIS2_PLACEMENT_3D ( 'NONE', #14643, #14928, #10693 ) ;
#46603 = EDGE_LOOP ( 'NONE', ( #53533, #31498, #15974, #17441 ) ) ;
#46604 = VECTOR ( 'NONE', #53269, 1000.000000000000227 ) ;
#46605 = VERTEX_POINT ( 'NONE', #2791 ) ;
#46606 = ORIENTED_EDGE ( 'NONE', *, *, #26825, .F. ) ;
#46607 = DIRECTION ( 'NONE',  ( 0.5449076811759707706, 0.6444004775717708799, -0.5364919789714476250 ) ) ;
#46608 = DIRECTION ( 'NONE',  ( 0.000000000000000000, -0.000000000000000000, -1.000000000000000000 ) ) ;
#46609 = DIRECTION ( 'NONE',  ( -0.5364919789714478471, 0.6444004775717705469, -0.5449076811759709926 ) ) ;
#46610 = FACE_OUTER_BOUND ( 'NONE', #1191, .T. ) ;
#46611 = EDGE_CURVE ( 'NONE', #44519, #7829, #49152, .T. ) ;
#46612 = ORIENTED_EDGE ( 'NONE', *, *, #5661, .T. ) ;
#46614 = ORIENTED_EDGE ( 'NONE', *, *, #32690, .F. ) ;
#46613 = ADVANCED_FACE ( 'NONE', ( #20116 ), #51379, .F. ) ;
#46615 = VECTOR ( 'NONE', #36814, 1000.000000000000227 ) ;
#46616 = ORIENTED_EDGE ( 'NONE', *, *, #16702, .T. ) ;
#46617 = DIRECTION ( 'NONE',  ( 0.5364919789714477361, 0.6444004775717706579, 0.5449076811759711036 ) ) ;
#46618 = AXIS2_PLACEMENT_3D ( 'NONE', #44386, #26502, #39596 ) ;
#46619 = LINE ( 'NONE', #21643, #36721 ) ;
#46620 = ADVANCED_FACE ( 'NONE', ( #29207 ), #51640, .F. ) ;
#46621 = ORIENTED_EDGE ( 'NONE', *, *, #1863, .F. ) ;
#46622 = FACE_OUTER_BOUND ( 'NONE', #24869, .T. ) ;
#46623 = ORIENTED_EDGE ( 'NONE', *, *, #28227, .F. ) ;
#46624 = VECTOR ( 'NONE', #32554, 999.9999999999998863 ) ;
#46625 = CARTESIAN_POINT ( 'NONE',  ( -17.32775551252169777, -0.1191753592594162470, 8.848214321482844369 ) ) ;
#46626 = LINE ( 'NONE', #16246, #1306 ) ;
#46627 = EDGE_CURVE ( 'NONE', #13033, #7193, #45992, .T. ) ;
#46628 = VERTEX_POINT ( 'NONE', #7640 ) ;
#46629 = PLANE ( 'NONE',  #16815 ) ;
#46630 = VECTOR ( 'NONE', #34845, 999.9999999999998863 ) ;
#46631 = ORIENTED_EDGE ( 'NONE', *, *, #15292, .T. ) ;
#46632 = CARTESIAN_POINT ( 'NONE',  ( 2.072287782118878319, 0.000000000000000000, -2.950529333540147015 ) ) ;
#46633 = DIRECTION ( 'NONE',  ( -0.005961354470445682716, -0.6427876096865404731, 0.7660212471507180654 ) ) ;
#46634 = ORIENTED_EDGE ( 'NONE', *, *, #55716, .F. ) ;
#46635 = FACE_OUTER_BOUND ( 'NONE', #43145, .T. ) ;
#46636 = DIRECTION ( 'NONE',  ( -0.5449076811759708816, 0.6444004775717707689, 0.5364919789714475140 ) ) ;
#46637 = DIRECTION ( 'NONE',  ( 0.000000000000000000, -1.000000000000000000, 0.000000000000000000 ) ) ;
#46638 = VECTOR ( 'NONE', #41176, 999.9999999999998863 ) ;
#46639 = CARTESIAN_POINT ( 'NONE',  ( -18.67619601524082285, 0.000000000000000000, 3.936400510096834893 ) ) ;
#46640 = ORIENTED_EDGE ( 'NONE', *, *, #24842, .T. ) ;
#46641 = VECTOR ( 'NONE', #33183, 1000.000000000000227 ) ;
#46642 = EDGE_LOOP ( 'NONE', ( #6020, #20120, #14102, #16013 ) ) ;
#46643 = FACE_OUTER_BOUND ( 'NONE', #4170, .T. ) ;
#46644 = CARTESIAN_POINT ( 'NONE',  ( -25.20278734466900517, 0.000000000000000000, 6.670939612111840944 ) ) ;
#46645 = DIRECTION ( 'NONE',  ( 0.007781995580012662783, 0.000000000000000000, -0.9999697198139514409 ) ) ;
#46646 = DIRECTION ( 'NONE',  ( 0.007781995580012662783, 0.000000000000000000, -0.9999697198139514409 ) ) ;
#46647 = DIRECTION ( 'NONE',  ( 0.007781995580012663651, 0.000000000000000000, -0.9999697198139515519 ) ) ;
#46648 = AXIS2_PLACEMENT_3D ( 'NONE', #30886, #31742, #43657 ) ;
#46649 = VECTOR ( 'NONE', #28365, 1000.000000000000227 ) ;
#46650 = DIRECTION ( 'NONE',  ( 0.000000000000000000, -0.000000000000000000, -1.000000000000000000 ) ) ;
#46651 = ORIENTED_EDGE ( 'NONE', *, *, #18661, .T. ) ;
#46652 = DIRECTION ( 'NONE',  ( 0.007781995580012663651, 0.000000000000000000, -0.9999697198139515519 ) ) ;
#46653 = PLANE ( 'NONE',  #38660 ) ;
#46654 = ORIENTED_EDGE ( 'NONE', *, *, #26298, .F. ) ;
#46655 = LINE ( 'NONE', #32504, #22289 ) ;
#46656 = ORIENTED_EDGE ( 'NONE', *, *, #45263, .T. ) ;
#46657 = CARTESIAN_POINT ( 'NONE',  ( -11.17520446802705614, 0.000000000000000000, 7.318763589012519333 ) ) ;
#46658 = LINE ( 'NONE', #32755, #2466 ) ;
#46659 = EDGE_CURVE ( 'NONE', #24728, #9006, #3392, .T. ) ;
#46660 = DIRECTION ( 'NONE',  ( 0.005961354470445682716, -0.6427876096865404731, -0.7660212471507180654 ) ) ;
#46661 = CARTESIAN_POINT ( 'NONE',  ( -24.26908309836554878, 0.000000000000000000, 6.108867788427308376 ) ) ;
#46662 = CARTESIAN_POINT ( 'NONE',  ( -67.39221309084119582, 0.1329240779904678482, -1.367029069770140604 ) ) ;
#46663 = AXIS2_PLACEMENT_3D ( 'NONE', #40249, #44790, #49625 ) ;
#46664 = EDGE_LOOP ( 'NONE', ( #44188, #7650, #18237, #27994 ) ) ;
#46665 = ORIENTED_EDGE ( 'NONE', *, *, #21253, .F. ) ;
#46666 = AXIS2_PLACEMENT_3D ( 'NONE', #35828, #53151, #5177 ) ;
#46667 = DIRECTION ( 'NONE',  ( 0.000000000000000000, -0.000000000000000000, -1.000000000000000000 ) ) ;
#46668 = DIRECTION ( 'NONE',  ( 0.6427681459581294776, -0.7660444431189769032, 0.005002170337467562802 ) ) ;
#46669 = DIRECTION ( 'NONE',  ( 0.5000000000000011102, -0.8660254037844380415, 0.000000000000000000 ) ) ;
#46670 = VECTOR ( 'NONE', #49979, 1000.000000000000227 ) ;
#46671 = ADVANCED_FACE ( 'NONE', ( #38877 ), #26636, .F. ) ;
#46672 = EDGE_CURVE ( 'NONE', #11685, #34978, #52742, .T. ) ;
#46673 = EDGE_CURVE ( 'NONE', #49950, #20904, #25812, .T. ) ;
#46674 = DIRECTION ( 'NONE',  ( -0.7660212471507179544, -0.6427876096865405842, -0.005961354470445141482 ) ) ;
#46675 = CARTESIAN_POINT ( 'NONE',  ( -18.67697421479882181, -0.1191753592594197858, 4.036397482078229793 ) ) ;
#46676 = PLANE ( 'NONE',  #40335 ) ;
#46677 = VECTOR ( 'NONE', #9725, 999.9999999999998863 ) ;
#46679 = EDGE_CURVE ( 'NONE', #37343, #25250, #18387, .T. ) ;
#46678 = ORIENTED_EDGE ( 'NONE', *, *, #44656, .T. ) ;
#46680 = CARTESIAN_POINT ( 'NONE',  ( -19.45503627000849889, 0.000000000000000000, 7.556996783084074742 ) ) ;
#46681 = PLANE ( 'NONE',  #36845 ) ;
#46682 = CARTESIAN_POINT ( 'NONE',  ( -14.16629225735672115, -0.8417996532631574214, 2.357132303004818130 ) ) ;
#46683 = ORIENTED_EDGE ( 'NONE', *, *, #50432, .F. ) ;
#46684 = AXIS2_PLACEMENT_3D ( 'NONE', #33560, #8576, #25067 ) ;
#46685 = DIRECTION ( 'NONE',  ( 0.000000000000000000, -0.000000000000000000, -1.000000000000000000 ) ) ;
#46686 = FACE_OUTER_BOUND ( 'NONE', #51782, .T. ) ;
#46687 = FACE_OUTER_BOUND ( 'NONE', #36515, .T. ) ;
#46688 = AXIS2_PLACEMENT_3D ( 'NONE', #39759, #577, #44003 ) ;
#46689 = VERTEX_POINT ( 'NONE', #47676 ) ;
#46690 = CARTESIAN_POINT ( 'NONE',  ( -20.69764258542294755, 20.51603762622108107, -4.338448882017707398 ) ) ;
#46691 = ORIENTED_EDGE ( 'NONE', *, *, #29487, .T. ) ;
#46692 = EDGE_CURVE ( 'NONE', #44862, #30431, #17865, .T. ) ;
#46693 = VECTOR ( 'NONE', #32240, 1000.000000000000000 ) ;
#46694 = ORIENTED_EDGE ( 'NONE', *, *, #50759, .T. ) ;
#46695 = VECTOR ( 'NONE', #52942, 999.9999999999998863 ) ;
#46696 = ORIENTED_EDGE ( 'NONE', *, *, #45706, .F. ) ;
#46697 = EDGE_CURVE ( 'NONE', #16476, #44308, #52212, .T. ) ;
#46698 = ORIENTED_EDGE ( 'NONE', *, *, #31713, .T. ) ;
#46699 = DIRECTION ( 'NONE',  ( -0.5364919789714478471, 0.6444004775717705469, -0.5449076811759709926 ) ) ;
#46700 = VERTEX_POINT ( 'NONE', #31179 ) ;
#46701 = PLANE ( 'NONE',  #52158 ) ;
#46702 = EDGE_CURVE ( 'NONE', #18842, #39017, #43665, .T. ) ;
#46703 = VERTEX_POINT ( 'NONE', #21562 ) ;
#46704 = PLANE ( 'NONE',  #36799 ) ;
#46705 = ORIENTED_EDGE ( 'NONE', *, *, #32567, .T. ) ;
#46706 = VERTEX_POINT ( 'NONE', #13580 ) ;
#46707 = EDGE_CURVE ( 'NONE', #39606, #18021, #44253, .T. ) ;
#46708 = AXIS2_PLACEMENT_3D ( 'NONE', #38430, #24810, #50378 ) ;
#46709 = LINE ( 'NONE', #16906, #42000 ) ;
#46710 = AXIS2_PLACEMENT_3D ( 'NONE', #37976, #26057, #51008 ) ;
#46711 = CARTESIAN_POINT ( 'NONE',  ( -15.33351336157133105, -1.651309408375655874, 5.348069112848596873 ) ) ;
#46712 = DIRECTION ( 'NONE',  ( -0.9335804264972041855, 0.3583679495452941066, 1.079669255038093093E-15 ) ) ;
#46713 = FACE_OUTER_BOUND ( 'NONE', #11208, .T. ) ;
#46714 = SURFACE_SIDE_STYLE ('',( #42172 ) ) ;
#46715 = VECTOR ( 'NONE', #18152, 1000.000000000000227 ) ;
#46716 = ORIENTED_EDGE ( 'NONE', *, *, #14638, .F. ) ;
#46717 = ORIENTED_EDGE ( 'NONE', *, *, #47322, .F. ) ;
#46718 = CARTESIAN_POINT ( 'NONE',  ( -18.82244137458435063, 0.000000000000000000, 8.936585358602211926 ) ) ;
#46719 = CARTESIAN_POINT ( 'NONE',  ( -10.74029228357944987, 0.000000000000000000, 11.14194120806293320 ) ) ;
#46720 = AXIS2_PLACEMENT_3D ( 'NONE', #20928, #38253, #4212 ) ;
#46721 = UNCERTAINTY_MEASURE_WITH_UNIT (LENGTH_MEASURE( 1.000000000000000082E-05 ), #30108, 'distance_accuracy_value', 'NONE');
#46722 = CARTESIAN_POINT ( 'NONE',  ( -16.79925329029790149, 0.000000000000000000, 13.49544742625427496 ) ) ;
#46723 = VECTOR ( 'NONE', #1780, 1000.000000000000227 ) ;
#46724 = VECTOR ( 'NONE', #2352, 1000.000000000000000 ) ;
#46725 = DIRECTION ( 'NONE',  ( 0.9999697198139515519, 0.000000000000000000, 0.007781995580013368816 ) ) ;
#46726 = VECTOR ( 'NONE', #39619, 1000.000000000000227 ) ;
#46727 = DIRECTION ( 'NONE',  ( -0.005002170337468016433, -0.7660444431189770143, 0.6427681459581293666 ) ) ;
#46728 = PLANE ( 'NONE',  #5102 ) ;
#46729 = ORIENTED_EDGE ( 'NONE', *, *, #45209, .F. ) ;
#46730 = DIRECTION ( 'NONE',  ( 0.2426528472758541499, 0.7422098413412800966, 0.6246952433987894571 ) ) ;
#46731 = CARTESIAN_POINT ( 'NONE',  ( -8.875996589204540044, 0.000000000000000000, 10.41778544861944233 ) ) ;
#46732 = ORIENTED_EDGE ( 'NONE', *, *, #5627, .T. ) ;
#46733 = VECTOR ( 'NONE', #10438, 999.9999999999998863 ) ;
#46734 = DIRECTION ( 'NONE',  ( 0.000000000000000000, -1.000000000000000000, 0.000000000000000000 ) ) ;
#46735 = CARTESIAN_POINT ( 'NONE',  ( 2.072287782118878319, 0.000000000000000000, -2.950529333540147015 ) ) ;
#46736 = VECTOR ( 'NONE', #38099, 999.9999999999998863 ) ;
#46737 = PLANE ( 'NONE',  #49897 ) ;
#46738 = DIRECTION ( 'NONE',  ( 0.005002170337468016433, -0.7660444431189770143, -0.6427681459581293666 ) ) ;
#46739 = FACE_OUTER_BOUND ( 'NONE', #53153, .T. ) ;
#46740 = VECTOR ( 'NONE', #5989, 1000.000000000000227 ) ;
#46741 = VERTEX_POINT ( 'NONE', #53046 ) ;
#46742 = VECTOR ( 'NONE', #25100, 1000.000000000000227 ) ;
#46743 = ORIENTED_EDGE ( 'NONE', *, *, #48981, .T. ) ;
#46744 = CARTESIAN_POINT ( 'NONE',  ( -9.110551994824897193, 0.000000000000000000, 3.538847790438064411 ) ) ;
#46745 = CARTESIAN_POINT ( 'NONE',  ( -19.95413052528122932, 21.13775321566489396, 4.283625658180314488 ) ) ;
#46746 = CARTESIAN_POINT ( 'NONE',  ( -20.54204810873173415, 0.000000000000000000, 4.860550213503115558 ) ) ;
#46747 = EDGE_CURVE ( 'NONE', #547, #26572, #1058, .T. ) ;
#46748 = CARTESIAN_POINT ( 'NONE',  ( -15.43560933383329292, -0.6798977022406551551, 3.793474551966180108 ) ) ;
#46749 = CARTESIAN_POINT ( 'NONE',  ( -17.74560456716937296, 0.000000000000000000, 3.774316574337878372 ) ) ;
#46750 = EDGE_CURVE ( 'NONE', #35444, #37821, #18116, .T. ) ;
#46751 = DIRECTION ( 'NONE',  ( -0.9999697198139514409, -0.000000000000000000, -0.007781995580013368816 ) ) ;
#46752 = EDGE_CURVE ( 'NONE', #4570, #4586, #35190, .T. ) ;
#46753 = DIRECTION ( 'NONE',  ( 0.000000000000000000, -1.000000000000000000, 0.000000000000000000 ) ) ;
#46754 = AXIS2_PLACEMENT_3D ( 'NONE', #43729, #12540, #17924 ) ;
#46755 = DIRECTION ( 'NONE',  ( -0.005002170337468016433, -0.7660444431189770143, 0.6427681459581293666 ) ) ;
#46756 = CARTESIAN_POINT ( 'NONE',  ( -66.90530812237336988, -8.360358167099661841, 0.5932824550257441709 ) ) ;
#46757 = AXIS2_PLACEMENT_3D ( 'NONE', #19752, #54644, #37914 ) ;
#46758 = DIRECTION ( 'NONE',  ( -0.7660212471507179544, -0.6427876096865405842, -0.005961354470445141482 ) ) ;
#46759 = ORIENTED_EDGE ( 'NONE', *, *, #32582, .T. ) ;
#46760 = DIRECTION ( 'NONE',  ( 0.007781995580012663651, -3.146120232559066537E-19, -0.9999697198139514409 ) ) ;
#46761 = VECTOR ( 'NONE', #34500, 1000.000000000000227 ) ;
#46762 = ORIENTED_EDGE ( 'NONE', *, *, #20724, .F. ) ;
#46763 = AXIS2_PLACEMENT_3D ( 'NONE', #18215, #18809, #22763 ) ;
#46764 = ORIENTED_EDGE ( 'NONE', *, *, #43336, .T. ) ;
#46765 = EDGE_LOOP ( 'NONE', ( #25507, #4868, #19064, #18905 ) ) ;
#46766 = ORIENTED_EDGE ( 'NONE', *, *, #44883, .F. ) ;
#46767 = AXIS2_PLACEMENT_3D ( 'NONE', #54312, #7746, #25074 ) ;
#46768 = VECTOR ( 'NONE', #36792, 1000.000000000000000 ) ;
#46769 = ORIENTED_EDGE ( 'NONE', *, *, #20659, .F. ) ;
#46770 = VERTEX_POINT ( 'NONE', #9622 ) ;
#46771 = DIRECTION ( 'NONE',  ( 0.000000000000000000, -1.000000000000000000, 0.000000000000000000 ) ) ;
#46772 = LINE ( 'NONE', #7893, #24772 ) ;
#46773 = FACE_OUTER_BOUND ( 'NONE', #32254, .T. ) ;
#46774 = VECTOR ( 'NONE', #50064, 999.9999999999998863 ) ;
#46775 = VECTOR ( 'NONE', #15479, 999.9999999999998863 ) ;
#46776 = ORIENTED_EDGE ( 'NONE', *, *, #4393, .T. ) ;
#46777 = CARTESIAN_POINT ( 'NONE',  ( -27.06708303904391144, 0.000000000000000000, 7.395095371555332697 ) ) ;
#46778 = ORIENTED_EDGE ( 'NONE', *, *, #6770, .T. ) ;
#46779 = CARTESIAN_POINT ( 'NONE',  ( -14.20280369269832832, 0.000000000000000000, 12.40765738797303719 ) ) ;
#46780 = ORIENTED_EDGE ( 'NONE', *, *, #54971, .T. ) ;
#46781 = EDGE_CURVE ( 'NONE', #50643, #3193, #43138, .T. ) ;
#46782 = AXIS2_PLACEMENT_3D ( 'NONE', #27140, #44448, #5551 ) ;
#46783 = VECTOR ( 'NONE', #20037, 1000.000000000000227 ) ;
#46784 = CARTESIAN_POINT ( 'NONE',  ( -66.02452298553313881, -9.265908444350362316, -1.783245832582586177 ) ) ;
#46785 = ADVANCED_FACE ( 'NONE', ( #22663 ), #39973, .F. ) ;
#46786 = LINE ( 'NONE', #52636, #43689 ) ;
#46787 = CARTESIAN_POINT ( 'NONE',  ( -68.51814297103354079, -10.99829263872246088, -7.485193420789068242 ) ) ;
#46788 = EDGE_LOOP ( 'NONE', ( #53475, #37452, #50186, #13795 ) ) ;
#46789 = CARTESIAN_POINT ( 'NONE',  ( -16.76809155115178385, 0.000000000000000000, 9.491230867342991928 ) ) ;
#46790 = VERTEX_POINT ( 'NONE', #8485 ) ;
#46791 = CARTESIAN_POINT ( 'NONE',  ( -19.25258962936204199, 0.000000000000000000, 4.501253007741028433 ) ) ;
#46792 = EDGE_CURVE ( 'NONE', #37525, #29163, #51907, .T. ) ;
#46793 = LINE ( 'NONE', #7909, #1221 ) ;
#46794 = VECTOR ( 'NONE', #35654, 999.9999999999998863 ) ;
#46795 = DIRECTION ( 'NONE',  ( -0.7660212471507179544, -0.6427876096865405842, -0.005961354470445141482 ) ) ;
#46796 = DIRECTION ( 'NONE',  ( 0.005961354470445682716, -0.6427876096865404731, -0.7660212471507180654 ) ) ;
#46797 = DIRECTION ( 'NONE',  ( 0.000000000000000000, -0.000000000000000000, -1.000000000000000000 ) ) ;
#46798 = CARTESIAN_POINT ( 'NONE',  ( -55.84246788140315942, 5.810395100437907523, 2.999999999999993339 ) ) ;
#46799 = CARTESIAN_POINT ( 'NONE',  ( -16.81190032086591302, 0.000000000000000000, 3.212244750653343583 ) ) ;
#46800 = CARTESIAN_POINT ( 'NONE',  ( -16.99924723426068951, 0.000000000000000000, 13.49389102713827171 ) ) ;
#46801 = ORIENTED_EDGE ( 'NONE', *, *, #41297, .T. ) ;
#46802 = DIRECTION ( 'NONE',  ( 0.000000000000000000, -1.000000000000000000, 0.000000000000000000 ) ) ;
#46803 = ORIENTED_EDGE ( 'NONE', *, *, #46821, .T. ) ;
#46804 = AXIS2_PLACEMENT_3D ( 'NONE', #32216, #19129, #15427 ) ;
#46805 = LINE ( 'NONE', #38852, #51914 ) ;
#46806 = PLANE ( 'NONE',  #31471 ) ;
#46807 = CARTESIAN_POINT ( 'NONE',  ( -8.875996589204540044, 0.000000000000000000, 10.41778544861944233 ) ) ;
#46808 = AXIS2_PLACEMENT_3D ( 'NONE', #12722, #34030, #16145 ) ;
#46809 = CARTESIAN_POINT ( 'NONE',  ( -11.77243710274829525, -0.1191753592594197858, 11.50324088822667612 ) ) ;
#46810 = DIRECTION ( 'NONE',  ( 0.000000000000000000, -0.000000000000000000, -1.000000000000000000 ) ) ;
#46811 = VECTOR ( 'NONE', #9356, 999.9999999999998863 ) ;
#46813 = AXIS2_PLACEMENT_3D ( 'NONE', #41269, #7451, #15414 ) ;
#46812 = CARTESIAN_POINT ( 'NONE',  ( -9.954103585529763265, 0.000000000000000000, 3.834951836585689389 ) ) ;
#46814 = ORIENTED_EDGE ( 'NONE', *, *, #25324, .F. ) ;
#46815 = LINE ( 'NONE', #32896, #30143 ) ;
#46816 = CARTESIAN_POINT ( 'NONE',  ( -22.95552628724609789, 17.67284575698099758, 4.512058519171590731 ) ) ;
#46817 = DIRECTION ( 'NONE',  ( 0.7660212471507180654, -0.6427876096865404731, 0.005961354470445141482 ) ) ;
#46818 = EDGE_CURVE ( 'NONE', #36758, #51910, #34593, .T. ) ;
#46819 = FACE_OUTER_BOUND ( 'NONE', #16903, .T. ) ;
#46820 = VECTOR ( 'NONE', #24852, 1000.000000000000227 ) ;
#46821 = EDGE_CURVE ( 'NONE', #49645, #37012, #22102, .T. ) ;
#46822 = VECTOR ( 'NONE', #49524, 999.9999999999998863 ) ;
#46823 = DIRECTION ( 'NONE',  ( 0.000000000000000000, -1.000000000000000000, 0.000000000000000000 ) ) ;
#46824 = LINE ( 'NONE', #48794, #4016 ) ;
#46825 = CARTESIAN_POINT ( 'NONE',  ( -14.10280672071693431, -0.1191753592594197858, 12.40843558753103792 ) ) ;
#46826 = EDGE_CURVE ( 'NONE', #4575, #3699, #26103, .T. ) ;
#46827 = CARTESIAN_POINT ( 'NONE',  ( -13.93584171313674958, 0.000000000000000000, 3.803965029789607044 ) ) ;
#46828 = VERTEX_POINT ( 'NONE', #39136 ) ;
#46829 = VECTOR ( 'NONE', #31260, 999.9999999999998863 ) ;
#46831 = FACE_OUTER_BOUND ( 'NONE', #27567, .T. ) ;
#46830 = AXIS2_PLACEMENT_3D ( 'NONE', #25110, #46107, #42420 ) ;
#46832 = DIRECTION ( 'NONE',  ( 0.5364919789714477361, 0.6444004775717706579, 0.5449076811759711036 ) ) ;
#46833 = ORIENTED_EDGE ( 'NONE', *, *, #9128, .F. ) ;
#46834 = VERTEX_POINT ( 'NONE', #30648 ) ;
#46835 = DIRECTION ( 'NONE',  ( 0.9999697198139515519, 0.000000000000000000, 0.007781995580013368816 ) ) ;
#46836 = ORIENTED_EDGE ( 'NONE', *, *, #19840, .T. ) ;
#46837 = PRODUCT_DEFINITION ( 'UNKNOWN', '', #21726, #29107 ) ;
#46838 = LINE ( 'NONE', #2795, #50159 ) ;
#46839 = VECTOR ( 'NONE', #11384, 999.9999999999998863 ) ;
#46840 = EDGE_CURVE ( 'NONE', #31761, #20073, #18698, .T. ) ;
#46841 = ORIENTED_EDGE ( 'NONE', *, *, #33178, .F. ) ;
#46842 = VERTEX_POINT ( 'NONE', #53342 ) ;
#46843 = EDGE_LOOP ( 'NONE', ( #48353, #44698, #3114, #1642 ) ) ;
#46844 = LINE ( 'NONE', #3945, #19322 ) ;
#46845 = DIRECTION ( 'NONE',  ( -0.7660212471507179544, -0.6427876096865405842, -0.005961354470445141482 ) ) ;
#46846 = VECTOR ( 'NONE', #23551, 1000.000000000000114 ) ;
#46847 = CARTESIAN_POINT ( 'NONE',  ( -15.88788263391494660, -0.1191753592594200495, 2.953019594114145274 ) ) ;
#46848 = AXIS2_PLACEMENT_3D ( 'NONE', #28043, #54166, #45347 ) ;
#46849 = EDGE_LOOP ( 'NONE', ( #9717, #39603, #24444, #29622 ) ) ;
#46850 = ORIENTED_EDGE ( 'NONE', *, *, #10986, .T. ) ;
#46851 = AXIS2_PLACEMENT_3D ( 'NONE', #38199, #46426, #50441 ) ;
#46852 = LINE ( 'NONE', #7366, #48421 ) ;
#46853 = CARTESIAN_POINT ( 'NONE',  ( -15.87975247367846166, 0.000000000000000000, 2.850166870931599927 ) ) ;
#46854 = ORIENTED_EDGE ( 'NONE', *, *, #49593, .T. ) ;
#46855 = CARTESIAN_POINT ( 'NONE',  ( -8.860905869600902207, 1.745854407020028306E-14, -4.599999999999999645 ) ) ;
#46856 = DIRECTION ( 'NONE',  ( 0.5449076811759707706, 0.6444004775717708799, -0.5364919789714476250 ) ) ;
#46857 = ORIENTED_EDGE ( 'NONE', *, *, #23661, .F. ) ;
#46858 = PLANE ( 'NONE',  #31226 ) ;
#46859 = DIRECTION ( 'NONE',  ( 0.007781995580012662783, 0.000000000000000000, -0.9999697198139514409 ) ) ;
#46860 = VERTEX_POINT ( 'NONE', #31748 ) ;
#46861 = AXIS2_PLACEMENT_3D ( 'NONE', #4806, #39461, #52510 ) ;
#46862 = DIRECTION ( 'NONE',  ( 0.5364919789714477361, 0.6444004775717706579, 0.5449076811759711036 ) ) ;
#46863 = EDGE_CURVE ( 'NONE', #5052, #33621, #49054, .T. ) ;
#46864 = VECTOR ( 'NONE', #46534, 999.9999999999998863 ) ;
#46865 = CARTESIAN_POINT ( 'NONE',  ( -17.42409743439815983, 2.017525632630139398, 12.78552735456895739 ) ) ;
#46866 = AXIS2_PLACEMENT_3D ( 'NONE', #32383, #19283, #49935 ) ;
#46867 = ORIENTED_EDGE ( 'NONE', *, *, #37307, .T. ) ;
#46868 = PLANE ( 'NONE',  #8632 ) ;
#46869 = FACE_OUTER_BOUND ( 'NONE', #34335, .T. ) ;
#46870 = CARTESIAN_POINT ( 'NONE',  ( -11.33783571642116783, 0.000000000000000000, 2.516181047545578586 ) ) ;
#46871 = CARTESIAN_POINT ( 'NONE',  ( -1.451368222102410455, 5.185123052344191130, 3.782134281800667797 ) ) ;
#46872 = VERTEX_POINT ( 'NONE', #27200 ) ;
#46873 = EDGE_CURVE ( 'NONE', #34917, #21011, #41090, .T. ) ;
#46874 = LINE ( 'NONE', #3688, #6568 ) ;
#46875 = DIRECTION ( 'NONE',  ( 0.000000000000000000, -1.000000000000000000, 0.000000000000000000 ) ) ;
#46876 = LINE ( 'NONE', #21006, #18545 ) ;
#46877 = CARTESIAN_POINT ( 'NONE',  ( -12.01504067337997483, -3.270328918600661439, 1.444030332666087268 ) ) ;
#46878 = EDGE_CURVE ( 'NONE', #55101, #54363, #53868, .T. ) ;
#46879 = DIRECTION ( 'NONE',  ( -0.6427681459581293666, -0.7660444431189770143, -0.005002170337467561935 ) ) ;
#46881 = EDGE_CURVE ( 'NONE', #16954, #349, #10983, .T. ) ;
#46880 = FACE_OUTER_BOUND ( 'NONE', #30457, .T. ) ;
#46882 = VECTOR ( 'NONE', #622, 1000.000000000000227 ) ;
#46883 = LINE ( 'NONE', #54819, #36718 ) ;
#46884 = ORIENTED_EDGE ( 'NONE', *, *, #46464, .T. ) ;
#46885 = CARTESIAN_POINT ( 'NONE',  ( -20.06674461129317422, -3.917936722690659401, 10.90653844675688156 ) ) ;
#46886 = EDGE_LOOP ( 'NONE', ( #88, #28172, #50611, #35344 ) ) ;
#46887 = FACE_OUTER_BOUND ( 'NONE', #20815, .T. ) ;
#46888 = EDGE_CURVE ( 'NONE', #19170, #17361, #44799, .T. ) ;
#46889 = DIRECTION ( 'NONE',  ( 0.000000000000000000, -0.000000000000000000, -1.000000000000000000 ) ) ;
#46890 = EDGE_CURVE ( 'NONE', #22139, #28250, #23238, .T. ) ;
#46891 = VECTOR ( 'NONE', #17789, 999.9999999999998863 ) ;
#46892 = DIRECTION ( 'NONE',  ( 0.6427681459581294776, -0.7660444431189769032, 0.005002170337467562802 ) ) ;
#46893 = CARTESIAN_POINT ( 'NONE',  ( -14.26657388737785936, -2.622721114510660367, 2.339264374922224388 ) ) ;
#46894 = EDGE_CURVE ( 'NONE', #40362, #25201, #10737, .T. ) ;
#46895 = LINE ( 'NONE', #26998, #7518 ) ;
#46896 = EDGE_LOOP ( 'NONE', ( #44717, #22775, #19683, #47240 ) ) ;
#46897 = VECTOR ( 'NONE', #44168, 999.9999999999998863 ) ;
#46898 = VERTEX_POINT ( 'NONE', #15265 ) ;
#46899 = LINE ( 'NONE', #37822, #39509 ) ;
#46900 = LINE ( 'NONE', #52279, #53134 ) ;
#46901 = ORIENTED_EDGE ( 'NONE', *, *, #46297, .F. ) ;
#46902 = LINE ( 'NONE', #3158, #49277 ) ;
#46903 = ADVANCED_FACE ( 'NONE', ( #45622 ), #44505, .F. ) ;
#46904 = VECTOR ( 'NONE', #43023, 1000.000000000000114 ) ;
#46905 = ORIENTED_EDGE ( 'NONE', *, *, #16058, .F. ) ;
#46906 = CARTESIAN_POINT ( 'NONE',  ( -12.23851102634202448, -0.1191753592594197858, 11.68427982808754884 ) ) ;
#46907 = ORIENTED_EDGE ( 'NONE', *, *, #851, .T. ) ;
#46908 = DIRECTION ( 'NONE',  ( 0.000000000000000000, -1.000000000000000000, 0.000000000000000000 ) ) ;
#46909 = EDGE_CURVE ( 'NONE', #13509, #28907, #18970, .T. ) ;
#46910 = ORIENTED_EDGE ( 'NONE', *, *, #7013, .F. ) ;
#46911 = ORIENTED_EDGE ( 'NONE', *, *, #39377, .F. ) ;
#46912 = VERTEX_POINT ( 'NONE', #14163 ) ;
#46913 = DIRECTION ( 'NONE',  ( -0.5364919789714478471, 0.6444004775717705469, -0.5449076811759709926 ) ) ;
#46914 = PLANE ( 'NONE',  #30509 ) ;
#46915 = DIRECTION ( 'NONE',  ( 0.007781995580012663651, -3.146120232559066537E-19, -0.9999697198139514409 ) ) ;
#46916 = CARTESIAN_POINT ( 'NONE',  ( -19.16801431701463443, 4.333955019861511992, 3.989163584846405985 ) ) ;
#46917 = EDGE_LOOP ( 'NONE', ( #46016, #39734, #14015, #1967 ) ) ;
#46918 = ORIENTED_EDGE ( 'NONE', *, *, #12951, .F. ) ;
#46919 = VERTEX_POINT ( 'NONE', #53588 ) ;
#46920 = CARTESIAN_POINT ( 'NONE',  ( -14.10280672071693431, -0.1191753592594197858, 12.40843558753103792 ) ) ;
#46921 = CARTESIAN_POINT ( 'NONE',  ( -14.03425665725284865, 0.4483081953215033444, 2.119010243948319161 ) ) ;
#46922 = VERTEX_POINT ( 'NONE', #31487 ) ;
#46923 = CARTESIAN_POINT ( 'NONE',  ( -27.99767448711536133, 0.000000000000000000, 7.557179307314289218 ) ) ;
#46924 = ORIENTED_EDGE ( 'NONE', *, *, #10264, .F. ) ;
#46925 = DIRECTION ( 'NONE',  ( 0.007781995580012663651, -3.146120232559066537E-19, -0.9999697198139514409 ) ) ;
#46926 = CARTESIAN_POINT ( 'NONE',  ( 2.072287782118878319, 0.000000000000000000, -2.950529333540147015 ) ) ;
#46927 = EDGE_LOOP ( 'NONE', ( #32785, #9332, #42507, #48430 ) ) ;
#46928 = FACE_OUTER_BOUND ( 'NONE', #16593, .T. ) ;
#46929 = EDGE_CURVE ( 'NONE', #7041, #1224, #36556, .T. ) ;
#46930 = EDGE_LOOP ( 'NONE', ( #49134, #8266, #6117 ) ) ;
#46931 = VECTOR ( 'NONE', #54090, 1000.000000000000227 ) ;
#46932 = CARTESIAN_POINT ( 'NONE',  ( -10.27421835998572064, 0.000000000000000000, 10.96090226820206048 ) ) ;
#46933 = LINE ( 'NONE', #25611, #53845 ) ;
#46934 = ORIENTED_EDGE ( 'NONE', *, *, #41643, .F. ) ;
#46935 = DIRECTION ( 'NONE',  ( 0.000000000000000000, -0.000000000000000000, -1.000000000000000000 ) ) ;
#46936 = DIRECTION ( 'NONE',  ( 0.007781995580012663651, 0.000000000000000000, -0.9999697198139515519 ) ) ;
#46937 = CARTESIAN_POINT ( 'NONE',  ( -15.76926926996742573, 4.172053068839010947, 2.674141106593023842 ) ) ;
#46938 = CARTESIAN_POINT ( 'NONE',  ( -16.81190032086591302, 0.000000000000000000, 3.212244750653343583 ) ) ;
#46939 = ORIENTED_EDGE ( 'NONE', *, *, #49838, .F. ) ;
#46940 = EDGE_CURVE ( 'NONE', #31213, #15482, #14986, .T. ) ;
#46941 = ORIENTED_EDGE ( 'NONE', *, *, #38950, .F. ) ;
#46942 = AXIS2_PLACEMENT_3D ( 'NONE', #26602, #39944, #5583 ) ;
#46943 = FACE_OUTER_BOUND ( 'NONE', #51448, .T. ) ;
#46944 = CARTESIAN_POINT ( 'NONE',  ( -18.35559287531120987, -2.460819163488158878, 7.850490845989765987 ) ) ;
#46945 = LINE ( 'NONE', #42, #53094 ) ;
#46946 = PLANE ( 'NONE',  #19448 ) ;
#46948 = EDGE_CURVE ( 'NONE', #19740, #1987, #48798, .T. ) ;
#46947 = CARTESIAN_POINT ( 'NONE',  ( -20.06177075545399191, 0.000000000000000000, 14.76272000528038220 ) ) ;
#46949 = CARTESIAN_POINT ( 'NONE',  ( -13.49707129784320436, 0.000000000000000000, 7.131368270877496585 ) ) ;
#46950 = VERTEX_POINT ( 'NONE', #22938 ) ;
#46951 = PLANE ( 'NONE',  #11391 ) ;
#46952 = LINE ( 'NONE', #7773, #19606 ) ;
#46953 = ORIENTED_EDGE ( 'NONE', *, *, #14142, .F. ) ;
#46954 = LINE ( 'NONE', #47501, #14107 ) ;
#46955 = VERTEX_POINT ( 'NONE', #1350 ) ;
#46956 = PLANE ( 'NONE',  #8967 ) ;
#46957 = DIRECTION ( 'NONE',  ( -0.005002170337468016433, -0.7660444431189770143, 0.6427681459581293666 ) ) ;
#46958 = ADVANCED_FACE ( 'NONE', ( #36034 ), #49635, .F. ) ;
#46959 = CARTESIAN_POINT ( 'NONE',  ( -14.46888367232926420, 0.000000000000000000, 12.59025272694991315 ) ) ;
#46960 = PLANE ( 'NONE',  #44111 ) ;
#46961 = EDGE_CURVE ( 'NONE', #6604, #36649, #32019, .T. ) ;
#46962 = CARTESIAN_POINT ( 'NONE',  ( -65.88684560494814946, 1.999999999999989120, -3.942473205312013285 ) ) ;
#46963 = VERTEX_POINT ( 'NONE', #27780 ) ;
#46964 = EDGE_LOOP ( 'NONE', ( #39204, #24973 ) ) ;
#46965 = CARTESIAN_POINT ( 'NONE',  ( -69.59775774058348929, -0.6007421665236040154, 7.493101075386322307 ) ) ;
#46966 = LINE ( 'NONE', #37595, #5011 ) ;
#46967 = DIRECTION ( 'NONE',  ( 0.000000000000000000, -1.000000000000000000, 0.000000000000000000 ) ) ;
#46968 = LINE ( 'NONE', #38432, #29564 ) ;
#46969 = EDGE_CURVE ( 'NONE', #43426, #46161, #6203, .T. ) ;
#46970 = LINE ( 'NONE', #39277, #13813 ) ;
#46971 = PLANE ( 'NONE',  #37616 ) ;
#46972 = ORIENTED_EDGE ( 'NONE', *, *, #25933, .F. ) ;
#46973 = FACE_OUTER_BOUND ( 'NONE', #37864, .T. ) ;
#46974 = CARTESIAN_POINT ( 'NONE',  ( -13.49209884813190818, -3.917936722690662954, 1.997107809296931658 ) ) ;
#46975 = PLANE ( 'NONE',  #1530 ) ;
#46976 = ORIENTED_EDGE ( 'NONE', *, *, #48806, .F. ) ;
#46977 = DIRECTION ( 'NONE',  ( 0.5364919789714477361, 0.6444004775717706579, 0.5449076811759711036 ) ) ;
#46978 = LINE ( 'NONE', #8642, #5983 ) ;
#46979 = FACE_OUTER_BOUND ( 'NONE', #38821, .T. ) ;
#46980 = ORIENTED_EDGE ( 'NONE', *, *, #35710, .T. ) ;
#46981 = VECTOR ( 'NONE', #37497, 999.9999999999998863 ) ;
#46982 = FACE_OUTER_BOUND ( 'NONE', #54605, .T. ) ;
#46983 = ORIENTED_EDGE ( 'NONE', *, *, #26749, .F. ) ;
#46984 = ORIENTED_EDGE ( 'NONE', *, *, #47849, .T. ) ;
#46985 = ORIENTED_EDGE ( 'NONE', *, *, #40950, .F. ) ;
#46986 = ORIENTED_EDGE ( 'NONE', *, *, #7457, .F. ) ;
#46987 = CARTESIAN_POINT ( 'NONE',  ( -18.76354595665420177, -0.1191753592594177458, 14.21882498613976331 ) ) ;
#46989 = EDGE_CURVE ( 'NONE', #38231, #7720, #28044, .T. ) ;
#46988 = ORIENTED_EDGE ( 'NONE', *, *, #22344, .F. ) ;
#46990 = DIRECTION ( 'NONE',  ( -0.7660212471507179544, -0.6427876096865405842, -0.005961354470445141482 ) ) ;
#46991 = VERTEX_POINT ( 'NONE', #41640 ) ;
#46992 = PLANE ( 'NONE',  #7770 ) ;
#46993 = ORIENTED_EDGE ( 'NONE', *, *, #34585, .T. ) ;
#46994 = EDGE_CURVE ( 'NONE', #33913, #36677, #7565, .T. ) ;
#46995 = ORIENTED_EDGE ( 'NONE', *, *, #54831, .F. ) ;
#46996 = CARTESIAN_POINT ( 'NONE',  ( -12.60458797795435615, 0.000000000000000000, 11.86609696750642229 ) ) ;
#46997 = DIRECTION ( 'NONE',  ( 0.5364919789714477361, 0.6444004775717706579, 0.5449076811759711036 ) ) ;
#46998 = ADVANCED_FACE ( 'NONE', ( #3860 ), #29742, .F. ) ;
#46999 = CARTESIAN_POINT ( 'NONE',  ( -24.26908309836554878, 0.000000000000000000, 6.108867788427308376 ) ) ;
#47000 = DIRECTION ( 'NONE',  ( 0.5449076811759707706, 0.6444004775717708799, -0.5364919789714476250 ) ) ;
#47001 = CARTESIAN_POINT ( 'NONE',  ( -17.20841836556132876, 0.000000000000000000, 6.363821570217892187 ) ) ;
#47002 = ORIENTED_EDGE ( 'NONE', *, *, #28155, .T. ) ;
#47003 = ADVANCED_FACE ( 'NONE', ( #12417 ), #24593, .T. ) ;
#47004 = ADVANCED_FACE ( 'NONE', ( #20344 ), #55265, .F. ) ;
#47005 = ADVANCED_FACE ( 'NONE', ( #47039 ), #8139, .F. ) ;
#47006 = ORIENTED_EDGE ( 'NONE', *, *, #46840, .F. ) ;
#47007 = LINE ( 'NONE', #11786, #48521 ) ;
#47008 = PLANE ( 'NONE',  #26692 ) ;
#47009 = CARTESIAN_POINT ( 'NONE',  ( -19.94981257973373090, -1.391042808123044372, 6.283224763914724953 ) ) ;
#47010 = LINE ( 'NONE', #42183, #28521 ) ;
#47011 = DIRECTION ( 'NONE',  ( 0.9999697198139515519, 0.000000000000000000, 0.007781995580013368816 ) ) ;
#47012 = LINE ( 'NONE', #51272, #35919 ) ;
#47013 = EDGE_LOOP ( 'NONE', ( #21647, #39092, #52286, #20503 ) ) ;
#47014 = LINE ( 'NONE', #47863, #33792 ) ;
#47015 = DIRECTION ( 'NONE',  ( 0.000000000000000000, -1.000000000000000000, 0.000000000000000000 ) ) ;
#47016 = ORIENTED_EDGE ( 'NONE', *, *, #42107, .F. ) ;
#47017 = AXIS2_PLACEMENT_3D ( 'NONE', #22452, #52526, #39760 ) ;
#47018 = CARTESIAN_POINT ( 'NONE',  ( -15.60102546347950536, 0.000000000000000000, 12.95077420755565356 ) ) ;
#47019 = FACE_OUTER_BOUND ( 'NONE', #36985, .T. ) ;
#47020 = LINE ( 'NONE', #52595, #33612 ) ;
#47021 = EDGE_CURVE ( 'NONE', #33592, #22613, #3589, .T. ) ;
#47022 = DIRECTION ( 'NONE',  ( 0.000000000000000000, -1.000000000000000000, 0.000000000000000000 ) ) ;
#47023 = LINE ( 'NONE', #50715, #46783 ) ;
#47024 = EDGE_CURVE ( 'NONE', #54767, #42084, #12101, .T. ) ;
#47025 = ORIENTED_EDGE ( 'NONE', *, *, #2626, .F. ) ;
#47026 = EDGE_LOOP ( 'NONE', ( #47976, #18547, #15847, #3057 ) ) ;
#47027 = EDGE_CURVE ( 'NONE', #36758, #12750, #50728, .T. ) ;
#47028 = LINE ( 'NONE', #25435, #50249 ) ;
#47029 = LINE ( 'NONE', #20041, #30430 ) ;
#47030 = CARTESIAN_POINT ( 'NONE',  ( -10.94028622754223967, 0.000000000000000000, 11.14038480894692995 ) ) ;
#47031 = EDGE_CURVE ( 'NONE', #22170, #17803, #11820, .T. ) ;
#47032 = LINE ( 'NONE', #47589, #22814 ) ;
#47033 = LINE ( 'NONE', #55259, #39417 ) ;
#47034 = CARTESIAN_POINT ( 'NONE',  ( -9.110551994824897193, -1.000000000000000000, 3.538847790438064411 ) ) ;
#47035 = PLANE ( 'NONE',  #13888 ) ;
#47036 = EDGE_CURVE ( 'NONE', #28250, #34243, #20050, .T. ) ;
#47037 = CARTESIAN_POINT ( 'NONE',  ( -14.00280974873554030, 0.000000000000000000, 12.40921378708904044 ) ) ;
#47038 = CARTESIAN_POINT ( 'NONE',  ( -67.08542992444135677, -8.381013491352103273, 2.158836163547856124 ) ) ;
#47039 = FACE_OUTER_BOUND ( 'NONE', #44031, .T. ) ;
#47040 = ORIENTED_EDGE ( 'NONE', *, *, #20051, .F. ) ;
#47041 = DIRECTION ( 'NONE',  ( 0.9999697198139515519, 0.000000000000000000, 0.007781995580013368816 ) ) ;
#47042 = ORIENTED_EDGE ( 'NONE', *, *, #23561, .F. ) ;
#47043 = EDGE_LOOP ( 'NONE', ( #29969, #37516, #4515, #3267 ) ) ;
#47044 = ORIENTED_EDGE ( 'NONE', *, *, #25193, .F. ) ;
#47045 = ORIENTED_EDGE ( 'NONE', *, *, #35247, .T. ) ;
#47046 = ORIENTED_EDGE ( 'NONE', *, *, #39732, .T. ) ;
#47047 = ORIENTED_EDGE ( 'NONE', *, *, #45964, .T. ) ;
#47048 = CARTESIAN_POINT ( 'NONE',  ( -18.42808488909577846, -4.727446477803161073, 11.59857078128931995 ) ) ;
#47049 = LINE ( 'NONE', #20356, #51968 ) ;
#47050 = LINE ( 'NONE', #55279, #30320 ) ;
#47051 = VECTOR ( 'NONE', #16860, 999.9999999999998863 ) ;
#47052 = ORIENTED_EDGE ( 'NONE', *, *, #4620, .T. ) ;
#47053 = LINE ( 'NONE', #25464, #53045 ) ;
#47054 = ORIENTED_EDGE ( 'NONE', *, *, #3433, .T. ) ;
#47055 = PLANE ( 'NONE',  #12274 ) ;
#47056 = ORIENTED_EDGE ( 'NONE', *, *, #7920, .F. ) ;
#47057 = CARTESIAN_POINT ( 'NONE',  ( 5.523400220244046643, 0.000000000000000000, 2.340280168031445562 ) ) ;
#47058 = LINE ( 'NONE', #38241, #34619 ) ;
#47059 = CARTESIAN_POINT ( 'NONE',  ( -22.40556560354864146, -0.1191753592594197858, 5.484709000965211523 ) ) ;
#47060 = ORIENTED_EDGE ( 'NONE', *, *, #14690, .F. ) ;
#47061 = CARTESIAN_POINT ( 'NONE',  ( -17.90178974141802470, 0.000000000000000000, 10.05174629191152391 ) ) ;
#47062 = EDGE_LOOP ( 'NONE', ( #29864, #44034, #51749, #52651, #37575 ) ) ;
#47063 = EDGE_CURVE ( 'NONE', #7707, #28385, #42497, .T. ) ;
#47064 = EDGE_CURVE ( 'NONE', #10235, #49289, #29138, .T. ) ;
#47065 = LINE ( 'NONE', #38840, #29132 ) ;
#47066 = DIRECTION ( 'NONE',  ( 0.005961354470445682716, -0.6427876096865404731, -0.7660212471507180654 ) ) ;
#47067 = EDGE_CURVE ( 'NONE', #16632, #36484, #42756, .T. ) ;
#47068 = CARTESIAN_POINT ( 'NONE',  ( -17.06301742894022055, -2.622721114510660367, 3.425498014087459797 ) ) ;
#47069 = CARTESIAN_POINT ( 'NONE',  ( 2.072287782118878319, 0.000000000000000000, -2.950529333540147015 ) ) ;
#47070 = DIRECTION ( 'NONE',  ( 0.005961354470445682716, -0.6427876096865404731, -0.7660212471507180654 ) ) ;
#47071 = CARTESIAN_POINT ( 'NONE',  ( -19.60990026154428278, 0.000000000000000000, 4.498472333781370125 ) ) ;
#47072 = CARTESIAN_POINT ( 'NONE',  ( -8.843397823305778616, 0.000000000000000000, 6.228914038079274462 ) ) ;
#47073 = CARTESIAN_POINT ( 'NONE',  ( -27.99923088623136636, 0.000000000000000000, 7.757173251277078130 ) ) ;
#47074 = ORIENTED_EDGE ( 'NONE', *, *, #35052, .T. ) ;
#47075 = DIRECTION ( 'NONE',  ( -0.9999697198139514409, -0.000000000000000000, -0.007781995580013368816 ) ) ;
#47076 = ORIENTED_EDGE ( 'NONE', *, *, #24842, .F. ) ;
#47077 = DIRECTION ( 'NONE',  ( 0.6427681459581294776, -0.7660444431189769032, 0.005002170337467562802 ) ) ;
#47078 = DIRECTION ( 'NONE',  ( -0.5364919789714478471, 0.6444004775717705469, -0.5449076811759709926 ) ) ;
#47079 = DIRECTION ( 'NONE',  ( 0.7660212471507180654, -0.6427876096865404731, 0.005961354470445141482 ) ) ;
#47080 = LINE ( 'NONE', #50771, #34947 ) ;
#47081 = CARTESIAN_POINT ( 'NONE',  ( -32.65841372305263235, 0.000000000000000000, 9.367568705923016381 ) ) ;
#47082 = EDGE_CURVE ( 'NONE', #17974, #52765, #32841, .T. ) ;
#47083 = CARTESIAN_POINT ( 'NONE',  ( -27.06708303904391144, 0.000000000000000000, 7.395095371555332697 ) ) ;
#47084 = VERTEX_POINT ( 'NONE', #33144 ) ;
#47085 = CARTESIAN_POINT ( 'NONE',  ( -15.31839071495291726, 22.08214803548214533, 3.972478845913684165 ) ) ;
#47086 = CARTESIAN_POINT ( 'NONE',  ( -19.05323196117389628, 5.305366725996514710, 3.913585100488310875 ) ) ;
#47087 = PLANE ( 'NONE',  #22751 ) ;
#47088 = AXIS2_PLACEMENT_3D ( 'NONE', #24714, #20167, #25025 ) ;
#47089 = LINE ( 'NONE', #15864, #17334 ) ;
#47090 = DIRECTION ( 'NONE',  ( -0.000000000000000000, -0.000000000000000000, 1.000000000000000000 ) ) ;
#47091 = EDGE_CURVE ( 'NONE', #54809, #42711, #37684, .T. ) ;
#47092 = DIRECTION ( 'NONE',  ( 0.007781995580012662783, 0.000000000000000000, -0.9999697198139514409 ) ) ;
#47093 = FACE_OUTER_BOUND ( 'NONE', #46412, .T. ) ;
#47094 = ORIENTED_EDGE ( 'NONE', *, *, #22336, .T. ) ;
#47095 = DIRECTION ( 'NONE',  ( 0.5364919789714477361, 0.6444004775717706579, 0.5449076811759711036 ) ) ;
#47096 = LINE ( 'NONE', #8200, #25091 ) ;
#47097 = ORIENTED_EDGE ( 'NONE', *, *, #53423, .F. ) ;
#47098 = EDGE_CURVE ( 'NONE', #7373, #23301, #37375, .T. ) ;
#47099 = ORIENTED_EDGE ( 'NONE', *, *, #13750, .T. ) ;
#47100 = DIRECTION ( 'NONE',  ( -0.7660212471507179544, -0.6427876096865405842, -0.005961354470445141482 ) ) ;
#47101 = EDGE_CURVE ( 'NONE', #55644, #54555, #8296, .T. ) ;
#47102 = ORIENTED_EDGE ( 'NONE', *, *, #8753, .T. ) ;
#47103 = EDGE_CURVE ( 'NONE', #23572, #16010, #50462, .T. ) ;
#47104 = VERTEX_POINT ( 'NONE', #38812 ) ;
#47105 = VERTEX_POINT ( 'NONE', #43602 ) ;
#47106 = ORIENTED_EDGE ( 'NONE', *, *, #38407, .F. ) ;
#47107 =( BOUNDED_SURFACE ( )  B_SPLINE_SURFACE ( 3, 2, ( 
 ( #22376, #35162, #9284 ),
 ( #44229, #13556, #43385 ),
 ( #30868, #26605, #31148 ),
 ( #48469, #9592, #1031 ) ),
 .UNSPECIFIED., .F., .F., .F. ) 
 B_SPLINE_SURFACE_WITH_KNOTS ( ( 4, 4 ),
 ( 3, 3 ),
 ( 0.5110550755831337888, 0.5110755313919185250 ),
 ( 0.000000000000000000, 1.000000000000000000 ),
 .UNSPECIFIED. ) 
 GEOMETRIC_REPRESENTATION_ITEM ( )  RATIONAL_B_SPLINE_SURFACE ( (
 ( 1.000000000000000000, 0.6915731974592014275, 1.000000000000000000),
 ( 1.000000000000000000, 0.6915635181374664153, 1.000000000000000000),
 ( 1.000000000000000000, 0.6915538386379234126, 1.000000000000000000),
 ( 1.000000000000000000, 0.6915441589605814121, 1.000000000000000000) ) ) 
 REPRESENTATION_ITEM ( '' )  SURFACE ( )  );
#47108 = CARTESIAN_POINT ( 'NONE',  ( -9.345197321036080140, -9.000137384199520696, 0.4116184280635072357 ) ) ;
#47109 = ORIENTED_EDGE ( 'NONE', *, *, #53587, .F. ) ;
#47110 = CARTESIAN_POINT ( 'NONE',  ( -50.99228148001754590, 2.341865487272625668, -5.000000000000000000 ) ) ;
#47111 = LINE ( 'NONE', #51651, #22166 ) ;
#47112 = ORIENTED_EDGE ( 'NONE', *, *, #217, .T. ) ;
#47113 = ORIENTED_EDGE ( 'NONE', *, *, #49105, .F. ) ;
#47114 = PLANE ( 'NONE',  #52023 ) ;
#47115 = DIRECTION ( 'NONE',  ( 0.9999697198139515519, 0.000000000000000000, 0.007781995580013368816 ) ) ;
#47116 = ORIENTED_EDGE ( 'NONE', *, *, #15711, .T. ) ;
#47117 = FACE_OUTER_BOUND ( 'NONE', #53808, .T. ) ;
#47118 = DIRECTION ( 'NONE',  ( -0.5364919789714478471, 0.6444004775717705469, -0.5449076811759709926 ) ) ;
#47119 = ORIENTED_EDGE ( 'NONE', *, *, #38605, .T. ) ;
#47120 = CARTESIAN_POINT ( 'NONE',  ( -17.79170326090322263, 3.200641362704009119, 9.045020623922320979 ) ) ;
#47122 = ORIENTED_EDGE ( 'NONE', *, *, #40140, .T. ) ;
#47121 = EDGE_CURVE ( 'NONE', #34236, #22478, #39074, .T. ) ;
#47123 = DIRECTION ( 'NONE',  ( 0.5364919789714477361, 0.6444004775717706579, 0.5449076811759711036 ) ) ;
#47124 = ADVANCED_FACE ( 'NONE', ( #13782 ), #56124, .F. ) ;
#47125 = EDGE_CURVE ( 'NONE', #36041, #10112, #147, .T. ) ;
#47126 = LINE ( 'NONE', #8820, #48120 ) ;
#47127 = ORIENTED_EDGE ( 'NONE', *, *, #49782, .F. ) ;
#47128 = PLANE ( 'NONE',  #40361 ) ;
#47129 = LINE ( 'NONE', #38626, #36534 ) ;
#47130 = LINE ( 'NONE', #5648, #23944 ) ;
#47131 = LINE ( 'NONE', #8232, #50969 ) ;
#47132 = ORIENTED_EDGE ( 'NONE', *, *, #3192, .T. ) ;
#47133 = CARTESIAN_POINT ( 'NONE',  ( -34.64355613791357769, 0.000000000000000000, 10.23836012842048326 ) ) ;
#47134 = LINE ( 'NONE', #55368, #33268 ) ;
#47135 = LINE ( 'NONE', #30099, #31234 ) ;
#47136 = LINE ( 'NONE', #25554, #15034 ) ;
#47137 = CARTESIAN_POINT ( 'NONE',  ( -14.29926954212191248, -2.622721114510659035, 6.540585794009272647 ) ) ;
#47138 = CARTESIAN_POINT ( 'NONE',  ( -12.06004980474070898, 0.000000000000000000, 1.602570457315059205 ) ) ;
#47139 = ADVANCED_FACE ( 'NONE', ( #44189 ), #38510, .F. ) ;
#47140 = DIRECTION ( 'NONE',  ( -0.005961354470445682716, -0.6427876096865404731, 0.7660212471507180654 ) ) ;
#47141 = ORIENTED_EDGE ( 'NONE', *, *, #54596, .F. ) ;
#47142 = CARTESIAN_POINT ( 'NONE',  ( -10.90768746164348002, 0.000000000000000000, 6.951513398406762079 ) ) ;
#47143 = ORIENTED_EDGE ( 'NONE', *, *, #42322, .F. ) ;
#47144 = DIRECTION ( 'NONE',  ( -0.005961354470445682716, -0.6427876096865404731, 0.7660212471507180654 ) ) ;
#47145 = CARTESIAN_POINT ( 'NONE',  ( -14.01623497886155256, -0.1191753592594197858, 2.226008083469502630 ) ) ;
#47146 = DIRECTION ( 'NONE',  ( -0.005002170337468016433, -0.7660444431189770143, 0.6427681459581293666 ) ) ;
#47147 = FACE_OUTER_BOUND ( 'NONE', #7553, .T. ) ;
#47148 = DIRECTION ( 'NONE',  ( -0.5364919789714478471, 0.6444004775717705469, -0.5449076811759709926 ) ) ;
#47149 = ORIENTED_EDGE ( 'NONE', *, *, #25143, .F. ) ;
#47150 = VECTOR ( 'NONE', #49276, 1000.000000000000227 ) ;
#47151 = ORIENTED_EDGE ( 'NONE', *, *, #51435, .T. ) ;
#47152 = PLANE ( 'NONE',  #20487 ) ;
#47153 = LINE ( 'NONE', #13089, #28639 ) ;
#47154 = ORIENTED_EDGE ( 'NONE', *, *, #4619, .F. ) ;
#47155 = DIRECTION ( 'NONE',  ( 0.9999697198139515519, 0.000000000000000000, 0.007781995580013368816 ) ) ;
#47156 = EDGE_LOOP ( 'NONE', ( #34343, #20858, #48683, #15278, #45470 ) ) ;
#47157 = CARTESIAN_POINT ( 'NONE',  ( -10.29290469531352592, -0.1166911823299086465, 0.7797401565107704435 ) ) ;
#47158 = ADVANCED_FACE ( 'NONE', ( #8407 ), #17211, .F. ) ;
#47159 = ORIENTED_EDGE ( 'NONE', *, *, #30, .T. ) ;
#47160 = CARTESIAN_POINT ( 'NONE',  ( -16.28201862538443834, 0.000000000000000000, 6.740363097011673688 ) ) ;
#47161 = VERTEX_POINT ( 'NONE', #39357 ) ;
#47162 = EDGE_LOOP ( 'NONE', ( #38705, #48800, #54825, #27872 ) ) ;
#47163 = EDGE_LOOP ( 'NONE', ( #49902, #54290, #9902, #18203 ) ) ;
#47164 = CARTESIAN_POINT ( 'NONE',  ( -58.00000000000000711, -9.333333333333333925, 3.692809041582076013 ) ) ;
#47165 = DIRECTION ( 'NONE',  ( 0.000000000000000000, -0.000000000000000000, -1.000000000000000000 ) ) ;
#47166 = PLANE ( 'NONE',  #2165 ) ;
#47167 = ADVANCED_FACE ( 'NONE', ( #52134 ), #31107, .F. ) ;
#47168 = LINE ( 'NONE', #12818, #18493 ) ;
#47169 = ORIENTED_EDGE ( 'NONE', *, *, #43381, .F. ) ;
#47170 = ORIENTED_EDGE ( 'NONE', *, *, #52635, .F. ) ;
#47171 = EDGE_CURVE ( 'NONE', #12432, #47173, #4712, .T. ) ;
#47172 = EDGE_CURVE ( 'NONE', #40878, #3654, #26290, .T. ) ;
#47173 = VERTEX_POINT ( 'NONE', #47300 ) ;
#47174 = CARTESIAN_POINT ( 'NONE',  ( -20.43500284407263834, 4.657758921906509642, 12.46314610441118198 ) ) ;
#47175 = DIRECTION ( 'NONE',  ( 0.5449076811759707706, 0.6444004775717708799, -0.5364919789714476250 ) ) ;
#47176 = EDGE_LOOP ( 'NONE', ( #13642, #18063, #5438, #49821, #43359 ) ) ;
#47177 = DIRECTION ( 'NONE',  ( 0.000000000000000000, -1.000000000000000000, 0.000000000000000000 ) ) ;
#47178 = ADVANCED_FACE ( 'NONE', ( #22031 ), #13251, .F. ) ;
#47179 = EDGE_LOOP ( 'NONE', ( #34936, #42566, #24452, #40323 ) ) ;
#47180 = FACE_OUTER_BOUND ( 'NONE', #12965, .T. ) ;
#47181 = LINE ( 'NONE', #8879, #43954 ) ;
#47182 = ORIENTED_EDGE ( 'NONE', *, *, #32819, .F. ) ;
#47183 = ADVANCED_FACE ( 'NONE', ( #21759 ), #51581, .F. ) ;
#47184 = DIRECTION ( 'NONE',  ( -0.005002170337468016433, -0.7660444431189770143, 0.6427681459581293666 ) ) ;
#47185 = ORIENTED_EDGE ( 'NONE', *, *, #36561, .F. ) ;
#47186 = EDGE_CURVE ( 'NONE', #52765, #46212, #17483, .T. ) ;
#47187 = CIRCLE ( 'NONE', #16375, 2.125000000000000000 ) ;
#47188 = DIRECTION ( 'NONE',  ( 0.5449076811759707706, 0.6444004775717708799, -0.5364919789714476250 ) ) ;
#47189 = DIRECTION ( 'NONE',  ( 0.005002170337468016433, -0.7660444431189770143, -0.6427681459581293666 ) ) ;
#47190 = VERTEX_POINT ( 'NONE', #48137 ) ;
#47191 = CARTESIAN_POINT ( 'NONE',  ( -15.44334144360980865, -0.1191753592594183703, 5.538890639235001245 ) ) ;
#47192 = DIRECTION ( 'NONE',  ( -0.9999697198139514409, -0.000000000000000000, -0.007781995580013368816 ) ) ;
#47193 = DIRECTION ( 'NONE',  ( -0.5364919789714478471, 0.6444004775717705469, -0.5449076811759709926 ) ) ;
#47194 = LINE ( 'NONE', #13132, #44573 ) ;
#47195 = ORIENTED_EDGE ( 'NONE', *, *, #26354, .T. ) ;
#47196 = ADVANCED_FACE ( 'NONE', ( #738 ), #25736, .F. ) ;
#47197 = CARTESIAN_POINT ( 'NONE',  ( -19.60912206198628027, -0.1191753592594197858, 4.398475361799976113 ) ) ;
#47198 = CARTESIAN_POINT ( 'NONE',  ( -17.26532721389163072, 0.000000000000000000, 13.67648636611514590 ) ) ;
#47199 = LINE ( 'NONE', #34176, #20450 ) ;
#47200 = CARTESIAN_POINT ( 'NONE',  ( -11.22056963685719211, 0.000000000000000000, 1.239771416285661010 ) ) ;
#47201 = DIRECTION ( 'NONE',  ( -0.6427681459581293666, -0.7660444431189770143, -0.005002170337467561935 ) ) ;
#47202 = EDGE_CURVE ( 'NONE', #41560, #35868, #9547, .T. ) ;
#47203 = DIRECTION ( 'NONE',  ( 0.007781995580012662783, 0.000000000000000000, -0.9999697198139514409 ) ) ;
#47204 = ORIENTED_EDGE ( 'NONE', *, *, #4221, .F. ) ;
#47205 = LINE ( 'NONE', #34436, #10783 ) ;
#47206 = CARTESIAN_POINT ( 'NONE',  ( -17.74404816805336793, 0.000000000000000000, 3.574322630375089460 ) ) ;
#47207 = PLANE ( 'NONE',  #1441 ) ;
#47208 = ORIENTED_EDGE ( 'NONE', *, *, #27592, .T. ) ;
#47209 = CARTESIAN_POINT ( 'NONE',  ( -16.27339646486858982, 0.000000000000000000, 5.632433987238382400 ) ) ;
#47210 = PLANE ( 'NONE',  #12314 ) ;
#47211 = ORIENTED_EDGE ( 'NONE', *, *, #9110, .F. ) ;
#47212 = DIRECTION ( 'NONE',  ( -0.1139275668495183524, 0.9934890585767659488, 4.694855797473114533E-16 ) ) ;
#47213 = DIRECTION ( 'NONE',  ( -0.5449076811759708816, 0.6444004775717707689, 0.5364919789714475140 ) ) ;
#47214 = AXIS2_PLACEMENT_3D ( 'NONE', #8874, #26179, #4585 ) ;
#47215 = DIRECTION ( 'NONE',  ( 0.007781995580012663651, 0.000000000000000000, -0.9999697198139515519 ) ) ;
#47216 = CARTESIAN_POINT ( 'NONE',  ( -67.39666695391619555, 0.1330242493074720589, 1.387855868234969092 ) ) ;
#47217 = ORIENTED_EDGE ( 'NONE', *, *, #48870, .T. ) ;
#47218 = VERTEX_POINT ( 'NONE', #47601 ) ;
#47219 = LINE ( 'NONE', #30193, #14032 ) ;
#47220 = CARTESIAN_POINT ( 'NONE',  ( -24.66083255426108423, 18.30077902615464680, 4.553899851047459535 ) ) ;
#47221 = CARTESIAN_POINT ( 'NONE',  ( -15.40103151951671734, 0.000000000000000000, 12.95233060667165681 ) ) ;
#47222 = CARTESIAN_POINT ( 'NONE',  ( -18.76354595665420177, -0.1191753592594177458, 14.21882498613976331 ) ) ;
#47223 = LINE ( 'NONE', #52051, #19235 ) ;
#47224 = VECTOR ( 'NONE', #46270, 1000.000000000000114 ) ;
#47225 = CARTESIAN_POINT ( 'NONE',  ( -18.86354292863559579, 0.000000000000000000, 14.21804678658176080 ) ) ;
#47226 = ADVANCED_FACE ( 'NONE', ( #5293 ), #55841, .F. ) ;
#47227 = ORIENTED_EDGE ( 'NONE', *, *, #50792, .T. ) ;
#47228 = CARTESIAN_POINT ( 'NONE',  ( 2.072287782118878319, 0.000000000000000000, -2.950529333540147015 ) ) ;
#47229 = VECTOR ( 'NONE', #16412, 1000.000000000000227 ) ;
#47230 = CARTESIAN_POINT ( 'NONE',  ( -19.07690576783079806, 0.000000000000000000, 7.626602792214121962 ) ) ;
#47231 = ORIENTED_EDGE ( 'NONE', *, *, #34918, .T. ) ;
#47232 = DIRECTION ( 'NONE',  ( 0.005002170337468016433, -0.7660444431189770143, -0.6427681459581293666 ) ) ;
#47233 = CARTESIAN_POINT ( 'NONE',  ( -15.33969221856512988, 0.000000000000000000, 5.070362163553848056 ) ) ;
#47234 = CARTESIAN_POINT ( 'NONE',  ( 0.000000000000000000, 0.000000000000000000, 0.000000000000000000 ) ) ;
#47235 = EDGE_CURVE ( 'NONE', #55625, #9472, #14374, .T. ) ;
#47236 = ORIENTED_EDGE ( 'NONE', *, *, #35979, .T. ) ;
#47237 = CARTESIAN_POINT ( 'NONE',  ( -18.53018086135774212, -3.756034771668160577, 10.04397622040690408 ) ) ;
#47238 = ORIENTED_EDGE ( 'NONE', *, *, #23798, .T. ) ;
#47239 = EDGE_CURVE ( 'NONE', #30300, #30276, #45295, .T. ) ;
#47240 = ORIENTED_EDGE ( 'NONE', *, *, #31766, .F. ) ;
#47241 = ORIENTED_EDGE ( 'NONE', *, *, #34968, .F. ) ;
#47242 = ORIENTED_EDGE ( 'NONE', *, *, #15461, .F. ) ;
#47243 = DIRECTION ( 'NONE',  ( -0.005961354470445682716, -0.6427876096865404731, 0.7660212471507180654 ) ) ;
#47244 = ORIENTED_EDGE ( 'NONE', *, *, #56147, .F. ) ;
#47245 = DIRECTION ( 'NONE',  ( -0.7660212471507179544, -0.6427876096865405842, -0.005961354470445141482 ) ) ;
#47246 = VECTOR ( 'NONE', #5407, 999.9999999999998863 ) ;
#47247 = AXIS2_PLACEMENT_3D ( 'NONE', #21897, #22188, #30972 ) ;
#47248 = EDGE_LOOP ( 'NONE', ( #27124, #14996, #46086, #28978 ) ) ;
#47249 = CARTESIAN_POINT ( 'NONE',  ( -10.40281381572843244, 0.000000000000000000, 1.784793464566069687 ) ) ;
#47250 = EDGE_CURVE ( 'NONE', #37328, #35631, #49570, .T. ) ;
#47251 = ORIENTED_EDGE ( 'NONE', *, *, #10157, .T. ) ;
#47252 = DIRECTION ( 'NONE',  ( 0.007781995580012663651, 0.000000000000000000, -0.9999697198139515519 ) ) ;
#47253 = ORIENTED_EDGE ( 'NONE', *, *, #3582, .F. ) ;
#47254 = ADVANCED_FACE ( 'NONE', ( #1829 ), #39912, .F. ) ;
#47255 = CARTESIAN_POINT ( 'NONE',  ( -15.81450767503806532, 0.000000000000000000, 6.374669305521920570 ) ) ;
#47256 = LINE ( 'NONE', #46711, #43024 ) ;
#47257 = CARTESIAN_POINT ( 'NONE',  ( -10.27421835998572064, 0.000000000000000000, 10.96090226820206048 ) ) ;
#47258 = CARTESIAN_POINT ( 'NONE',  ( -15.88130887279446490, 0.000000000000000000, 3.050160814894388839 ) ) ;
#47259 = LINE ( 'NONE', #33103, #53708 ) ;
#47260 = ORIENTED_EDGE ( 'NONE', *, *, #43551, .T. ) ;
#47261 = EDGE_CURVE ( 'NONE', #29343, #22728, #23696, .T. ) ;
#47262 = VERTEX_POINT ( 'NONE', #36787 ) ;
#47263 = LINE ( 'NONE', #47559, #53066 ) ;
#47264 = DIRECTION ( 'NONE',  ( 0.9999697198139515519, 0.000000000000000000, 0.007781995580013368816 ) ) ;
#47265 = UNCERTAINTY_MEASURE_WITH_UNIT (LENGTH_MEASURE( 1.000000000000000082E-05 ), #45508, 'distance_accuracy_value', 'NONE');
#47266 = VECTOR ( 'NONE', #17039, 999.9999999999998863 ) ;
#47267 = CARTESIAN_POINT ( 'NONE',  ( -19.26983395039373903, 0.000000000000000000, 6.717111227287613673 ) ) ;
#47268 = EDGE_CURVE ( 'NONE', #39753, #14310, #6143, .T. ) ;
#47269 = FACE_OUTER_BOUND ( 'NONE', #44473, .T. ) ;
#47270 = CARTESIAN_POINT ( 'NONE',  ( -11.30636317915456779, -0.1191753592594197858, 11.32220194836580340 ) ) ;
#47271 = CARTESIAN_POINT ( 'NONE',  ( -13.47982697681151087, 0.000000000000000000, 4.915510051330911345 ) ) ;
#47272 = ORIENTED_EDGE ( 'NONE', *, *, #1104, .F. ) ;
#47273 = DIRECTION ( 'NONE',  ( -0.2426528472758541499, 0.7422098413412800966, -0.6246952433987894571 ) ) ;
#47274 = CARTESIAN_POINT ( 'NONE',  ( -18.19747506107908563, 0.000000000000000000, 14.03856424583689311 ) ) ;
#47275 = ORIENTED_EDGE ( 'NONE', *, *, #13487, .F. ) ;
#47276 = CARTESIAN_POINT ( 'NONE',  ( -26.13493519185646008, 0.000000000000000000, 7.033017491833586377 ) ) ;
#47277 = B_SPLINE_CURVE_WITH_KNOTS ( 'NONE', 3,
 ( #17743, #12055, #55794, #7832 ),
 .UNSPECIFIED., .F., .F.,
 ( 4, 4 ),
 ( 0.000000000000000000, 0.0003538863460371602767 ),
 .UNSPECIFIED. ) ;
#47278 = CARTESIAN_POINT ( 'NONE',  ( -20.54204810873173415, 0.000000000000000000, 4.860550213503115558 ) ) ;
#47279 = DIRECTION ( 'NONE',  ( -0.5449076811759708816, 0.6444004775717707689, 0.5364919789714475140 ) ) ;
#47280 = CARTESIAN_POINT ( 'NONE',  ( -22.40478740399063895, 0.000000000000000000, 5.384712028983816623 ) ) ;
#47281 = EDGE_LOOP ( 'NONE', ( #43209, #9147, #10625, #53772 ) ) ;
#47282 = ORIENTED_EDGE ( 'NONE', *, *, #19870, .T. ) ;
#47283 = CARTESIAN_POINT ( 'NONE',  ( -8.743798853363076162, -0.1191753592594191058, 4.483031819370165927 ) ) ;
#47284 = PLANE ( 'NONE',  #23177 ) ;
#47285 = LINE ( 'NONE', #8397, #29727 ) ;
#47286 = EDGE_CURVE ( 'NONE', #2953, #17094, #41021, .T. ) ;
#47287 = VECTOR ( 'NONE', #14620, 1000.000000000000000 ) ;
#47288 = VECTOR ( 'NONE', #33447, 999.9999999999998863 ) ;
#47289 = DIRECTION ( 'NONE',  ( 0.9999697198139515519, 0.000000000000000000, 0.007781995580013368816 ) ) ;
#47290 = LINE ( 'NONE', #16638, #53896 ) ;
#47291 = ADVANCED_FACE ( 'NONE', ( #10926 ), #23167, .F. ) ;
#47292 = FACE_OUTER_BOUND ( 'NONE', #32259, .T. ) ;
#47293 = CARTESIAN_POINT ( 'NONE',  ( -19.91685214842295437, -2.137015261443159009, 4.549520895431744982 ) ) ;
#47294 = ORIENTED_EDGE ( 'NONE', *, *, #42144, .F. ) ;
#47295 = DIRECTION ( 'NONE',  ( -0.6246952433987894571, 0.7422098413412802076, 0.2426528472758539834 ) ) ;
#47296 = LINE ( 'NONE', #8406, #34174 ) ;
#47297 = ADVANCED_FACE ( 'NONE', ( #45552 ), #32250, .F. ) ;
#47298 = AXIS2_PLACEMENT_3D ( 'NONE', #11460, #28785, #46087 ) ;
#47299 = EDGE_CURVE ( 'NONE', #33755, #14069, #44446, .T. ) ;
#47300 = CARTESIAN_POINT ( 'NONE',  ( -12.29872409866145055, 0.000000000000000000, 6.571355959844968453 ) ) ;
#47301 = ORIENTED_EDGE ( 'NONE', *, *, #21864, .T. ) ;
#47302 = DIRECTION ( 'NONE',  ( -0.7660212471507179544, -0.6427876096865405842, -0.005961354470445141482 ) ) ;
#47303 = EDGE_CURVE ( 'NONE', #37046, #37070, #990, .T. ) ;
#47304 = EDGE_CURVE ( 'NONE', #3167, #33190, #18319, .T. ) ;
#47305 = EDGE_CURVE ( 'NONE', #27291, #34236, #35657, .T. ) ;
#47306 = ORIENTED_EDGE ( 'NONE', *, *, #41760, .F. ) ;
#47307 = ORIENTED_EDGE ( 'NONE', *, *, #6249, .T. ) ;
#47308 = VECTOR ( 'NONE', #51331, 999.9999999999998863 ) ;
#47309 = ORIENTED_EDGE ( 'NONE', *, *, #55163, .T. ) ;
#47310 = ORIENTED_EDGE ( 'NONE', *, *, #34059, .F. ) ;
#47311 = EDGE_LOOP ( 'NONE', ( #47471, #35385, #37846, #47025, #10691 ) ) ;
#47312 = ORIENTED_EDGE ( 'NONE', *, *, #4839, .F. ) ;
#47313 = LINE ( 'NONE', #8420, #47680 ) ;
#47314 = LINE ( 'NONE', #52437, #23838 ) ;
#47315 = LINE ( 'NONE', #26305, #53057 ) ;
#47316 = VERTEX_POINT ( 'NONE', #40763 ) ;
#47317 = CARTESIAN_POINT ( 'NONE',  ( -55.47117325737978888, 6.581829179614757663, -2.749999999999994671 ) ) ;
#47318 = EDGE_CURVE ( 'NONE', #56078, #11098, #52973, .T. ) ;
#47319 = ORIENTED_EDGE ( 'NONE', *, *, #746, .T. ) ;
#47320 = CARTESIAN_POINT ( 'NONE',  ( -16.79925329029790149, 0.000000000000000000, 13.49544742625427496 ) ) ;
#47321 = ORIENTED_EDGE ( 'NONE', *, *, #8648, .F. ) ;
#47322 = EDGE_CURVE ( 'NONE', #41338, #40788, #31416, .T. ) ;
#47323 = LINE ( 'NONE', #478, #7645 ) ;
#47324 = ADVANCED_FACE ( 'NONE', ( #40496 ), #22868, .F. ) ;
#47325 = CARTESIAN_POINT ( 'NONE',  ( -16.81345671998191449, 0.000000000000000000, 3.412238694616132495 ) ) ;
#47326 = PLANE ( 'NONE',  #48604 ) ;
#47327 = ORIENTED_EDGE ( 'NONE', *, *, #12284, .F. ) ;
#47328 = LINE ( 'NONE', #12131, #3811 ) ;
#47329 = EDGE_CURVE ( 'NONE', #563, #27821, #32636, .T. ) ;
#47330 = ORIENTED_EDGE ( 'NONE', *, *, #44388, .T. ) ;
#47331 = VECTOR ( 'NONE', #26485, 999.9999999999998863 ) ;
#47332 = EDGE_CURVE ( 'NONE', #46401, #39009, #25130, .T. ) ;
#47333 = VECTOR ( 'NONE', #3619, 1000.000000000000227 ) ;
#47334 = CARTESIAN_POINT ( 'NONE',  ( -14.92276770555628929, 0.9340140483890027046, 4.210707049457523610 ) ) ;
#47335 = CARTESIAN_POINT ( 'NONE',  ( -17.74404816805336793, 0.000000000000000000, 3.574322630375089460 ) ) ;
#47336 = DIRECTION ( 'NONE',  ( -0.9999697198139514409, -0.000000000000000000, -0.007781995580013368816 ) ) ;
#47337 = AXIS2_PLACEMENT_3D ( 'NONE', #38972, #42946, #38712 ) ;
#47338 = CARTESIAN_POINT ( 'NONE',  ( -2.882214333898595271, 3.377503723539708513, -2.098823647966802319 ) ) ;
#47339 = DIRECTION ( 'NONE',  ( 0.5364919789714477361, 0.6444004775717706579, 0.5449076811759711036 ) ) ;
#47340 = DIRECTION ( 'NONE',  ( 0.9999697198139515519, 0.000000000000000000, 0.007781995580013368816 ) ) ;
#47341 = CARTESIAN_POINT ( 'NONE',  ( -15.88130887279446490, 0.000000000000000000, 3.050160814894388839 ) ) ;
#47342 = CARTESIAN_POINT ( 'NONE',  ( -69.29498278149517887, -11.65405304096510086, -7.815307374640577898 ) ) ;
#47343 = ORIENTED_EDGE ( 'NONE', *, *, #2027, .T. ) ;
#47344 = CARTESIAN_POINT ( 'NONE',  ( -23.66772770479517618, 18.99370688441070953, 4.503109509781816122 ) ) ;
#47345 = ORIENTED_EDGE ( 'NONE', *, *, #40174, .F. ) ;
#47346 = LINE ( 'NONE', #12719, #53739 ) ;
#47347 = CARTESIAN_POINT ( 'NONE',  ( -17.74560456716937296, 0.000000000000000000, 3.774316574337878372 ) ) ;
#47348 = PLANE ( 'NONE',  #28109 ) ;
#47349 = VECTOR ( 'NONE', #18985, 999.9999999999998863 ) ;
#47350 = LINE ( 'NONE', #24944, #22251 ) ;
#47351 = DIRECTION ( 'NONE',  ( 0.000000000000000000, -0.000000000000000000, -1.000000000000000000 ) ) ;
#47352 = DIRECTION ( 'NONE',  ( 0.5449076811759707706, 0.6444004775717708799, -0.5364919789714476250 ) ) ;
#47353 = CARTESIAN_POINT ( 'NONE',  ( -14.06380102061297066, -0.1191753592594185784, 7.396286890827852289 ) ) ;
#47354 = PRODUCT_CONTEXT ( 'NONE', #5743, 'mechanical' ) ;
#47355 = ORIENTED_EDGE ( 'NONE', *, *, #34302, .F. ) ;
#47356 = CARTESIAN_POINT ( 'NONE',  ( -17.34288414376936416, 20.91330620938233409, 4.147373874202379795 ) ) ;
#47357 = CARTESIAN_POINT ( 'NONE',  ( -10.22736869892390743, 0.000000000000000000, 4.940821433706977572 ) ) ;
#47358 = DIRECTION ( 'NONE',  ( -0.6427681459581293666, -0.7660444431189770143, -0.005002170337467561935 ) ) ;
#47359 = CARTESIAN_POINT ( 'NONE',  ( -26.13337879274045505, 0.000000000000000000, 6.833023547870798353 ) ) ;
#47360 = LINE ( 'NONE', #7628, #52982 ) ;
#47361 = VECTOR ( 'NONE', #43522, 999.9999999999998863 ) ;
#47362 = PLANE ( 'NONE',  #10519 ) ;
#47363 = CARTESIAN_POINT ( 'NONE',  ( -12.65264600905801551, -0.1191753592594188005, 5.191276406585294545 ) ) ;
#47364 = EDGE_LOOP ( 'NONE', ( #56162, #44663, #53393, #42070 ) ) ;
#47365 = DIRECTION ( 'NONE',  ( 0.005002170337468016433, -0.7660444431189770143, -0.6427681459581293666 ) ) ;
#47366 = ADVANCED_FACE ( 'NONE', ( #24531 ), #11502, .F. ) ;
#47367 = CARTESIAN_POINT ( 'NONE',  ( -17.74560456716937296, 0.000000000000000000, 3.774316574337878372 ) ) ;
#47368 = ORIENTED_EDGE ( 'NONE', *, *, #12138, .T. ) ;
#47369 = VECTOR ( 'NONE', #55202, 999.9999999999998863 ) ;
#47370 = ORIENTED_EDGE ( 'NONE', *, *, #17869, .F. ) ;
#47371 = DIRECTION ( 'NONE',  ( 0.000000000000000000, -1.000000000000000000, 0.000000000000000000 ) ) ;
#47372 = ADVANCED_FACE ( 'NONE', ( #54936 ), #45849, .F. ) ;
#47373 = EDGE_CURVE ( 'NONE', #34361, #12737, #28824, .T. ) ;
#47374 = VECTOR ( 'NONE', #32384, 1000.000000000000000 ) ;
#47375 = VECTOR ( 'NONE', #4813, 999.9999999999998863 ) ;
#47376 = ORIENTED_EDGE ( 'NONE', *, *, #19241, .F. ) ;
#47377 = ADVANCED_FACE ( 'NONE', ( #19736 ), #3251, .F. ) ;
#47378 = VECTOR ( 'NONE', #21186, 1000.000000000000000 ) ;
#47379 = VERTEX_POINT ( 'NONE', #11199 ) ;
#47380 = EDGE_LOOP ( 'NONE', ( #39747, #50919, #36998, #47690 ) ) ;
#47381 = VECTOR ( 'NONE', #39114, 999.9999999999998863 ) ;
#47382 = ORIENTED_EDGE ( 'NONE', *, *, #35584, .T. ) ;
#47383 = DIRECTION ( 'NONE',  ( -0.9031405107545327215, -0.1035669190568590248, -0.4166666666666675178 ) ) ;
#47384 = ORIENTED_EDGE ( 'NONE', *, *, #36983, .F. ) ;
#47385 = CARTESIAN_POINT ( 'NONE',  ( -23.23471500290295921, 19.24370688441070953, -4.657437592157546824 ) ) ;
#47386 = FACE_OUTER_BOUND ( 'NONE', #12860, .T. ) ;
#47387 = ORIENTED_EDGE ( 'NONE', *, *, #8575, .F. ) ;
#47388 = VECTOR ( 'NONE', #32804, 1000.000000000000227 ) ;
#47389 = ORIENTED_EDGE ( 'NONE', *, *, #45533, .T. ) ;
#47390 = EDGE_CURVE ( 'NONE', #31490, #17094, #12032, .T. ) ;
#47391 = CARTESIAN_POINT ( 'NONE',  ( -16.33317936670417225, 0.000000000000000000, 13.31440848639340224 ) ) ;
#47392 = ORIENTED_EDGE ( 'NONE', *, *, #54466, .F. ) ;
#47393 = EDGE_CURVE ( 'NONE', #38849, #11370, #33909, .T. ) ;
#47394 = CARTESIAN_POINT ( 'NONE',  ( -20.54126990917373519, -0.1191753592594197858, 4.760553241521720658 ) ) ;
#47395 = DIRECTION ( 'NONE',  ( 0.6427681459581294776, -0.7660444431189769032, 0.005002170337467562802 ) ) ;
#47396 = ORIENTED_EDGE ( 'NONE', *, *, #38145, .T. ) ;
#47397 = CARTESIAN_POINT ( 'NONE',  ( -17.10590788104098792, -4.889348428825664783, 3.369840843825817167 ) ) ;
#47398 = ORIENTED_EDGE ( 'NONE', *, *, #47560, .T. ) ;
#47399 = ADVANCED_FACE ( 'NONE', ( #51229 ), #49622, .T. ) ;
#47400 = DIRECTION ( 'NONE',  ( 0.5449076811759707706, 0.6444004775717708799, -0.5364919789714476250 ) ) ;
#47401 = VECTOR ( 'NONE', #52804, 1000.000000000000227 ) ;
#47402 = EDGE_CURVE ( 'NONE', #12998, #11552, #44708, .T. ) ;
#47403 = LINE ( 'NONE', #13057, #2779 ) ;
#47404 = ORIENTED_EDGE ( 'NONE', *, *, #7758, .F. ) ;
#47405 = LINE ( 'NONE', #25004, #26733 ) ;
#47406 = CARTESIAN_POINT ( 'NONE',  ( -16.81267852042391198, -0.1191753592594197858, 3.312241722634738039 ) ) ;
#47407 = DIRECTION ( 'NONE',  ( 0.5449076811759707706, 0.6444004775717708799, -0.5364919789714476250 ) ) ;
#47408 = VECTOR ( 'NONE', #11887, 1000.000000000000227 ) ;
#47409 = DIRECTION ( 'NONE',  ( 0.007781995580012663651, -3.146120232559066537E-19, -0.9999697198139514409 ) ) ;
#47410 = ORIENTED_EDGE ( 'NONE', *, *, #32047, .T. ) ;
#47411 = VECTOR ( 'NONE', #3010, 999.9999999999998863 ) ;
#47412 = VECTOR ( 'NONE', #32297, 999.9999999999998863 ) ;
#47413 = CARTESIAN_POINT ( 'NONE',  ( -19.60834386242827776, 0.000000000000000000, 4.298478389818581213 ) ) ;
#47414 = CARTESIAN_POINT ( 'NONE',  ( -14.93495759592298988, 0.000000000000000000, 12.77129166681078409 ) ) ;
#47415 = DIRECTION ( 'NONE',  ( 0.005002170337468016433, -0.7660444431189770143, -0.6427681459581293666 ) ) ;
#47416 = CARTESIAN_POINT ( 'NONE',  ( -15.06355305166570346, 0.000000000000000000, 3.595182863174795962 ) ) ;
#47417 = CARTESIAN_POINT ( 'NONE',  ( -16.23605725028139091, -4.889348428825661230, 11.01282148875231748 ) ) ;
#47418 = PLANE ( 'NONE',  #11343 ) ;
#47419 = LINE ( 'NONE', #33524, #13427 ) ;
#47420 = VECTOR ( 'NONE', #44954, 1000.000000000000227 ) ;
#47421 = FACE_OUTER_BOUND ( 'NONE', #46577, .T. ) ;
#47422 = PLANE ( 'NONE',  #23194 ) ;
#47423 = VECTOR ( 'NONE', #47500, 1000.000000000000114 ) ;
#47424 = EDGE_LOOP ( 'NONE', ( #38936, #49592, #30462, #36868 ) ) ;
#47425 = PRESENTATION_STYLE_ASSIGNMENT (( #30404 ) ) ;
#47426 = DIRECTION ( 'NONE',  ( 0.5364919789714477361, 0.6444004775717706579, 0.5449076811759711036 ) ) ;
#47427 = ORIENTED_EDGE ( 'NONE', *, *, #34582, .F. ) ;
#47428 = DIRECTION ( 'NONE',  ( 0.5449076811759707706, 0.6444004775717708799, -0.5364919789714476250 ) ) ;
#47429 = FACE_OUTER_BOUND ( 'NONE', #54847, .T. ) ;
#47430 = CARTESIAN_POINT ( 'NONE',  ( -23.29661890453421691, 19.01267837833611551, -4.488312987714206059 ) ) ;
#47431 = VECTOR ( 'NONE', #1386, 999.9999999999998863 ) ;
#47432 = VECTOR ( 'NONE', #33991, 1000.000000000000227 ) ;
#47433 = DIRECTION ( 'NONE',  ( 0.005002170337468016433, -0.7660444431189770143, -0.6427681459581293666 ) ) ;
#47434 = FACE_OUTER_BOUND ( 'NONE', #13257, .T. ) ;
#47435 = ORIENTED_EDGE ( 'NONE', *, *, #53331, .T. ) ;
#47436 = VERTEX_POINT ( 'NONE', #24825 ) ;
#47437 = DIRECTION ( 'NONE',  ( -0.7660212471507179544, -0.6427876096865405842, -0.005961354470445141482 ) ) ;
#47438 = PLANE ( 'NONE',  #8667 ) ;
#47439 = ORIENTED_EDGE ( 'NONE', *, *, #43847, .T. ) ;
#47440 = VECTOR ( 'NONE', #11719, 1000.000000000000114 ) ;
#47441 = DIRECTION ( 'NONE',  ( 0.000000000000000000, -1.000000000000000000, 0.000000000000000000 ) ) ;
#47442 = EDGE_CURVE ( 'NONE', #17725, #12293, #55207, .T. ) ;
#47443 = ORIENTED_EDGE ( 'NONE', *, *, #36075, .T. ) ;
#47444 = LINE ( 'NONE', #8859, #47635 ) ;
#47445 = VECTOR ( 'NONE', #3363, 1000.000000000000114 ) ;
#47446 = ORIENTED_EDGE ( 'NONE', *, *, #44725, .F. ) ;
#47447 = DIRECTION ( 'NONE',  ( -0.5449076811759708816, 0.6444004775717707689, 0.5364919789714475140 ) ) ;
#47448 = ADVANCED_FACE ( 'NONE', ( #28524 ), #24279, .F. ) ;
#47449 = EDGE_CURVE ( 'NONE', #24475, #16658, #17994, .T. ) ;
#47450 = ORIENTED_EDGE ( 'NONE', *, *, #3078, .T. ) ;
#47451 = ORIENTED_EDGE ( 'NONE', *, *, #54482, .T. ) ;
#47452 = VERTEX_POINT ( 'NONE', #25388 ) ;
#47453 = LINE ( 'NONE', #43743, #51999 ) ;
#47454 = AXIS2_PLACEMENT_3D ( 'NONE', #14092, #14633, #10386 ) ;
#47455 = LINE ( 'NONE', #26426, #33217 ) ;
#47456 = DIRECTION ( 'NONE',  ( 0.000000000000000000, -0.000000000000000000, -1.000000000000000000 ) ) ;
#47457 = VECTOR ( 'NONE', #47192, 1000.000000000000227 ) ;
#47458 = AXIS2_PLACEMENT_3D ( 'NONE', #17455, #29410, #22000 ) ;
#47459 = DIRECTION ( 'NONE',  ( 0.000000000000000000, -0.000000000000000000, -1.000000000000000000 ) ) ;
#47460 = ORIENTED_EDGE ( 'NONE', *, *, #56176, .F. ) ;
#47461 = EDGE_LOOP ( 'NONE', ( #7774, #39777, #31890, #7000 ) ) ;
#47462 = VECTOR ( 'NONE', #49127, 1000.000000000000114 ) ;
#47463 = ORIENTED_EDGE ( 'NONE', *, *, #2928, .F. ) ;
#47464 = VECTOR ( 'NONE', #5345, 1000.000000000000000 ) ;
#47465 = DIRECTION ( 'NONE',  ( -0.000000000000000000, -0.000000000000000000, 1.000000000000000000 ) ) ;
#47466 = VERTEX_POINT ( 'NONE', #8929 ) ;
#47467 = FACE_OUTER_BOUND ( 'NONE', #54133, .T. ) ;
#47468 = ORIENTED_EDGE ( 'NONE', *, *, #3007, .F. ) ;
#47469 = DIRECTION ( 'NONE',  ( -0.7660212471507179544, -0.6427876096865405842, -0.005961354470445141482 ) ) ;
#47470 = DIRECTION ( 'NONE',  ( -0.005002170337468016433, -0.7660444431189770143, 0.6427681459581293666 ) ) ;
#47471 = ORIENTED_EDGE ( 'NONE', *, *, #20025, .F. ) ;
#47472 = DIRECTION ( 'NONE',  ( 0.9999697198139515519, 0.000000000000000000, 0.007781995580013368816 ) ) ;
#47473 = ORIENTED_EDGE ( 'NONE', *, *, #54583, .T. ) ;
#47474 = EDGE_CURVE ( 'NONE', #3804, #21256, #8339, .T. ) ;
#47475 = DIRECTION ( 'NONE',  ( 0.007781995580012662783, 0.000000000000000000, -0.9999697198139514409 ) ) ;
#47476 = VECTOR ( 'NONE', #49139, 999.9999999999998863 ) ;
#47478 = ADVANCED_FACE ( 'NONE', ( #38748 ), #43294, .F. ) ;
#47477 = ORIENTED_EDGE ( 'NONE', *, *, #24478, .F. ) ;
#47479 = CARTESIAN_POINT ( 'NONE',  ( 4.452747148193316740, 0.000000000000000000, 0.4159841754879232689 ) ) ;
#47480 = FACE_OUTER_BOUND ( 'NONE', #13991, .T. ) ;
#47481 = CARTESIAN_POINT ( 'NONE',  ( -16.81190032086591302, 0.000000000000000000, 3.212244750653343583 ) ) ;
#47482 = ADVANCED_FACE ( 'NONE', ( #42986 ), #48075, .F. ) ;
#47483 = ORIENTED_EDGE ( 'NONE', *, *, #9979, .F. ) ;
#47484 = VECTOR ( 'NONE', #16982, 1000.000000000000227 ) ;
#47485 = DIRECTION ( 'NONE',  ( 0.5364919789714477361, 0.6444004775717706579, 0.5449076811759711036 ) ) ;
#47486 = LINE ( 'NONE', #17375, #11983 ) ;
#47487 = EDGE_CURVE ( 'NONE', #17816, #25199, #21425, .T. ) ;
#47488 = PLANE ( 'NONE',  #19476 ) ;
#47489 = AXIS2_PLACEMENT_3D ( 'NONE', #6829, #24409, #55630 ) ;
#47490 = CARTESIAN_POINT ( 'NONE',  ( -16.06709938707323460, 0.000000000000000000, 13.13181314741652628 ) ) ;
#47491 = DIRECTION ( 'NONE',  ( 0.000000000000000000, -1.000000000000000000, 0.000000000000000000 ) ) ;
#47492 = DIRECTION ( 'NONE',  ( 0.7660212471507180654, -0.6427876096865404731, 0.005961354470445141482 ) ) ;
#47493 = DIRECTION ( 'NONE',  ( 0.6427681459581294776, -0.7660444431189769032, 0.005002170337467562802 ) ) ;
#47494 = ORIENTED_EDGE ( 'NONE', *, *, #25517, .F. ) ;
#47495 = DIRECTION ( 'NONE',  ( 0.000000000000000000, -1.000000000000000000, 0.000000000000000000 ) ) ;
#47496 = DIRECTION ( 'NONE',  ( 0.000000000000000000, -0.000000000000000000, -1.000000000000000000 ) ) ;
#47497 = DIRECTION ( 'NONE',  ( -0.005002170337468016433, -0.7660444431189770143, 0.6427681459581293666 ) ) ;
#47498 = ORIENTED_EDGE ( 'NONE', *, *, #18651, .F. ) ;
#47499 = AXIS2_PLACEMENT_3D ( 'NONE', #9116, #9966, #43479 ) ;
#47500 = DIRECTION ( 'NONE',  ( 0.5449076811759707706, 0.6444004775717708799, -0.5364919789714476250 ) ) ;
#47501 = CARTESIAN_POINT ( 'NONE',  ( -18.26762043990991202, -2.946525016555662457, 3.883075692263754153 ) ) ;
#47502 = VERTEX_POINT ( 'NONE', #13714 ) ;
#47503 = VECTOR ( 'NONE', #34094, 999.9999999999998863 ) ;
#47504 = CARTESIAN_POINT ( 'NONE',  ( -23.44702061269273230, 18.93456859731804087, -4.495868787147773382 ) ) ;
#47505 = DIRECTION ( 'NONE',  ( -0.6427681459581293666, -0.7660444431189770143, -0.005002170337467561935 ) ) ;
#47506 = ADVANCED_FACE ( 'NONE', ( #21955 ), #52061, .F. ) ;
#47507 = CARTESIAN_POINT ( 'NONE',  ( -15.00169697481098297, -0.1191753592594168437, 8.496984177065126431 ) ) ;
#47508 = CARTESIAN_POINT ( 'NONE',  ( -68.55686626046413323, 0.1328883920391356610, -5.294842188084643908 ) ) ;
#47509 = EDGE_LOOP ( 'NONE', ( #21582, #16859, #907, #4452 ) ) ;
#47510 = VECTOR ( 'NONE', #21266, 999.9999999999998863 ) ;
#47511 = AXIS2_PLACEMENT_3D ( 'NONE', #8977, #26553, #13510 ) ;
#47512 = EDGE_LOOP ( 'NONE', ( #10698, #43003, #9754, #7265 ) ) ;
#47513 = DIRECTION ( 'NONE',  ( 0.000000000000000000, -1.000000000000000000, 0.000000000000000000 ) ) ;
#47514 = FACE_OUTER_BOUND ( 'NONE', #25811, .T. ) ;
#47515 = CARTESIAN_POINT ( 'NONE',  ( -13.45720677381246411, 0.000000000000000000, 2.008862543950673540 ) ) ;
#47516 = ADVANCED_FACE ( 'NONE', ( #42693 ), #34464, .F. ) ;
#47517 = DIRECTION ( 'NONE',  ( -0.005002170337468016433, -0.7660444431189770143, 0.6427681459581293666 ) ) ;
#47518 = DIRECTION ( 'NONE',  ( 0.005961354470445682716, -0.6427876096865404731, -0.7660212471507180654 ) ) ;
#47519 = EDGE_CURVE ( 'NONE', #43608, #11345, #51647, .T. ) ;
#47520 = FACE_OUTER_BOUND ( 'NONE', #21360, .T. ) ;
#47521 = EDGE_LOOP ( 'NONE', ( #13347, #1206, #13077, #31346 ) ) ;
#47522 = CARTESIAN_POINT ( 'NONE',  ( -14.07242318112881740, -0.1191753592594177180, 8.504216000601145353 ) ) ;
#47523 = EDGE_CURVE ( 'NONE', #47613, #50717, #21116, .T. ) ;
#47524 = DIRECTION ( 'NONE',  ( -0.005961354470445682716, -0.6427876096865404731, 0.7660212471507180654 ) ) ;
#47525 = ORIENTED_EDGE ( 'NONE', *, *, #2104, .T. ) ;
#47526 = VECTOR ( 'NONE', #53139, 999.9999999999998863 ) ;
#47527 = DIRECTION ( 'NONE',  ( -0.000000000000000000, -1.000000000000000000, -0.000000000000000000 ) ) ;
#47528 = DIRECTION ( 'NONE',  ( 0.007781995580012663651, 0.000000000000000000, -0.9999697198139515519 ) ) ;
#47529 = VECTOR ( 'NONE', #8111, 1000.000000000000227 ) ;
#47530 = CARTESIAN_POINT ( 'NONE',  ( -16.48488662285251038, 0.000000000000000000, 7.108116401153436570 ) ) ;
#47531 = VERTEX_POINT ( 'NONE', #17716 ) ;
#47532 = PRODUCT_RELATED_PRODUCT_CATEGORY ( 'part', '', ( #27850 ) ) ;
#47533 = FACE_OUTER_BOUND ( 'NONE', #13101, .T. ) ;
#47534 = VECTOR ( 'NONE', #46141, 999.9999999999998863 ) ;
#47535 = ORIENTED_EDGE ( 'NONE', *, *, #30371, .F. ) ;
#47536 = ADVANCED_FACE ( 'NONE', ( #8641 ), #39011, .F. ) ;
#47537 = ORIENTED_EDGE ( 'NONE', *, *, #9788, .T. ) ;
#47538 = ORIENTED_EDGE ( 'NONE', *, *, #15351, .T. ) ;
#47539 = ORIENTED_EDGE ( 'NONE', *, *, #22259, .T. ) ;
#47540 = VECTOR ( 'NONE', #41922, 1000.000000000000114 ) ;
#47541 = LINE ( 'NONE', #43825, #53840 ) ;
#47542 = EDGE_LOOP ( 'NONE', ( #46780, #50014, #34156, #13158 ) ) ;
#47543 = CARTESIAN_POINT ( 'NONE',  ( -13.20612570884338943, 23.30166480535930518, -3.681892822732769410 ) ) ;
#47544 = VECTOR ( 'NONE', #46348, 1000.000000000000227 ) ;
#47545 = ORIENTED_EDGE ( 'NONE', *, *, #36546, .T. ) ;
#47546 = DIRECTION ( 'NONE',  ( 0.6427681459581294776, -0.7660444431189769032, 0.005002170337467562802 ) ) ;
#47547 = ORIENTED_EDGE ( 'NONE', *, *, #6221, .F. ) ;
#47548 = PLANE ( 'NONE',  #49191 ) ;
#47549 = ORIENTED_EDGE ( 'NONE', *, *, #40065, .T. ) ;
#47550 = VECTOR ( 'NONE', #45914, 1000.000000000000227 ) ;
#47551 = AXIS2_PLACEMENT_3D ( 'NONE', #50428, #51260, #37927 ) ;
#47552 = FACE_OUTER_BOUND ( 'NONE', #8262, .T. ) ;
#47553 = DIRECTION ( 'NONE',  ( 0.9999697198139515519, 0.000000000000000000, 0.007781995580013368816 ) ) ;
#47554 = CARTESIAN_POINT ( 'NONE',  ( -11.64544826116150134, 2.553033558614006271, 5.594771718522403070 ) ) ;
#47555 = PLANE ( 'NONE',  #55009 ) ;
#47556 = CARTESIAN_POINT ( 'NONE',  ( -1.602266347997184592, -7.552920495778074894, 3.840748238420124139 ) ) ;
#47557 = ORIENTED_EDGE ( 'NONE', *, *, #13245, .F. ) ;
#47558 = VERTEX_POINT ( 'NONE', #52361 ) ;
#47559 = CARTESIAN_POINT ( 'NONE',  ( -15.58595925418828898, -1.975113310420658852, 2.872420537456616074 ) ) ;
#47560 = EDGE_CURVE ( 'NONE', #14388, #30483, #4384, .T. ) ;
#47561 = LINE ( 'NONE', #43571, #12177 ) ;
#47562 = DIRECTION ( 'NONE',  ( 0.9999697198139515519, 0.000000000000000000, 0.007781995580013368816 ) ) ;
#47563 = VECTOR ( 'NONE', #6420, 999.9999999999998863 ) ;
#47564 = LINE ( 'NONE', #9216, #18697 ) ;
#47565 = VECTOR ( 'NONE', #49696, 1000.000000000000227 ) ;
#47566 = LINE ( 'NONE', #26013, #22222 ) ;
#47567 = DIRECTION ( 'NONE',  ( -0.8531650599175529814, -0.4028455766673920135, 0.3313982828793697877 ) ) ;
#47568 = ORIENTED_EDGE ( 'NONE', *, *, #30414, .F. ) ;
#47569 = DIRECTION ( 'NONE',  ( 0.007781995580012662783, 0.000000000000000000, -0.9999697198139514409 ) ) ;
#47570 = DIRECTION ( 'NONE',  ( -0.5364919789714478471, 0.6444004775717705469, -0.5449076811759709926 ) ) ;
#47571 = AXIS2_PLACEMENT_3D ( 'NONE', #51739, #13139, #34175 ) ;
#47572 = ORIENTED_EDGE ( 'NONE', *, *, #32861, .T. ) ;
#47573 = EDGE_CURVE ( 'NONE', #24462, #1358, #78, .T. ) ;
#47574 = PLANE ( 'NONE',  #12532 ) ;
#47575 = DIRECTION ( 'NONE',  ( -0.5449076811759708816, 0.6444004775717707689, 0.5364919789714475140 ) ) ;
#47576 = CARTESIAN_POINT ( 'NONE',  ( -20.18892918444406348, 0.000000000000000000, 5.401956350015513664 ) ) ;
#47577 = EDGE_CURVE ( 'NONE', #4495, #46324, #43815, .T. ) ;
#47578 = EDGE_CURVE ( 'NONE', #38849, #55928, #3792, .T. ) ;
#47579 = CARTESIAN_POINT ( 'NONE',  ( -1.246832498358330099E-15, 2.000000000000000000, 0.000000000000000000 ) ) ;
#47580 = ORIENTED_EDGE ( 'NONE', *, *, #27250, .F. ) ;
#47581 = AXIS2_PLACEMENT_3D ( 'NONE', #3361, #20679, #37994 ) ;
#47582 = VERTEX_POINT ( 'NONE', #55771 ) ;
#47583 = VECTOR ( 'NONE', #40830, 1000.000000000000227 ) ;
#47584 = LINE ( 'NONE', #29981, #22132 ) ;
#47585 = CARTESIAN_POINT ( 'NONE',  ( -22.36868959911851462, 19.74370688441071309, -4.433759251830043269 ) ) ;
#47586 = LINE ( 'NONE', #3849, #17023 ) ;
#47587 = EDGE_CURVE ( 'NONE', #46034, #33489, #16883, .T. ) ;
#47588 = VECTOR ( 'NONE', #8899, 1000.000000000000114 ) ;
#47589 = CARTESIAN_POINT ( 'NONE',  ( -14.20280369269832832, 0.000000000000000000, 12.40765738797303719 ) ) ;
#47590 = EDGE_CURVE ( 'NONE', #678, #27743, #12616, .T. ) ;
#47591 = LINE ( 'NONE', #25727, #54789 ) ;
#47592 = DIRECTION ( 'NONE',  ( 0.9999697198139515519, 0.000000000000000000, 0.007781995580013368816 ) ) ;
#47593 = FACE_OUTER_BOUND ( 'NONE', #31263, .T. ) ;
#47594 = ADVANCED_FACE ( 'NONE', ( #40417 ), #53210, .F. ) ;
#47595 = ORIENTED_EDGE ( 'NONE', *, *, #10965, .F. ) ;
#47596 = AXIS2_PLACEMENT_3D ( 'NONE', #37305, #2099, #53794 ) ;
#47597 = CARTESIAN_POINT ( 'NONE',  ( -27.06708303904391144, 0.000000000000000000, 7.395095371555332697 ) ) ;
#47598 = VECTOR ( 'NONE', #35345, 999.9999999999998863 ) ;
#47599 = DIRECTION ( 'NONE',  ( -0.005002170337468016433, -0.7660444431189770143, 0.6427681459581293666 ) ) ;
#47600 = ORIENTED_EDGE ( 'NONE', *, *, #37307, .F. ) ;
#47601 = CARTESIAN_POINT ( 'NONE',  ( -11.70325384083886000, -0.1191753592594189115, 2.613340307316962985 ) ) ;
#47602 = ORIENTED_EDGE ( 'NONE', *, *, #27977, .F. ) ;
#47603 = CARTESIAN_POINT ( 'NONE',  ( -8.836332061905933344, 0.000000000000000000, 5.320978872268770310 ) ) ;
#47604 = ADVANCED_FACE ( 'NONE', ( #31335 ), #14845, .F. ) ;
#47605 = EDGE_LOOP ( 'NONE', ( #36695, #41341, #14236, #52411 ) ) ;
#47606 = VERTEX_POINT ( 'NONE', #19371 ) ;
#47607 = VECTOR ( 'NONE', #10208, 999.9999999999998863 ) ;
#47608 = ADVANCED_FACE ( 'NONE', ( #1513 ), #5770, .F. ) ;
#47609 = ORIENTED_EDGE ( 'NONE', *, *, #16202, .T. ) ;
#47610 = ORIENTED_EDGE ( 'NONE', *, *, #9307, .T. ) ;
#47611 = ORIENTED_EDGE ( 'NONE', *, *, #36604, .F. ) ;
#47612 = VECTOR ( 'NONE', #51596, 999.9999999999998863 ) ;
#47613 = VERTEX_POINT ( 'NONE', #927 ) ;
#47614 = DIRECTION ( 'NONE',  ( -0.5449076811759708816, 0.6444004775717707689, 0.5364919789714475140 ) ) ;
#47615 = DIRECTION ( 'NONE',  ( -0.9999697198139514409, -0.000000000000000000, -0.007781995580013368816 ) ) ;
#47616 = DIRECTION ( 'NONE',  ( 0.005002170337468016433, -0.7660444431189770143, -0.6427681459581293666 ) ) ;
#47617 = VECTOR ( 'NONE', #27677, 1000.000000000000227 ) ;
#47618 = ORIENTED_EDGE ( 'NONE', *, *, #38661, .F. ) ;
#47619 = LINE ( 'NONE', #39091, #48538 ) ;
#47620 = VERTEX_POINT ( 'NONE', #23089 ) ;
#47621 = VECTOR ( 'NONE', #30385, 999.9999999999998863 ) ;
#47622 = VERTEX_POINT ( 'NONE', #22539 ) ;
#47623 = VECTOR ( 'NONE', #90, 1000.000000000000000 ) ;
#47624 = VECTOR ( 'NONE', #20237, 1000.000000000000114 ) ;
#47625 = DIRECTION ( 'NONE',  ( 0.000000000000000000, -0.000000000000000000, -1.000000000000000000 ) ) ;
#47626 = AXIS2_PLACEMENT_3D ( 'NONE', #2592, #53446, #54003 ) ;
#47627 = LINE ( 'NONE', #12700, #17812 ) ;
#47628 = VERTEX_POINT ( 'NONE', #53463 ) ;
#47629 = PLANE ( 'NONE',  #36448 ) ;
#47630 = ORIENTED_EDGE ( 'NONE', *, *, #47063, .F. ) ;
#47631 = AXIS2_PLACEMENT_3D ( 'NONE', #26334, #26617, #39704 ) ;
#47632 = DIRECTION ( 'NONE',  ( 0.5449076811759707706, 0.6444004775717708799, -0.5364919789714476250 ) ) ;
#47633 = EDGE_CURVE ( 'NONE', #9930, #49888, #36706, .T. ) ;
#47634 = CARTESIAN_POINT ( 'NONE',  ( -12.85804337256432639, 5.143464774974015441, 1.512328983069690214 ) ) ;
#47635 = VECTOR ( 'NONE', #21627, 1000.000000000000114 ) ;
#47636 = CARTESIAN_POINT ( 'NONE',  ( -1.086233639165236964, 0.000000000000000000, -2.796443541562362078 ) ) ;
#47637 = VECTOR ( 'NONE', #35293, 999.9999999999998863 ) ;
#47638 = CARTESIAN_POINT ( 'NONE',  ( -18.86354292863559579, 0.000000000000000000, 14.21804678658176080 ) ) ;
#47639 = CARTESIAN_POINT ( 'NONE',  ( -17.26532721389163072, 0.000000000000000000, 13.67648636611514590 ) ) ;
#47640 = CARTESIAN_POINT ( 'NONE',  ( -17.46532115785441519, 0.000000000000000000, 13.67492996699914265 ) ) ;
#47641 = CARTESIAN_POINT ( 'NONE',  ( -16.38123739780782984, -0.1191753592594194527, 6.639587925472277163 ) ) ;
#47642 = CARTESIAN_POINT ( 'NONE',  ( -20.38395485794165651, 5.143464774974010112, 13.24044338485239081 ) ) ;
#47643 = ORIENTED_EDGE ( 'NONE', *, *, #12734, .F. ) ;
#47644 = DIRECTION ( 'NONE',  ( -0.5449076811759708816, 0.6444004775717707689, 0.5364919789714475140 ) ) ;
#47645 = ADVANCED_FACE ( 'NONE', ( #19087 ), #5227, .F. ) ;
#47646 = EDGE_CURVE ( 'NONE', #5305, #39923, #10024, .T. ) ;
#47647 = CARTESIAN_POINT ( 'NONE',  ( -23.33693525117809386, 0.000000000000000000, 5.746789908705562944 ) ) ;
#47648 = PLANE ( 'NONE',  #32354 ) ;
#47649 = DIRECTION ( 'NONE',  ( -0.005002170337468016433, -0.7660444431189770143, 0.6427681459581293666 ) ) ;
#47650 = FACE_OUTER_BOUND ( 'NONE', #1242, .T. ) ;
#47651 = CARTESIAN_POINT ( 'NONE',  ( -19.05966144679910457, 0.000000000000000000, 5.410744572667534946 ) ) ;
#47652 = EDGE_CURVE ( 'NONE', #46401, #35539, #6330, .T. ) ;
#47653 = PLANE ( 'NONE',  #24131 ) ;
#47654 = VECTOR ( 'NONE', #15793, 1000.000000000000227 ) ;
#47655 = FACE_OUTER_BOUND ( 'NONE', #43358, .T. ) ;
#47656 = PRODUCT_CONTEXT ( 'NONE', #1749, 'mechanical' ) ;
#47657 = AXIS2_PLACEMENT_3D ( 'NONE', #24844, #42163, #34479 ) ;
#47658 = ORIENTED_EDGE ( 'NONE', *, *, #39784, .F. ) ;
#47659 = CARTESIAN_POINT ( 'NONE',  ( -17.74482636761137044, -0.1191753592594197858, 3.674319602356483916 ) ) ;
#47660 = CARTESIAN_POINT ( 'NONE',  ( -14.66887761629205222, 0.000000000000000000, 12.58869632783390990 ) ) ;
#47661 = PLANE ( 'NONE',  #10956 ) ;
#47662 = VECTOR ( 'NONE', #34441, 1000.000000000000114 ) ;
#47663 = DIRECTION ( 'NONE',  ( 0.5449076811759707706, 0.6444004775717708799, -0.5364919789714476250 ) ) ;
#47664 = ADVANCED_FACE ( 'NONE', ( #18843 ), #49494, .F. ) ;
#47665 = VECTOR ( 'NONE', #52457, 999.9999999999998863 ) ;
#47666 = CARTESIAN_POINT ( 'NONE',  ( -56.00000000000000711, 3.800000000000001599, -1.887458608817680794 ) ) ;
#47667 = CARTESIAN_POINT ( 'NONE',  ( -15.96710241509184058, -0.1191753592594218814, 13.13259134697452879 ) ) ;
#47668 = CARTESIAN_POINT ( 'NONE',  ( -15.08235377181340198, 0.000000000000000000, 6.011035026684171889 ) ) ;
#47669 = EDGE_CURVE ( 'NONE', #45628, #26746, #35888, .T. ) ;
#47670 = PLANE ( 'NONE',  #43058 ) ;
#47671 = VECTOR ( 'NONE', #47472, 999.9999999999998863 ) ;
#47672 = CARTESIAN_POINT ( 'NONE',  ( -27.99845268667336384, -0.1191753592594197858, 7.657176279295684118 ) ) ;
#47673 = VECTOR ( 'NONE', #6402, 1000.000000000000114 ) ;
#47674 = ADVANCED_FACE ( 'NONE', ( #18250 ), #45227, .F. ) ;
#47675 = VERTEX_POINT ( 'NONE', #23380 ) ;
#47676 = CARTESIAN_POINT ( 'NONE',  ( -19.26827755127773401, 0.000000000000000000, 6.517117283324824761 ) ) ;
#47677 = VECTOR ( 'NONE', #3063, 1000.000000000000227 ) ;
#47678 = ADVANCED_FACE ( 'NONE', ( #23630 ), #40947, .T. ) ;
#47679 = ORIENTED_EDGE ( 'NONE', *, *, #44720, .T. ) ;
#47680 = VECTOR ( 'NONE', #52148, 999.9999999999998863 ) ;
#47681 = AXIS2_PLACEMENT_3D ( 'NONE', #24388, #50782, #24127 ) ;
#47682 = AXIS2_PLACEMENT_3D ( 'NONE', #31336, #31621, #44383 ) ;
#47683 = ORIENTED_EDGE ( 'NONE', *, *, #3652, .F. ) ;
#47684 = AXIS2_PLACEMENT_3D ( 'NONE', #52334, #3765, #13437 ) ;
#47685 = ORIENTED_EDGE ( 'NONE', *, *, #34652, .F. ) ;
#47686 = ORIENTED_EDGE ( 'NONE', *, *, #31577, .F. ) ;
#47687 = ORIENTED_EDGE ( 'NONE', *, *, #319, .T. ) ;
#47688 = DIRECTION ( 'NONE',  ( 0.007781995580012663651, -3.146120232559066537E-19, -0.9999697198139514409 ) ) ;
#47689 = CARTESIAN_POINT ( 'NONE',  ( -20.54126990917373519, -0.1191753592594197858, 4.760553241521720658 ) ) ;
#47690 = ORIENTED_EDGE ( 'NONE', *, *, #9239, .F. ) ;
#47691 = AXIS2_PLACEMENT_3D ( 'NONE', #9756, #40685, #40400 ) ;
#47692 = CARTESIAN_POINT ( 'NONE',  ( -65.82994354660264946, -3.295974604355934110E-14, -2.610734445418879002 ) ) ;
#47693 = ORIENTED_EDGE ( 'NONE', *, *, #48849, .F. ) ;
#47694 = CARTESIAN_POINT ( 'NONE',  ( -9.088448639303150500, -8.751434906964478344, 0.3118885208565043698 ) ) ;
#47695 = CARTESIAN_POINT ( 'NONE',  ( -11.59828696140490223, 0.000000000000000000, 1.975496072340833242 ) ) ;
#47696 = ORIENTED_EDGE ( 'NONE', *, *, #33278, .F. ) ;
#47697 = VECTOR ( 'NONE', #8117, 1000.000000000000227 ) ;
#47698 = FACE_OUTER_BOUND ( 'NONE', #2145, .T. ) ;
#47699 = EDGE_CURVE ( 'NONE', #5535, #30132, #40696, .T. ) ;
#47700 = ORIENTED_EDGE ( 'NONE', *, *, #19930, .T. ) ;
#47701 = LINE ( 'NONE', #35756, #54494 ) ;
#47702 = VECTOR ( 'NONE', #23601, 1000.000000000000227 ) ;
#47703 = ADVANCED_FACE ( 'NONE', ( #52898 ), #9766, .F. ) ;
#47704 = CARTESIAN_POINT ( 'NONE',  ( -14.62059092847759878, 0.000000000000000000, 6.383960641709946593 ) ) ;
#47705 = AXIS2_PLACEMENT_3D ( 'NONE', #22985, #27828, #1099 ) ;
#47706 = VECTOR ( 'NONE', #52638, 999.9999999999998863 ) ;
#47707 = EDGE_LOOP ( 'NONE', ( #20717, #53058, #8858, #51857 ) ) ;
#47708 = CARTESIAN_POINT ( 'NONE',  ( -27.99845268667336384, -0.1191753592594197858, 7.657176279295684118 ) ) ;
#47709 = CARTESIAN_POINT ( 'NONE',  ( -9.342070512798265725, 0.000000000000000000, 10.59882438848031505 ) ) ;
#47710 = DIRECTION ( 'NONE',  ( -0.5449076811759708816, 0.6444004775717707689, 0.5364919789714475140 ) ) ;
#47711 = EDGE_CURVE ( 'NONE', #18282, #31194, #48929, .T. ) ;
#47712 = LINE ( 'NONE', #42866, #33751 ) ;
#47713 = ORIENTED_EDGE ( 'NONE', *, *, #36436, .F. ) ;
#47714 = EDGE_CURVE ( 'NONE', #1256, #36728, #41526, .T. ) ;
#47715 = VECTOR ( 'NONE', #6378, 999.9999999999998863 ) ;
#47716 = ADVANCED_FACE ( 'NONE', ( #45766 ), #33550, .F. ) ;
#47717 = EDGE_CURVE ( 'NONE', #24728, #13033, #37532, .T. ) ;
#47718 = VECTOR ( 'NONE', #52764, 1000.000000000000227 ) ;
#47719 = LINE ( 'NONE', #16465, #37361 ) ;
#47720 = DIRECTION ( 'NONE',  ( 0.005002170337468016433, -0.7660444431189770143, -0.6427681459581293666 ) ) ;
#47721 = DIRECTION ( 'NONE',  ( 0.5449076811759707706, 0.6444004775717708799, -0.5364919789714476250 ) ) ;
#47722 = CARTESIAN_POINT ( 'NONE',  ( -21.47341775636118655, -0.1191753592594197858, 5.122631121243466090 ) ) ;
#47723 = CARTESIAN_POINT ( 'NONE',  ( -18.39746900504187010, 0.000000000000000000, 14.03700784672088808 ) ) ;
#47724 = EDGE_CURVE ( 'NONE', #10313, #8687, #3459, .T. ) ;
#47725 = DIRECTION ( 'NONE',  ( 0.7660212471507180654, -0.6427876096865404731, 0.005961354470445141482 ) ) ;
#47726 = CARTESIAN_POINT ( 'NONE',  ( -20.34003895477433588, 0.5857317160611430484, 5.278610298956506242 ) ) ;
#47727 = AXIS2_PLACEMENT_3D ( 'NONE', #18184, #35260, #22181 ) ;
#47728 = AXIS2_PLACEMENT_3D ( 'NONE', #15630, #50836, #41749 ) ;
#47729 = DIRECTION ( 'NONE',  ( 0.6427681459581294776, -0.7660444431189769032, 0.005002170337467562802 ) ) ;
#47730 = LINE ( 'NONE', #21312, #26787 ) ;
#47731 = DIRECTION ( 'NONE',  ( -0.9335804264972041855, 0.3583679495452941621, 0.000000000000000000 ) ) ;
#47732 = ORIENTED_EDGE ( 'NONE', *, *, #41993, .T. ) ;
#47733 = FACE_OUTER_BOUND ( 'NONE', #30291, .T. ) ;
#47734 = DIRECTION ( 'NONE',  ( 0.007781995580012663651, -3.146120232559066537E-19, -0.9999697198139514409 ) ) ;
#47735 = LINE ( 'NONE', #51688, #12804 ) ;
#47736 = CARTESIAN_POINT ( 'NONE',  ( -2.207734231944874725, 7.028681301134739989, 4.075932526321295768 ) ) ;
#47737 = EDGE_CURVE ( 'NONE', #41560, #16128, #6894, .T. ) ;
#47738 = DIRECTION ( 'NONE',  ( 0.05705673239519651330, -0.9983709377222390602, -2.388043913193231768E-16 ) ) ;
#47739 = AXIS2_PLACEMENT_3D ( 'NONE', #25443, #51578, #43057 ) ;
#47740 = ORIENTED_EDGE ( 'NONE', *, *, #33091, .F. ) ;
#47741 = EDGE_CURVE ( 'NONE', #26517, #28129, #15655, .T. ) ;
#47742 = ORIENTED_EDGE ( 'NONE', *, *, #47852, .T. ) ;
#47743 = EDGE_CURVE ( 'NONE', #14924, #53717, #15962, .T. ) ;
#47744 = FACE_OUTER_BOUND ( 'NONE', #41785, .T. ) ;
#47745 = DIRECTION ( 'NONE',  ( 0.5449076811759707706, 0.6444004775717708799, -0.5364919789714476250 ) ) ;
#47746 = ORIENTED_EDGE ( 'NONE', *, *, #22696, .F. ) ;
#47747 = VECTOR ( 'NONE', #39485, 1000.000000000000114 ) ;
#47748 = DIRECTION ( 'NONE',  ( 0.000000000000000000, -1.000000000000000000, 0.000000000000000000 ) ) ;
#47749 = EDGE_CURVE ( 'NONE', #49950, #7904, #6592, .T. ) ;
#47750 = VERTEX_POINT ( 'NONE', #15143 ) ;
#47751 = FACE_OUTER_BOUND ( 'NONE', #6743, .T. ) ;
#47752 = VECTOR ( 'NONE', #17143, 999.9999999999998863 ) ;
#47753 = ORIENTED_EDGE ( 'NONE', *, *, #33967, .T. ) ;
#47754 = DIRECTION ( 'NONE',  ( -0.7660212471507179544, -0.6427876096865405842, -0.005961354470445141482 ) ) ;
#47755 = EDGE_CURVE ( 'NONE', #14310, #44131, #54292, .T. ) ;
#47756 = AXIS2_PLACEMENT_3D ( 'NONE', #29485, #12151, #33460 ) ;
#47757 = VERTEX_POINT ( 'NONE', #2333 ) ;
#47758 = ORIENTED_EDGE ( 'NONE', *, *, #55858, .F. ) ;
#47759 = ORIENTED_EDGE ( 'NONE', *, *, #45175, .T. ) ;
#47760 = CARTESIAN_POINT ( 'NONE',  ( -15.66124530601080700, -1.489407457353157049, 5.209662645942111148 ) ) ;
#47761 = PLANE ( 'NONE',  #6021 ) ;
#47762 = CARTESIAN_POINT ( 'NONE',  ( -15.87975247367846166, 0.000000000000000000, 2.850166870931599927 ) ) ;
#47763 = VECTOR ( 'NONE', #52640, 1000.000000000000114 ) ;
#47764 = DIRECTION ( 'NONE',  ( -0.005002170337468016433, -0.7660444431189770143, 0.6427681459581293666 ) ) ;
#47765 = VERTEX_POINT ( 'NONE', #32996 ) ;
#47766 = ORIENTED_EDGE ( 'NONE', *, *, #4687, .F. ) ;
#47767 = VECTOR ( 'NONE', #10745, 1000.000000000000227 ) ;
#47768 = AXIS2_PLACEMENT_3D ( 'NONE', #2391, #51207, #6951 ) ;
#47769 = ORIENTED_EDGE ( 'NONE', *, *, #38437, .F. ) ;
#47770 = DIRECTION ( 'NONE',  ( 0.9999697198139515519, 0.000000000000000000, 0.007781995580013368816 ) ) ;
#47771 = VERTEX_POINT ( 'NONE', #33298 ) ;
#47772 = LINE ( 'NONE', #34155, #52013 ) ;
#47773 = ORIENTED_EDGE ( 'NONE', *, *, #41669, .F. ) ;
#47774 = DIRECTION ( 'NONE',  ( 0.7660212471507180654, -0.6427876096865404731, 0.005961354470445141482 ) ) ;
#47775 = DIRECTION ( 'NONE',  ( 0.5449076811759707706, 0.6444004775717708799, -0.5364919789714476250 ) ) ;
#47776 = ORIENTED_EDGE ( 'NONE', *, *, #12784, .F. ) ;
#47777 = CARTESIAN_POINT ( 'NONE',  ( -14.56888064431065821, -0.1191753592594197858, 12.58947452739191064 ) ) ;
#47778 = ORIENTED_EDGE ( 'NONE', *, *, #18897, .F. ) ;
#47779 = AXIS2_PLACEMENT_3D ( 'NONE', #3128, #11666, #28983 ) ;
#47780 = PLANE ( 'NONE',  #18201 ) ;
#47781 = ORIENTED_EDGE ( 'NONE', *, *, #53050, .F. ) ;
#47782 = DIRECTION ( 'NONE',  ( -0.5449076811759708816, 0.6444004775717707689, 0.5364919789714475140 ) ) ;
#47783 = PLANE ( 'NONE',  #21189 ) ;
#47784 = DIRECTION ( 'NONE',  ( 0.5364919789714477361, 0.6444004775717706579, 0.5449076811759711036 ) ) ;
#47785 = ORIENTED_EDGE ( 'NONE', *, *, #43431, .F. ) ;
#47786 = ADVANCED_FACE ( 'NONE', ( #32459 ), #46057, .F. ) ;
#47787 = EDGE_CURVE ( 'NONE', #1287, #55683, #50308, .T. ) ;
#47788 = CARTESIAN_POINT ( 'NONE',  ( -14.10280672071693431, -0.1191753592594197858, 12.40843558753103792 ) ) ;
#47789 = CARTESIAN_POINT ( 'NONE',  ( 2.072287782118878319, 0.000000000000000000, -2.950529333540147015 ) ) ;
#47790 = VECTOR ( 'NONE', #18316, 999.9999999999998863 ) ;
#47791 = CARTESIAN_POINT ( 'NONE',  ( -17.73140113748535285, 0.000000000000000000, 13.85752530597602039 ) ) ;
#47792 = CARTESIAN_POINT ( 'NONE',  ( -17.26532721389163072, 0.000000000000000000, 13.67648636611514590 ) ) ;
#47793 = ADVANCED_FACE ( 'NONE', ( #10859 ), #25055, .F. ) ;
#47794 = CARTESIAN_POINT ( 'NONE',  ( -14.72233906693923267, 5.143464774974014553, 2.236484742513179746 ) ) ;
#47795 = LINE ( 'NONE', #30748, #23395 ) ;
#47796 = AXIS2_PLACEMENT_3D ( 'NONE', #6946, #41294, #16019 ) ;
#47797 = CARTESIAN_POINT ( 'NONE',  ( -23.33693525117809386, 0.000000000000000000, 5.746789908705562944 ) ) ;
#47798 = EDGE_LOOP ( 'NONE', ( #33379, #2665, #18791, #31653 ) ) ;
#47799 = DIRECTION ( 'NONE',  ( 0.3313982828793700097, 0.4028455766673916805, 0.8531650599175528704 ) ) ;
#47800 = LINE ( 'NONE', #25941, #26800 ) ;
#47801 = CARTESIAN_POINT ( 'NONE',  ( -18.82703149329399395, -0.8417996532631562001, 4.167521701613545737 ) ) ;
#47802 = EDGE_LOOP ( 'NONE', ( #44062, #23620, #27551, #50748 ) ) ;
#47803 = DIRECTION ( 'NONE',  ( 0.9999697198139515519, 0.000000000000000000, 0.007781995580013368816 ) ) ;
#47804 = ORIENTED_EDGE ( 'NONE', *, *, #27568, .T. ) ;
#47805 = DIRECTION ( 'NONE',  ( -0.7660212471507179544, -0.6427876096865405842, -0.005961354470445141482 ) ) ;
#47806 = VECTOR ( 'NONE', #10489, 999.9999999999998863 ) ;
#47807 = DIRECTION ( 'NONE',  ( -0.5364919789714478471, 0.6444004775717705469, -0.5449076811759709926 ) ) ;
#47808 = DIRECTION ( 'NONE',  ( 0.007781995580012663651, -3.146120232559066537E-19, -0.9999697198139514409 ) ) ;
#47809 = DIRECTION ( 'NONE',  ( 0.000000000000000000, -1.000000000000000000, 0.000000000000000000 ) ) ;
#47810 = VERTEX_POINT ( 'NONE', #15390 ) ;
#47811 = AXIS2_PLACEMENT_3D ( 'NONE', #10215, #14758, #5676 ) ;
#47812 = ORIENTED_EDGE ( 'NONE', *, *, #51502, .F. ) ;
#47813 = DIRECTION ( 'NONE',  ( 0.000000000000000000, -0.000000000000000000, -1.000000000000000000 ) ) ;
#47814 = LINE ( 'NONE', #663, #41329 ) ;
#47815 = CARTESIAN_POINT ( 'NONE',  ( 2.072287782118878319, 0.000000000000000000, -2.950529333540147015 ) ) ;
#47816 = FACE_OUTER_BOUND ( 'NONE', #33518, .T. ) ;
#47817 = DIRECTION ( 'NONE',  ( 0.007781995580012662783, 0.000000000000000000, -0.9999697198139514409 ) ) ;
#47818 = DIRECTION ( 'NONE',  ( 0.005961354470445682716, -0.6427876096865404731, -0.7660212471507180654 ) ) ;
#47819 = ORIENTED_EDGE ( 'NONE', *, *, #52302, .T. ) ;
#47820 = FACE_OUTER_BOUND ( 'NONE', #5867, .T. ) ;
#47821 = EDGE_CURVE ( 'NONE', #37913, #54234, #29015, .T. ) ;
#47822 = DIRECTION ( 'NONE',  ( -0.9999697198139514409, -0.000000000000000000, -0.007781995580013368816 ) ) ;
#47823 = ORIENTED_EDGE ( 'NONE', *, *, #16838, .T. ) ;
#47824 = ADVANCED_FACE ( 'NONE', ( #28753 ), #50015, .F. ) ;
#47825 = DIRECTION ( 'NONE',  ( 0.9999697198139515519, 0.000000000000000000, 0.007781995580013368816 ) ) ;
#47826 = CARTESIAN_POINT ( 'NONE',  ( -14.01701317841955508, 0.000000000000000000, 2.326005055450897085 ) ) ;
#47827 = LINE ( 'NONE', #8931, #11256 ) ;
#47828 = EDGE_LOOP ( 'NONE', ( #38113, #30001, #32635, #31052 ) ) ;
#47829 = DIRECTION ( 'NONE',  ( 0.9999697198139515519, 0.000000000000000000, 0.007781995580013368816 ) ) ;
#47830 = EDGE_CURVE ( 'NONE', #53467, #33120, #29287, .T. ) ;
#47831 = VERTEX_POINT ( 'NONE', #20194 ) ;
#47832 = EDGE_LOOP ( 'NONE', ( #47141, #17359, #42021, #33784 ) ) ;
#47833 = AXIS2_PLACEMENT_3D ( 'NONE', #20333, #19789, #33966 ) ;
#47834 = VERTEX_POINT ( 'NONE', #46311 ) ;
#47835 = ORIENTED_EDGE ( 'NONE', *, *, #2754, .F. ) ;
#47836 = DIRECTION ( 'NONE',  ( 0.9999697198139515519, 0.000000000000000000, 0.007781995580013368816 ) ) ;
#47837 = ORIENTED_EDGE ( 'NONE', *, *, #4675, .F. ) ;
#47838 = CARTESIAN_POINT ( 'NONE',  ( -15.34503691632512101, 22.06676384394702595, -3.956079653413159036 ) ) ;
#47839 = VECTOR ( 'NONE', #10056, 999.9999999999998863 ) ;
#47840 = EDGE_LOOP ( 'NONE', ( #10720, #27483, #13333, #29583 ) ) ;
#47841 = LINE ( 'NONE', #4948, #37683 ) ;
#47842 = VERTEX_POINT ( 'NONE', #7422 ) ;
#47843 = DIRECTION ( 'NONE',  ( 0.6427681459581294776, -0.7660444431189769032, 0.005002170337467562802 ) ) ;
#47844 = ORIENTED_EDGE ( 'NONE', *, *, #47390, .F. ) ;
#47845 = DIRECTION ( 'NONE',  ( -0.005961354470445682716, -0.6427876096865404731, 0.7660212471507180654 ) ) ;
#47846 = LINE ( 'NONE', #34770, #26831 ) ;
#47847 = DIRECTION ( 'NONE',  ( -0.7660212471507179544, -0.6427876096865405842, -0.005961354470445141482 ) ) ;
#47848 = DIRECTION ( 'NONE',  ( 0.5449076811759707706, 0.6444004775717708799, -0.5364919789714476250 ) ) ;
#47849 = EDGE_CURVE ( 'NONE', #14819, #18282, #42065, .T. ) ;
#47850 = CARTESIAN_POINT ( 'NONE',  ( -17.74404816805336793, 0.000000000000000000, 3.574322630375089460 ) ) ;
#47851 = ORIENTED_EDGE ( 'NONE', *, *, #12053, .T. ) ;
#47852 = EDGE_CURVE ( 'NONE', #44098, #33926, #8012, .T. ) ;
#47853 = EDGE_LOOP ( 'NONE', ( #14784, #28421, #55153, #6374 ) ) ;
#47854 = PLANE ( 'NONE',  #38553 ) ;
#47855 = CARTESIAN_POINT ( 'NONE',  ( -29.86197018149027116, 0.000000000000000000, 8.281335066757780083 ) ) ;
#47856 = EDGE_CURVE ( 'NONE', #48678, #42632, #43477, .T. ) ;
#47857 = ADVANCED_FACE ( 'NONE', ( #4021 ), #48016, .F. ) ;
#47858 = PLANE ( 'NONE',  #19700 ) ;
#47859 = DIRECTION ( 'NONE',  ( 0.000000000000000000, -0.000000000000000000, -1.000000000000000000 ) ) ;
#47860 = PLANE ( 'NONE',  #15839 ) ;
#47861 = CARTESIAN_POINT ( 'NONE',  ( -11.77243710274829525, -0.1191753592594197858, 11.50324088822667612 ) ) ;
#47862 = ORIENTED_EDGE ( 'NONE', *, *, #1593, .F. ) ;
#47863 = CARTESIAN_POINT ( 'NONE',  ( -18.39746900504187010, 0.000000000000000000, 14.03700784672088808 ) ) ;
#47864 = LINE ( 'NONE', #31078, #6835 ) ;
#47865 = VERTEX_POINT ( 'NONE', #13105 ) ;
#47866 = B_SPLINE_CURVE_WITH_KNOTS ( 'NONE', 3,
 ( #8135, #17476, #50724, #55835, #29135, #7561, #24888, #3318, #8983, #26859, #48985, #48726, #13515, #5838, #14369, #30831, #26284, #43883, #44439, #39905, #5543, #31681, #9540, #39350, #31410, #48132, #10085, #985, #23160, #27398, #732, #44183, #44718, #18051 ),
 .UNSPECIFIED., .F., .F.,
 ( 4, 1, 1, 2, 2, 1, 1, 1, 1, 1, 2, 2, 1, 1, 1, 1, 1, 1, 2, 2, 1, 1, 1, 1, 1, 4 ),
 ( 0.000000000000000000, 0.02775256462266485064, 0.03469070577833101993, 0.03555797342278926160, 0.03577479033390380120, 0.03599160724501835468, 0.03642524106724729510, 0.03815977635616276537, 0.04162884693399369895, 0.05550512924531742637, 0.06244327040097930048, 0.06287690422320822703, 0.06331053804543715358, 0.06417780568989517320, 0.06591234097881149001, 0.06938141155664413751, 0.08325769386797447769, 0.1110102584906351164, 0.1248865408019652762, 0.1257538084464233652, 0.1266210760908814403, 0.1283556113797974241, 0.1318246819576294193, 0.1387628231132936596, 0.1665153877359508428, 0.2220205169812650703 ),
 .UNSPECIFIED. ) ;
#47867 = CARTESIAN_POINT ( 'NONE',  ( -18.61226887098971261, 0.000000000000000000, 7.630218703982132311 ) ) ;
#47868 = FACE_OUTER_BOUND ( 'NONE', #11193, .T. ) ;
#47869 = CARTESIAN_POINT ( 'NONE',  ( -15.79151524699580555, 0.000000000000000000, 3.420191679459803957 ) ) ;
#47870 = CARTESIAN_POINT ( 'NONE',  ( -13.53673582514181106, 0.000000000000000000, 12.22817484722816772 ) ) ;
#47871 = ADVANCED_FACE ( 'NONE', ( #8865 ), #34666, .F. ) ;
#47872 = LINE ( 'NONE', #33733, #46451 ) ;
#47873 = VERTEX_POINT ( 'NONE', #3723 ) ;
#47874 = EDGE_LOOP ( 'NONE', ( #53661, #28601, #2005, #26145 ) ) ;
#47875 = PLANE ( 'NONE',  #4915 ) ;
#47876 = FACE_OUTER_BOUND ( 'NONE', #14769, .T. ) ;
#47877 = DIRECTION ( 'NONE',  ( 0.7660212471507180654, -0.6427876096865404731, 0.005961354470445141482 ) ) ;
#47878 = AXIS2_PLACEMENT_3D ( 'NONE', #17120, #29049, #47201 ) ;
#47879 = PLANE ( 'NONE',  #21913 ) ;
#47880 = FACE_OUTER_BOUND ( 'NONE', #16655, .T. ) ;
#47881 = LINE ( 'NONE', #1576, #41858 ) ;
#47882 = DIRECTION ( 'NONE',  ( 0.000000000000000000, -1.000000000000000000, 0.000000000000000000 ) ) ;
#47883 = ORIENTED_EDGE ( 'NONE', *, *, #53891, .T. ) ;
#47884 = DIRECTION ( 'NONE',  ( -0.5364919789714478471, 0.6444004775717705469, -0.5449076811759709926 ) ) ;
#47885 = DIRECTION ( 'NONE',  ( 0.5449076811759707706, 0.6444004775717708799, -0.5364919789714476250 ) ) ;
#47886 = ORIENTED_EDGE ( 'NONE', *, *, #36641, .F. ) ;
#47887 = DIRECTION ( 'NONE',  ( 0.5449076811759707706, 0.6444004775717708799, -0.5364919789714476250 ) ) ;
#47888 = ORIENTED_EDGE ( 'NONE', *, *, #33420, .T. ) ;
#47889 = FACE_OUTER_BOUND ( 'NONE', #15084, .T. ) ;
#47890 = CARTESIAN_POINT ( 'NONE',  ( -21.19256270521356100, 3.362543313726507499, 10.63173860971578577 ) ) ;
#47891 = VERTEX_POINT ( 'NONE', #21041 ) ;
#47892 = EDGE_CURVE ( 'NONE', #16343, #31601, #47453, .T. ) ;
#47893 = ORIENTED_EDGE ( 'NONE', *, *, #43279, .F. ) ;
#47894 = ORIENTED_EDGE ( 'NONE', *, *, #12913, .T. ) ;
#47895 = ORIENTED_EDGE ( 'NONE', *, *, #41088, .T. ) ;
#47896 = VERTEX_POINT ( 'NONE', #29867 ) ;
#47897 = VERTEX_POINT ( 'NONE', #47164 ) ;
#47898 = LINE ( 'NONE', #12690, #55011 ) ;
#47899 = DIRECTION ( 'NONE',  ( 0.5449076811759707706, 0.6444004775717708799, -0.5364919789714476250 ) ) ;
#47900 = DIRECTION ( 'NONE',  ( -0.5449076811759708816, 0.6444004775717707689, 0.5364919789714475140 ) ) ;
#47901 = EDGE_CURVE ( 'NONE', #13341, #41396, #42910, .T. ) ;
#47902 = VERTEX_POINT ( 'NONE', #17343 ) ;
#47903 = LINE ( 'NONE', #7897, #41284 ) ;
#47904 = ORIENTED_EDGE ( 'NONE', *, *, #38161, .T. ) ;
#47905 = ADVANCED_FACE ( 'NONE', ( #51455 ), #30716, .F. ) ;
#47906 = EDGE_LOOP ( 'NONE', ( #11142, #38395, #38933, #51957 ) ) ;
#47907 = EDGE_CURVE ( 'NONE', #50552, #19938, #8269, .T. ) ;
#47908 = DIRECTION ( 'NONE',  ( 0.000000000000000000, -1.000000000000000000, 0.000000000000000000 ) ) ;
#47909 = CARTESIAN_POINT ( 'NONE',  ( -11.77950995886804719, -2.946525016555658905, 6.093242968378755897 ) ) ;
#47910 = CARTESIAN_POINT ( 'NONE',  ( -17.74404816805336793, 0.000000000000000000, 3.574322630375089460 ) ) ;
#47911 = EDGE_CURVE ( 'NONE', #16557, #30900, #25587, .T. ) ;
#47912 = ORIENTED_EDGE ( 'NONE', *, *, #36238, .F. ) ;
#47913 = FACE_OUTER_BOUND ( 'NONE', #4524, .T. ) ;
#47914 = VERTEX_POINT ( 'NONE', #38675 ) ;
#47915 = AXIS2_PLACEMENT_3D ( 'NONE', #39479, #264, #5396 ) ;
#47916 = CARTESIAN_POINT ( 'NONE',  ( -19.07846216694679953, 0.000000000000000000, 7.826596736176912650 ) ) ;
#47917 = EDGE_CURVE ( 'NONE', #41918, #7829, #22180, .T. ) ;
#47918 = DIRECTION ( 'NONE',  ( -0.5364919789714478471, 0.6444004775717705469, -0.5449076811759709926 ) ) ;
#47919 = EDGE_CURVE ( 'NONE', #40788, #29014, #55996, .T. ) ;
#47920 = FACE_OUTER_BOUND ( 'NONE', #55943, .T. ) ;
#47921 = LINE ( 'NONE', #9019, #40410 ) ;
#47922 = DIRECTION ( 'NONE',  ( -0.2588190451025212946, -0.9659258262890680902, 0.000000000000000000 ) ) ;
#47923 = CARTESIAN_POINT ( 'NONE',  ( -10.43442840428654073, 0.000000000000000000, 5.847200200401478476 ) ) ;
#47924 = DIRECTION ( 'NONE',  ( -0.6246952433987894571, 0.7422098413412802076, 0.2426528472758539834 ) ) ;
#47925 = CARTESIAN_POINT ( 'NONE',  ( -27.13182803479460858, 16.99370762638562127, 4.657392947539034544 ) ) ;
#47926 = ORIENTED_EDGE ( 'NONE', *, *, #26719, .F. ) ;
#47927 = CARTESIAN_POINT ( 'NONE',  ( -14.51438381650843468, 4.819660872929010687, 10.42908529298719778 ) ) ;
#47928 = EDGE_CURVE ( 'NONE', #51537, #13509, #16504, .T. ) ;
#47929 = DIRECTION ( 'NONE',  ( -0.3583679495452941066, -0.9335804264972041855, 0.000000000000000000 ) ) ;
#47930 = DIRECTION ( 'NONE',  ( 0.9999697198139515519, 0.000000000000000000, 0.007781995580013368816 ) ) ;
#47931 = DIRECTION ( 'NONE',  ( 0.005002170337468016433, -0.7660444431189770143, -0.6427681459581293666 ) ) ;
#47932 = CARTESIAN_POINT ( 'NONE',  ( -30.80012389882216794, 13.14376521425323752, -4.804632802340537800 ) ) ;
#47933 = DIRECTION ( 'NONE',  ( 0.005961354470445682716, -0.6427876096865404731, -0.7660212471507180654 ) ) ;
#47934 = LINE ( 'NONE', #4228, #7806 ) ;
#47935 = EDGE_CURVE ( 'NONE', #51315, #20494, #38371, .T. ) ;
#47936 = LINE ( 'NONE', #39122, #28312 ) ;
#47937 = EDGE_LOOP ( 'NONE', ( #23674, #35438, #9580, #56001 ) ) ;
#47938 = FACE_OUTER_BOUND ( 'NONE', #22524, .T. ) ;
#47939 = FACE_OUTER_BOUND ( 'NONE', #24968, .T. ) ;
#47940 = FACE_OUTER_BOUND ( 'NONE', #51089, .T. ) ;
#47941 = LINE ( 'NONE', #17007, #42709 ) ;
#47942 = CARTESIAN_POINT ( 'NONE',  ( -19.17193283235963008, -0.1191753592594166911, 6.987202158121982087 ) ) ;
#47943 = DIRECTION ( 'NONE',  ( 0.9999697198139515519, 0.000000000000000000, 0.007781995580013368816 ) ) ;
#47944 = DIRECTION ( 'NONE',  ( -0.7660212471507179544, -0.6427876096865405842, -0.005961354470445141482 ) ) ;
#47945 = DIRECTION ( 'NONE',  ( 0.000000000000000000, -0.000000000000000000, -1.000000000000000000 ) ) ;
#47946 = CARTESIAN_POINT ( 'NONE',  ( -67.23718175846519784, -9.538746327908999234, 3.332842667189706898 ) ) ;
#47947 = EDGE_LOOP ( 'NONE', ( #33686, #51000, #30255, #32993 ) ) ;
#47948 = CARTESIAN_POINT ( 'NONE',  ( -16.99924723426068951, 0.000000000000000000, 13.49389102713827171 ) ) ;
#47949 = AXIS2_PLACEMENT_3D ( 'NONE', #38992, #33594, #55 ) ;
#47950 = VERTEX_POINT ( 'NONE', #34405 ) ;
#47951 = EDGE_CURVE ( 'NONE', #30420, #53062, #51706, .T. ) ;
#47952 = ORIENTED_EDGE ( 'NONE', *, *, #50461, .F. ) ;
#47953 = ORIENTED_EDGE ( 'NONE', *, *, #25179, .T. ) ;
#47954 = ORIENTED_EDGE ( 'NONE', *, *, #44980, .F. ) ;
#47955 = ORIENTED_EDGE ( 'NONE', *, *, #21885, .F. ) ;
#47956 = DIRECTION ( 'NONE',  ( 0.000000000000000000, -1.000000000000000000, 0.000000000000000000 ) ) ;
#47957 = LINE ( 'NONE', #47689, #34864 ) ;
#47958 = EDGE_LOOP ( 'NONE', ( #23802, #35398, #16620, #8850 ) ) ;
#47959 = VERTEX_POINT ( 'NONE', #4322 ) ;
#47960 = EDGE_CURVE ( 'NONE', #5651, #46530, #34980, .T. ) ;
#47961 = CARTESIAN_POINT ( 'NONE',  ( -67.81506811452879901, 0.000000000000000000, -7.454891809856698970 ) ) ;
#47962 = EDGE_LOOP ( 'NONE', ( #49564, #55062, #16911, #14290 ) ) ;
#47963 = LINE ( 'NONE', #22119, #11029 ) ;
#47964 = LINE ( 'NONE', #9064, #2295 ) ;
#47965 = ORIENTED_EDGE ( 'NONE', *, *, #13925, .F. ) ;
#47966 = DIRECTION ( 'NONE',  ( 0.7660212471507180654, -0.6427876096865404731, 0.005961354470445141482 ) ) ;
#47967 = ORIENTED_EDGE ( 'NONE', *, *, #4863, .F. ) ;
#47968 = LINE ( 'NONE', #43686, #44529 ) ;
#47969 = EDGE_CURVE ( 'NONE', #2279, #8289, #51151, .T. ) ;
#47970 = EDGE_CURVE ( 'NONE', #39093, #45157, #52821, .T. ) ;
#47971 = LINE ( 'NONE', #20735, #23634 ) ;
#47972 = ORIENTED_EDGE ( 'NONE', *, *, #2429, .F. ) ;
#47973 = PLANE ( 'NONE',  #5915 ) ;
#47974 = FACE_OUTER_BOUND ( 'NONE', #51084, .T. ) ;
#47975 = CARTESIAN_POINT ( 'NONE',  ( -10.94028622754223967, 0.000000000000000000, 11.14038480894692995 ) ) ;
#47976 = ORIENTED_EDGE ( 'NONE', *, *, #8809, .F. ) ;
#47977 = CARTESIAN_POINT ( 'NONE',  ( -12.30199656298181132, -0.8417996532631574214, 1.632976543561326821 ) ) ;
#47978 = EDGE_LOOP ( 'NONE', ( #28496, #27260, #5246, #51996 ) ) ;
#47979 = EDGE_CURVE ( 'NONE', #29147, #29422, #9700, .T. ) ;
#47980 =( GEOMETRIC_REPRESENTATION_CONTEXT ( 3 ) GLOBAL_UNCERTAINTY_ASSIGNED_CONTEXT ( ( #54139 ) ) GLOBAL_UNIT_ASSIGNED_CONTEXT ( ( #15629, #50281, #11394 ) ) REPRESENTATION_CONTEXT ( 'NONE', 'WORKASPACE' ) );
#47981 = FACE_OUTER_BOUND ( 'NONE', #5173, .T. ) ;
#47982 = DIRECTION ( 'NONE',  ( 0.007781995580012662783, 0.000000000000000000, -0.9999697198139514409 ) ) ;
#47983 = LINE ( 'NONE', #13892, #3125 ) ;
#47984 = DIRECTION ( 'NONE',  ( 0.000000000000000000, -0.000000000000000000, -1.000000000000000000 ) ) ;
#47985 = CARTESIAN_POINT ( 'NONE',  ( -24.53375310857961367, 18.49370688441070953, 4.657440554554202805 ) ) ;
#47986 = PLANE ( 'NONE',  #39443 ) ;
#47987 = DIRECTION ( 'NONE',  ( -0.000000000000000000, -0.000000000000000000, 1.000000000000000000 ) ) ;
#47988 = ADVANCED_FACE ( 'NONE', ( #49421 ), #35512, .T. ) ;
#47989 = DIRECTION ( 'NONE',  ( 0.5364919789714477361, 0.6444004775717706579, 0.5449076811759711036 ) ) ;
#47990 = SHAPE_REPRESENTATION_RELATIONSHIP ( 'NONE' , 'NONE' ,  #53575, #3559 ) ;
#47991 = DIRECTION ( 'NONE',  ( -0.005961354470445682716, -0.6427876096865404731, 0.7660212471507180654 ) ) ;
#47992 = ORIENTED_EDGE ( 'NONE', *, *, #23850, .F. ) ;
#47993 = CARTESIAN_POINT ( 'NONE',  ( -22.36868959911851462, 19.74370688441071309, -4.433759251830043269 ) ) ;
#47994 = CARTESIAN_POINT ( 'NONE',  ( -13.17065887352947762, -0.1191753592594197858, 12.04635770780929427 ) ) ;
#47995 = CARTESIAN_POINT ( 'NONE',  ( -14.58996710526761120, 0.000000000000000000, 2.448865125390635278 ) ) ;
#47996 = DIRECTION ( 'NONE',  ( 0.6427681459581294776, -0.7660444431189769032, 0.005002170337467562802 ) ) ;
#47997 = DIRECTION ( 'NONE',  ( 0.5364919789714477361, 0.6444004775717706579, 0.5449076811759711036 ) ) ;
#47998 = LINE ( 'NONE', #53117, #50107 ) ;
#47999 = EDGE_LOOP ( 'NONE', ( #11638, #7039, #21640, #26300 ) ) ;
#48000 = ORIENTED_EDGE ( 'NONE', *, *, #45155, .F. ) ;
#48001 = CARTESIAN_POINT ( 'NONE',  ( -13.04137698704457904, 0.000000000000000000, 8.284087284458621525 ) ) ;
#48002 = CARTESIAN_POINT ( 'NONE',  ( -11.67244013076689946, 0.000000000000000000, 11.50401908778467863 ) ) ;
#48003 = ORIENTED_EDGE ( 'NONE', *, *, #45443, .T. ) ;
#48004 = EDGE_CURVE ( 'NONE', #34779, #4575, #45172, .T. ) ;
#48005 = CARTESIAN_POINT ( 'NONE',  ( 2.072287782118878319, 0.000000000000000000, -2.950529333540147015 ) ) ;
#48006 = ORIENTED_EDGE ( 'NONE', *, *, #54297, .T. ) ;
#48007 = CARTESIAN_POINT ( 'NONE',  ( -18.98470430123549946, -2.137015261443159009, 4.187443015709999550 ) ) ;
#48008 = EDGE_CURVE ( 'NONE', #14391, #2309, #9964, .T. ) ;
#48009 = ORIENTED_EDGE ( 'NONE', *, *, #19422, .F. ) ;
#48010 = DIRECTION ( 'NONE',  ( -0.5364919789714478471, 0.6444004775717705469, -0.5449076811759709926 ) ) ;
#48011 = ORIENTED_EDGE ( 'NONE', *, *, #306, .F. ) ;
#48012 = VERTEX_POINT ( 'NONE', #27554 ) ;
#48013 = EDGE_CURVE ( 'NONE', #1358, #29284, #44322, .T. ) ;
#48014 = VERTEX_POINT ( 'NONE', #5160 ) ;
#48015 = ADVANCED_FACE ( 'NONE', ( #9393 ), #1439, .F. ) ;
#48016 = PLANE ( 'NONE',  #6654 ) ;
#48017 = DIRECTION ( 'NONE',  ( -0.6427681459581293666, -0.7660444431189770143, -0.005002170337467561935 ) ) ;
#48018 = CARTESIAN_POINT ( 'NONE',  ( -4.032439601142493224, -5.958259985714265738, 4.784710058972824420 ) ) ;
#48019 = EDGE_CURVE ( 'NONE', #7643, #44870, #1135, .T. ) ;
#48020 = EDGE_CURVE ( 'NONE', #7759, #45468, #48278, .T. ) ;
#48021 = ADVANCED_FACE ( 'NONE', ( #6273 ), #14778, .T. ) ;
#48022 = LINE ( 'NONE', #39793, #9327 ) ;
#48023 = VERTEX_POINT ( 'NONE', #53405 ) ;
#48024 = VERTEX_POINT ( 'NONE', #53665 ) ;
#48025 = DIRECTION ( 'NONE',  ( 0.5449076811759707706, 0.6444004775717708799, -0.5364919789714476250 ) ) ;
#48026 = ORIENTED_EDGE ( 'NONE', *, *, #21365, .T. ) ;
#48027 = DIRECTION ( 'NONE',  ( -0.6427681459581293666, -0.7660444431189770143, -0.005002170337467561935 ) ) ;
#48028 = ORIENTED_EDGE ( 'NONE', *, *, #9865, .T. ) ;
#48029 = DIRECTION ( 'NONE',  ( -0.1139275668495183524, 0.9934890585767659488, 4.694855797473114533E-16 ) ) ;
#48030 = DIRECTION ( 'NONE',  ( 0.005002170337468016433, -0.7660444431189770143, -0.6427681459581293666 ) ) ;
#48031 = ORIENTED_EDGE ( 'NONE', *, *, #17691, .T. ) ;
#48032 = CARTESIAN_POINT ( 'NONE',  ( -32.65841372305263235, 0.000000000000000000, 9.367568705923016381 ) ) ;
#48033 = EDGE_CURVE ( 'NONE', #23836, #23840, #14501, .T. ) ;
#48034 = ORIENTED_EDGE ( 'NONE', *, *, #10188, .F. ) ;
#48035 = EDGE_CURVE ( 'NONE', #2673, #39014, #39789, .T. ) ;
#48036 = LINE ( 'NONE', #35005, #1896 ) ;
#48037 = ORIENTED_EDGE ( 'NONE', *, *, #43492, .T. ) ;
#48038 = DIRECTION ( 'NONE',  ( 0.6427681459581294776, -0.7660444431189769032, 0.005002170337467562802 ) ) ;
#48039 = CARTESIAN_POINT ( 'NONE',  ( -22.02184903649736469, 3.848249166794010634, 5.113186466190691171 ) ) ;
#48040 = EDGE_CURVE ( 'NONE', #18921, #4591, #27862, .T. ) ;
#48041 = CARTESIAN_POINT ( 'NONE',  ( -14.66887761629205222, 0.000000000000000000, 12.58869632783390990 ) ) ;
#48042 = VERTEX_POINT ( 'NONE', #609 ) ;
#48043 = FACE_OUTER_BOUND ( 'NONE', #20990, .T. ) ;
#48044 = ADVANCED_FACE ( 'NONE', ( #17937 ), #26714, .F. ) ;
#48045 = LINE ( 'NONE', #17115, #10142 ) ;
#48046 = DIRECTION ( 'NONE',  ( 0.5364919789714477361, 0.6444004775717706579, 0.5449076811759711036 ) ) ;
#48047 = CARTESIAN_POINT ( 'NONE',  ( -12.36248183396243583, -0.3560938001956550081, 2.068350099266224262 ) ) ;
#48048 = CARTESIAN_POINT ( 'NONE',  ( -15.50102849149811135, -0.1191753592594197858, 12.95155240711365430 ) ) ;
#48049 = DIRECTION ( 'NONE',  ( -0.9999697198139514409, -0.000000000000000000, -0.007781995580013368816 ) ) ;
#48050 = FILL_AREA_STYLE_COLOUR ( '', #43083 ) ;
#48051 = ORIENTED_EDGE ( 'NONE', *, *, #8696, .T. ) ;
#48052 = CARTESIAN_POINT ( 'NONE',  ( -13.67826452165829565, 0.000000000000000000, 4.713959708252118297 ) ) ;
#48053 = DIRECTION ( 'NONE',  ( 0.005002170337468016433, -0.7660444431189770143, -0.6427681459581293666 ) ) ;
#48054 = CARTESIAN_POINT ( 'NONE',  ( -20.54126990917373874, -1.000000000000000000, 4.760553241521714440 ) ) ;
#48055 = ORIENTED_EDGE ( 'NONE', *, *, #35877, .F. ) ;
#48056 = DIRECTION ( 'NONE',  ( 0.000000000000000000, -0.000000000000000000, -1.000000000000000000 ) ) ;
#48057 = PLANE ( 'NONE',  #29978 ) ;
#48058 = EDGE_LOOP ( 'NONE', ( #12228, #18065, #44045, #2705 ) ) ;
#48059 = LINE ( 'NONE', #31602, #25290 ) ;
#48060 = DIRECTION ( 'NONE',  ( 0.007781995580012663651, 0.000000000000000000, -0.9999697198139515519 ) ) ;
#48061 = CARTESIAN_POINT ( 'NONE',  ( -10.84028925556084388, -0.1191753592594197858, 11.14116300850493246 ) ) ;
#48062 = CARTESIAN_POINT ( 'NONE',  ( -18.82088497546834915, 0.000000000000000000, 8.736591414639422126 ) ) ;
#48063 = EDGE_LOOP ( 'NONE', ( #3023, #52425, #14330, #25847 ) ) ;
#48064 = ORIENTED_EDGE ( 'NONE', *, *, #16361, .F. ) ;
#48065 = FACE_OUTER_BOUND ( 'NONE', #23379, .T. ) ;
#48066 = CARTESIAN_POINT ( 'NONE',  ( -28.92982233430281980, 0.000000000000000000, 7.919257187036034651 ) ) ;
#48067 = CARTESIAN_POINT ( 'NONE',  ( -28.93060053386082231, -0.1191753592594197858, 8.019254159017428663 ) ) ;
#48068 = CARTESIAN_POINT ( 'NONE',  ( -19.21426901291696865, -0.1941918491731554619, 4.338599984426191547 ) ) ;
#48069 = DIRECTION ( 'NONE',  ( -0.9999697198139514409, -0.000000000000000000, -0.007781995580013368816 ) ) ;
#48070 = DIRECTION ( 'NONE',  ( 0.9999697198139515519, 0.000000000000000000, 0.007781995580013368816 ) ) ;
#48071 = ORIENTED_EDGE ( 'NONE', *, *, #51642, .F. ) ;
#48072 = FACE_OUTER_BOUND ( 'NONE', #43712, .T. ) ;
#48073 = DIRECTION ( 'NONE',  ( -0.5364919789714478471, 0.6444004775717705469, -0.5449076811759709926 ) ) ;
#48074 = ORIENTED_EDGE ( 'NONE', *, *, #15381, .T. ) ;
#48075 = PLANE ( 'NONE',  #15665 ) ;
#48076 = DIRECTION ( 'NONE',  ( 0.000000000000000000, -0.000000000000000000, -1.000000000000000000 ) ) ;
#48077 = FACE_OUTER_BOUND ( 'NONE', #12300, .T. ) ;
#48078 = EDGE_CURVE ( 'NONE', #23836, #3799, #18183, .T. ) ;
#48079 = ADVANCED_FACE ( 'NONE', ( #13929 ), #48584, .F. ) ;
#48080 = VERTEX_POINT ( 'NONE', #31559 ) ;
#48081 = CARTESIAN_POINT ( 'NONE',  ( -12.23851102634202448, -0.1191753592594197858, 11.68427982808754884 ) ) ;
#48082 = VERTEX_POINT ( 'NONE', #11891 ) ;
#48083 = EDGE_CURVE ( 'NONE', #44937, #13109, #50800, .T. ) ;
#48084 = VECTOR ( 'NONE', #2210, 1000.000000000000227 ) ;
#48085 = ORIENTED_EDGE ( 'NONE', *, *, #40100, .T. ) ;
#48086 = ORIENTED_EDGE ( 'NONE', *, *, #4519, .T. ) ;
#48087 = ORIENTED_EDGE ( 'NONE', *, *, #14827, .T. ) ;
#48088 = CARTESIAN_POINT ( 'NONE',  ( -27.06630483948590893, -0.1191753592594197858, 7.295098399573937797 ) ) ;
#48089 = ORIENTED_EDGE ( 'NONE', *, *, #13934, .T. ) ;
#48090 = CARTESIAN_POINT ( 'NONE',  ( -14.16301979303636038, 0.000000000000000000, 7.295511719288459318 ) ) ;
#48091 = EDGE_LOOP ( 'NONE', ( #42517, #36064, #53217, #35396 ) ) ;
#48092 = DIRECTION ( 'NONE',  ( 0.5449076811759707706, 0.6444004775717708799, -0.5364919789714476250 ) ) ;
#48093 = ORIENTED_EDGE ( 'NONE', *, *, #27573, .F. ) ;
#48094 = DIRECTION ( 'NONE',  ( -0.005002170337468016433, -0.7660444431189770143, 0.6427681459581293666 ) ) ;
#48095 = VERTEX_POINT ( 'NONE', #23842 ) ;
#48096 = ADVANCED_FACE ( 'NONE', ( #50543 ), #50241, .F. ) ;
#48097 = DIRECTION ( 'NONE',  ( 0.8531650599175529814, -0.4028455766673920135, -0.3313982828793697877 ) ) ;
#48098 =( BOUNDED_CURVE ( )  B_SPLINE_CURVE ( 3, ( #5225, #10022, #35576, #27071 ),
 .UNSPECIFIED., .F., .F. ) 
 B_SPLINE_CURVE_WITH_KNOTS ( ( 4, 4 ),
 ( -8.881784197001252323E-16, 1.140403016137402359 ),
 .UNSPECIFIED. ) 
 CURVE ( )  GEOMETRIC_REPRESENTATION_ITEM ( )  RATIONAL_B_SPLINE_CURVE ( ( 1.000000000000000000, 0.8945281452387661147, 0.8945281452387661147, 1.000000000000000000 ) ) 
 REPRESENTATION_ITEM ( '' )  );
#48099 = DIRECTION ( 'NONE',  ( -0.000000000000000000, 0.000000000000000000, 1.000000000000000000 ) ) ;
#48100 = DIRECTION ( 'NONE',  ( 0.005961354470445682716, -0.6427876096865404731, -0.7660212471507180654 ) ) ;
#48101 = ADVANCED_FACE ( 'NONE', ( #37771 ), #16174, .F. ) ;
#48102 = CARTESIAN_POINT ( 'NONE',  ( -19.54735067093493939, 2.562506240245330247, 7.319338878784295233 ) ) ;
#48103 = LINE ( 'NONE', #47556, #32873 ) ;
#48104 = VERTEX_POINT ( 'NONE', #45697 ) ;
#48106 = ORIENTED_EDGE ( 'NONE', *, *, #18475, .F. ) ;
#48105 = EDGE_CURVE ( 'NONE', #8726, #43397, #46250, .T. ) ;
#48107 = CARTESIAN_POINT ( 'NONE',  ( -19.78481654831908187, 1.743523803501507485, 4.311398836375244237 ) ) ;
#48108 = DIRECTION ( 'NONE',  ( 0.5449076811759707706, 0.6444004775717708799, -0.5364919789714476250 ) ) ;
#48109 = CARTESIAN_POINT ( 'NONE',  ( -13.45869596940543111, 3.038739411681507185, 7.096224758407104538 ) ) ;
#48110 = CARTESIAN_POINT ( 'NONE',  ( -9.036602278258525800, 2.977129085626424754, 3.729226913157295265 ) ) ;
#48111 = DIRECTION ( 'NONE',  ( -0.5364919789714478471, 0.6444004775717705469, -0.5449076811759709926 ) ) ;
#48112 = LINE ( 'NONE', #26265, #53137 ) ;
#48113 = ORIENTED_EDGE ( 'NONE', *, *, #7952, .T. ) ;
#48114 = CARTESIAN_POINT ( 'NONE',  ( -21.69200269479475551, 4.010151117816511679, 4.979897425557093804 ) ) ;
#48115 = ADVANCED_FACE ( 'NONE', ( #7356 ), #54236, .F. ) ;
#48116 = FACE_OUTER_BOUND ( 'NONE', #3295, .T. ) ;
#48117 = ORIENTED_EDGE ( 'NONE', *, *, #33053, .T. ) ;
#48118 = DIRECTION ( 'NONE',  ( -0.7660212471507179544, -0.6427876096865405842, -0.005961354470445141482 ) ) ;
#48119 = DIRECTION ( 'NONE',  ( 0.005002170337468016433, -0.7660444431189770143, -0.6427681459581293666 ) ) ;
#48120 = VECTOR ( 'NONE', #55950, 1000.000000000000227 ) ;
#48121 = DIRECTION ( 'NONE',  ( 0.005961354470445682716, -0.6427876096865404731, -0.7660212471507180654 ) ) ;
#48122 = DIRECTION ( 'NONE',  ( 0.005002170337468016433, -0.7660444431189770143, -0.6427681459581293666 ) ) ;
#48123 = AXIS2_PLACEMENT_3D ( 'NONE', #38650, #11936, #29577 ) ;
#48124 = CARTESIAN_POINT ( 'NONE',  ( -14.35031752825289431, -2.137015261443157232, 5.763288513568061155 ) ) ;
#48125 = VERTEX_POINT ( 'NONE', #55085 ) ;
#48126 = ORIENTED_EDGE ( 'NONE', *, *, #10414, .F. ) ;
#48127 = CARTESIAN_POINT ( 'NONE',  ( -17.46532115785441519, 0.000000000000000000, 13.67492996699914265 ) ) ;
#48128 = LINE ( 'NONE', #8396, #41281 ) ;
#48129 = FACE_OUTER_BOUND ( 'NONE', #38309, .T. ) ;
#48130 = DIRECTION ( 'NONE',  ( -0.1139275668495183524, 0.9934890585767659488, 4.694855797473114533E-16 ) ) ;
#48131 = CARTESIAN_POINT ( 'NONE',  ( -11.34933193044230038, 0.000000000000000000, 3.993419860576636005 ) ) ;
#48132 = CARTESIAN_POINT ( 'NONE',  ( -16.10294711066915596, 23.36123499678980409, -3.956918830547554666 ) ) ;
#48133 = CARTESIAN_POINT ( 'NONE',  ( -23.33693525117809386, 0.000000000000000000, 5.746789908705562944 ) ) ;
#48134 = DIRECTION ( 'NONE',  ( -0.9999697198139514409, -0.000000000000000000, -0.007781995580013368816 ) ) ;
#48135 = CARTESIAN_POINT ( 'NONE',  ( -24.26908309836554878, 0.000000000000000000, 6.108867788427308376 ) ) ;
#48136 = ORIENTED_EDGE ( 'NONE', *, *, #2312, .F. ) ;
#48137 = CARTESIAN_POINT ( 'NONE',  ( 4.930947970565946470, -1.129146301979396139, -1.967953638240999670 ) ) ;
#48138 = ORIENTED_EDGE ( 'NONE', *, *, #20827, .F. ) ;
#48139 = CARTESIAN_POINT ( 'NONE',  ( -12.33850799832341849, 0.000000000000000000, 11.68350162852954632 ) ) ;
#48140 = CARTESIAN_POINT ( 'NONE',  ( -10.86325900467495842, 0.000000000000000000, 1.242552090245319540 ) ) ;
#48141 = ADVANCED_FACE ( 'NONE', ( #11642 ), #53955, .F. ) ;
#48142 = VERTEX_POINT ( 'NONE', #33496 ) ;
#48143 = AXIS2_PLACEMENT_3D ( 'NONE', #32935, #49429, #10811 ) ;
#48144 = VERTEX_POINT ( 'NONE', #28685 ) ;
#48145 = EDGE_CURVE ( 'NONE', #47896, #5013, #23573, .T. ) ;
#48146 = ADVANCED_FACE ( 'NONE', ( #28958 ), #2801, .F. ) ;
#48147 = ORIENTED_EDGE ( 'NONE', *, *, #4151, .T. ) ;
#48148 = VERTEX_POINT ( 'NONE', #1968 ) ;
#48149 = EDGE_LOOP ( 'NONE', ( #29940, #24530, #7125, #23659, #45044 ) ) ;
#48150 = EDGE_LOOP ( 'NONE', ( #26110, #35624, #39436, #52042 ) ) ;
#48151 = DIRECTION ( 'NONE',  ( 0.5449076811759707706, 0.6444004775717708799, -0.5364919789714476250 ) ) ;
#48152 = DIRECTION ( 'NONE',  ( 0.000000000000000000, -0.000000000000000000, -1.000000000000000000 ) ) ;
#48153 = DIRECTION ( 'NONE',  ( -0.7660212471507179544, -0.6427876096865405842, -0.005961354470445141482 ) ) ;
#48154 = VECTOR ( 'NONE', #14193, 1000.000000000000227 ) ;
#48155 = ORIENTED_EDGE ( 'NONE', *, *, #47749, .T. ) ;
#48156 = CARTESIAN_POINT ( 'NONE',  ( -21.03941874682061197, 4.819660872929009798, 12.96363045103941403 ) ) ;
#48157 = ORIENTED_EDGE ( 'NONE', *, *, #11972, .F. ) ;
#48158 = ORIENTED_EDGE ( 'NONE', *, *, #14407, .T. ) ;
#48159 = VECTOR ( 'NONE', #2168, 1000.000000000000227 ) ;
#48160 = LINE ( 'NONE', #30605, #29275 ) ;
#48161 = CARTESIAN_POINT ( 'NONE',  ( -10.00813838035478298, 0.000000000000000000, 10.77830692922518452 ) ) ;
#48162 = DIRECTION ( 'NONE',  ( 0.007781995580012663651, 0.000000000000000000, -0.9999697198139515519 ) ) ;
#48163 = EDGE_LOOP ( 'NONE', ( #26316, #10160, #17628, #22049 ) ) ;
#48164 = DIRECTION ( 'NONE',  ( -0.7660212471507179544, -0.6427876096865405842, -0.005961354470445141482 ) ) ;
#48165 = ORIENTED_EDGE ( 'NONE', *, *, #46522, .T. ) ;
#48166 = DIRECTION ( 'NONE',  ( 0.5449076811759707706, 0.6444004775717708799, -0.5364919789714476250 ) ) ;
#48167 = CARTESIAN_POINT ( 'NONE',  ( -14.07383107636587738, -0.1191753592594190225, 8.685127515039473778 ) ) ;
#48168 = EDGE_CURVE ( 'NONE', #2142, #54076, #19303, .T. ) ;
#48169 = CARTESIAN_POINT ( 'NONE',  ( -13.73672976910459909, 0.000000000000000000, 12.22661844811216270 ) ) ;
#48170 = DIRECTION ( 'NONE',  ( 0.000000000000000000, -1.000000000000000000, 0.000000000000000000 ) ) ;
#48171 = DIRECTION ( 'NONE',  ( 0.9659258262890682012, -0.2588190451025213501, 0.000000000000000000 ) ) ;
#48172 = EDGE_CURVE ( 'NONE', #33376, #38808, #15069, .T. ) ;
#48173 = CARTESIAN_POINT ( 'NONE',  ( -21.47419595591918906, 0.000000000000000000, 5.222628093224860102 ) ) ;
#48174 = PLANE ( 'NONE',  #9425 ) ;
#48175 = CARTESIAN_POINT ( 'NONE',  ( -13.08486533123210194, 0.000000000000000000, 1.963927175729152541 ) ) ;
#48176 = VERTEX_POINT ( 'NONE', #32401 ) ;
#48177 = CARTESIAN_POINT ( 'NONE',  ( -24.26986129792355129, -0.1191753592594197858, 6.208864760408702388 ) ) ;
#48178 = EDGE_CURVE ( 'NONE', #49806, #36594, #19604, .T. ) ;
#48179 = VECTOR ( 'NONE', #33738, 1000.000000000000000 ) ;
#48180 = VECTOR ( 'NONE', #34925, 999.9999999999998863 ) ;
#48181 = DIRECTION ( 'NONE',  ( 0.007781995580012663651, -3.146120232559066537E-19, -0.9999697198139514409 ) ) ;
#48182 = CARTESIAN_POINT ( 'NONE',  ( -19.62219946167430251, -0.1191753592594169547, 5.137037730065149077 ) ) ;
#48183 = CARTESIAN_POINT ( 'NONE',  ( -11.20636620717317378, 0.000000000000000000, 11.32298014792380414 ) ) ;
#48184 = EDGE_CURVE ( 'NONE', #171, #25528, #46004, .T. ) ;
#48185 = CARTESIAN_POINT ( 'NONE',  ( -16.45088425288988176, 21.42830258649871311, -4.066195520365398330 ) ) ;
#48186 = LINE ( 'NONE', #53327, #42191 ) ;
#48187 = LINE ( 'NONE', #53028, #54037 ) ;
#48188 = PLANE ( 'NONE',  #29205 ) ;
#48189 = EDGE_LOOP ( 'NONE', ( #50881, #28835, #16433, #20982 ) ) ;
#48190 = LINE ( 'NONE', #9298, #51104 ) ;
#48191 = FACE_OUTER_BOUND ( 'NONE', #19526, .T. ) ;
#48192 = LINE ( 'NONE', #38864, #2786 ) ;
#48193 = DIRECTION ( 'NONE',  ( -1.007958083594381472E-15, 3.869188571150965639E-16, -1.000000000000000000 ) ) ;
#48194 = FACE_OUTER_BOUND ( 'NONE', #36150, .T. ) ;
#48195 = DIRECTION ( 'NONE',  ( 0.5364919789714477361, 0.6444004775717706579, 0.5449076811759711036 ) ) ;
#48196 = ADVANCED_FACE ( 'NONE', ( #15334 ), #32650, .F. ) ;
#48197 = CARTESIAN_POINT ( 'NONE',  ( -14.56888064431065821, -0.1191753592594197858, 12.58947452739191064 ) ) ;
#48198 = AXIS2_PLACEMENT_3D ( 'NONE', #17582, #52234, #34919 ) ;
#48199 = CARTESIAN_POINT ( 'NONE',  ( -29.93654370153088706, -1.000000000000000000, 22.35628214185738116 ) ) ;
#48200 = DIRECTION ( 'NONE',  ( 0.007781995580012663651, -3.146120232559066537E-19, -0.9999697198139514409 ) ) ;
#48201 = ADVANCED_FACE ( 'NONE', ( #54781 ), #7110, .F. ) ;
#48202 = VERTEX_POINT ( 'NONE', #34066 ) ;
#48203 = EDGE_CURVE ( 'NONE', #30292, #33948, #9557, .T. ) ;
#48204 = EDGE_CURVE ( 'NONE', #18526, #22565, #46844, .T. ) ;
#48205 = ORIENTED_EDGE ( 'NONE', *, *, #29223, .F. ) ;
#48206 = ORIENTED_EDGE ( 'NONE', *, *, #9500, .F. ) ;
#48207 = ORIENTED_EDGE ( 'NONE', *, *, #54672, .F. ) ;
#48208 = ORIENTED_EDGE ( 'NONE', *, *, #16068, .F. ) ;
#48209 = PLANE ( 'NONE',  #28707 ) ;
#48210 = CARTESIAN_POINT ( 'NONE',  ( -11.62702749645772826, 0.000000000000000000, 5.668593104918477898 ) ) ;
#48211 = EDGE_CURVE ( 'NONE', #52307, #21963, #16728, .T. ) ;
#48212 = VECTOR ( 'NONE', #25438, 1000.000000000000227 ) ;
#48213 = AXIS2_PLACEMENT_3D ( 'NONE', #33325, #24778, #38118 ) ;
#48214 = ORIENTED_EDGE ( 'NONE', *, *, #22789, .F. ) ;
#48215 = ORIENTED_EDGE ( 'NONE', *, *, #35787, .F. ) ;
#48216 = EDGE_CURVE ( 'NONE', #2943, #3628, #31118, .T. ) ;
#48217 = AXIS2_PLACEMENT_3D ( 'NONE', #45256, #14041, #31911 ) ;
#48218 = CARTESIAN_POINT ( 'NONE',  ( -16.37261523729198132, -0.1191753592594188005, 5.531658815698983211 ) ) ;
#48219 = VERTEX_POINT ( 'NONE', #43147 ) ;
#48220 = PLANE ( 'NONE',  #25508 ) ;
#48221 = LINE ( 'NONE', #811, #55861 ) ;
#48222 = ORIENTED_EDGE ( 'NONE', *, *, #38197, .T. ) ;
#48223 = DIRECTION ( 'NONE',  ( 0.6246952433987894571, -0.7422098413412800966, -0.2426528472758541777 ) ) ;
#48224 = ORIENTED_EDGE ( 'NONE', *, *, #35979, .F. ) ;
#48225 = FACE_OUTER_BOUND ( 'NONE', #12110, .T. ) ;
#48226 = VECTOR ( 'NONE', #6703, 999.9999999999998863 ) ;
#48227 = DIRECTION ( 'NONE',  ( 0.000000000000000000, -0.000000000000000000, 1.000000000000000000 ) ) ;
#48228 = AXIS2_PLACEMENT_3D ( 'NONE', #40142, #23115, #45246 ) ;
#48229 = CARTESIAN_POINT ( 'NONE',  ( -17.26532721389163072, 0.000000000000000000, 13.67648636611514590 ) ) ;
#48230 = CARTESIAN_POINT ( 'NONE',  ( -31.72626587586518099, 0.000000000000000000, 9.005490826201270949 ) ) ;
#48231 = ORIENTED_EDGE ( 'NONE', *, *, #13526, .T. ) ;
#48232 = DIRECTION ( 'NONE',  ( -0.005002170337468016433, -0.7660444431189770143, 0.6427681459581293666 ) ) ;
#48233 = PLANE ( 'NONE',  #21121 ) ;
#48234 = CARTESIAN_POINT ( 'NONE',  ( -8.935550834329328396, -0.1191753592594181482, 5.220203700729370233 ) ) ;
#48235 = ORIENTED_EDGE ( 'NONE', *, *, #34843, .F. ) ;
#48236 = DIRECTION ( 'NONE',  ( -0.5364919789714478471, 0.6444004775717705469, -0.5449076811759709926 ) ) ;
#48237 = ORIENTED_EDGE ( 'NONE', *, *, #21775, .F. ) ;
#48238 = DIRECTION ( 'NONE',  ( -0.9999697198139514409, -0.000000000000000000, -0.007781995580013368816 ) ) ;
#48239 = CARTESIAN_POINT ( 'NONE',  ( -17.92052085394417205, 1.743523803501506375, 3.587243076931753816 ) ) ;
#48240 = CARTESIAN_POINT ( 'NONE',  ( -16.73515930820439124, 0.000000000000000000, 5.259508372212608585 ) ) ;
#48241 = CARTESIAN_POINT ( 'NONE',  ( -11.67244013076689946, 0.000000000000000000, 11.50401908778467863 ) ) ;
#48242 = ADVANCED_FACE ( 'NONE', ( #25265 ), #18330, .F. ) ;
#48243 = DIRECTION ( 'NONE',  ( -0.6427681459581293666, -0.7660444431189770143, -0.005002170337467561935 ) ) ;
#48244 = LINE ( 'NONE', #9359, #15921 ) ;
#48245 = LINE ( 'NONE', #43707, #16166 ) ;
#48246 = PLANE ( 'NONE',  #31126 ) ;
#48247 = SURFACE_STYLE_USAGE ( .BOTH. , #32076 ) ;
#48248 = DIRECTION ( 'NONE',  ( -0.5364919789714478471, 0.6444004775717705469, -0.5449076811759709926 ) ) ;
#48249 = ORIENTED_EDGE ( 'NONE', *, *, #31704, .T. ) ;
#48250 = VECTOR ( 'NONE', #42272, 999.9999999999998863 ) ;
#48251 = CARTESIAN_POINT ( 'NONE',  ( -6.903226477722774312, 6.739079746892438827, 5.899821174169304960 ) ) ;
#48252 = DIRECTION ( 'NONE',  ( 0.7660212471507180654, -0.6427876096865404731, 0.005961354470445141482 ) ) ;
#48253 = CARTESIAN_POINT ( 'NONE',  ( -14.86798956032420094, 0.000000000000000000, 4.166042909511353365 ) ) ;
#48254 = ADVANCED_FACE ( 'NONE', ( #35671 ), #14101, .F. ) ;
#48255 = CIRCLE ( 'NONE', #31939, 1.750000000000003331 ) ;
#48256 = VECTOR ( 'NONE', #14201, 1000.000000000000227 ) ;
#48257 = CARTESIAN_POINT ( 'NONE',  ( -24.26908309836554878, 0.000000000000000000, 6.108867788427308376 ) ) ;
#48258 = EDGE_CURVE ( 'NONE', #32717, #13662, #31428, .T. ) ;
#48259 = CARTESIAN_POINT ( 'NONE',  ( -16.00300540497972790, 0.000000000000000000, 4.895874093374860792 ) ) ;
#48260 = ADVANCED_FACE ( 'NONE', ( #7953 ), #29809, .F. ) ;
#48261 = DIRECTION ( 'NONE',  ( 0.007781995580012663651, -3.146120232559066537E-19, -0.9999697198139514409 ) ) ;
#48262 = ORIENTED_EDGE ( 'NONE', *, *, #34804, .T. ) ;
#48263 = VECTOR ( 'NONE', #13027, 999.9999999999998863 ) ;
#48264 = VECTOR ( 'NONE', #28717, 1000.000000000000227 ) ;
#48265 = EDGE_LOOP ( 'NONE', ( #11695, #22477, #40945, #52366 ) ) ;
#48266 = DIRECTION ( 'NONE',  ( -0.6427681459581293666, -0.7660444431189770143, -0.005002170337467561935 ) ) ;
#48267 = DIRECTION ( 'NONE',  ( -0.7660212471507179544, -0.6427876096865405842, -0.005961354470445141482 ) ) ;
#48268 = ORIENTED_EDGE ( 'NONE', *, *, #22829, .T. ) ;
#48269 = ADVANCED_FACE ( 'NONE', ( #3661 ), #29529, .F. ) ;
#48270 = DIRECTION ( 'NONE',  ( 0.007781995580012662783, 0.000000000000000000, -0.9999697198139514409 ) ) ;
#48271 = COLOUR_RGB ( '', 0.09019608, 0.27058824, 0.51372549) ;
#48272 = ORIENTED_EDGE ( 'NONE', *, *, #30978, .T. ) ;
#48273 = LINE ( 'NONE', #13398, #50114 ) ;
#48274 = EDGE_CURVE ( 'NONE', #42565, #30246, #44203, .T. ) ;
#48275 = ORIENTED_EDGE ( 'NONE', *, *, #20528, .F. ) ;
#48276 = VERTEX_POINT ( 'NONE', #24981 ) ;
#48277 = ORIENTED_EDGE ( 'NONE', *, *, #22692, .F. ) ;
#48278 = LINE ( 'NONE', #52551, #18441 ) ;
#48279 = LINE ( 'NONE', #44039, #51373 ) ;
#48280 = DIRECTION ( 'NONE',  ( 0.000000000000000000, -1.000000000000000000, 0.000000000000000000 ) ) ;
#48281 = EDGE_CURVE ( 'NONE', #47104, #40951, #42303, .T. ) ;
#48282 = DIRECTION ( 'NONE',  ( -0.005002170337468016433, -0.7660444431189770143, 0.6427681459581293666 ) ) ;
#48283 = EDGE_LOOP ( 'NONE', ( #46911, #46743, #32452, #52249 ) ) ;
#48284 = VERTEX_POINT ( 'NONE', #25521 ) ;
#48285 = AXIS2_PLACEMENT_3D ( 'NONE', #18894, #4983, #49250 ) ;
#48286 = EDGE_CURVE ( 'NONE', #47084, #17177, #8209, .T. ) ;
#48287 = DIRECTION ( 'NONE',  ( -0.5449076811759708816, 0.6444004775717707689, 0.5364919789714475140 ) ) ;
#48288 = ORIENTED_EDGE ( 'NONE', *, *, #44980, .T. ) ;
#48289 = VECTOR ( 'NONE', #6665, 1000.000000000000227 ) ;
#48290 = FACE_OUTER_BOUND ( 'NONE', #45720, .T. ) ;
#48291 = ORIENTED_EDGE ( 'NONE', *, *, #22220, .F. ) ;
#48292 = PLANE ( 'NONE',  #34211 ) ;
#48293 = PLANE ( 'NONE',  #33988 ) ;
#48294 = VECTOR ( 'NONE', #23761, 1000.000000000000114 ) ;
#48295 = AXIS2_PLACEMENT_3D ( 'NONE', #46420, #37099, #20624 ) ;
#48296 = ORIENTED_EDGE ( 'NONE', *, *, #10222, .F. ) ;
#48297 = LINE ( 'NONE', #55714, #13213 ) ;
#48298 = EDGE_LOOP ( 'NONE', ( #30853, #2613, #9113, #34907 ) ) ;
#48299 = VECTOR ( 'NONE', #36995, 1000.000000000000227 ) ;
#48300 = DIRECTION ( 'NONE',  ( -0.5364919789714478471, 0.6444004775717705469, -0.5449076811759709926 ) ) ;
#48301 = VECTOR ( 'NONE', #27517, 999.9999999999998863 ) ;
#48302 = ORIENTED_EDGE ( 'NONE', *, *, #10545, .F. ) ;
#48303 = CARTESIAN_POINT ( 'NONE',  ( -9.987828218865807628, 0.6049996566053985614, 1.280352617363947898 ) ) ;
#48304 = CARTESIAN_POINT ( 'NONE',  ( -19.06334656290779250, 0.000000000000000000, 8.565378508916090539 ) ) ;
#48305 = CARTESIAN_POINT ( 'NONE',  ( -18.76354595665420177, -0.1191753592594177458, 14.21882498613976331 ) ) ;
#48306 = ORIENTED_EDGE ( 'NONE', *, *, #10714, .F. ) ;
#48307 = CARTESIAN_POINT ( 'NONE',  ( -19.72429228760297448, 0.000000000000000000, 5.405572261783524013 ) ) ;
#48308 = DIRECTION ( 'NONE',  ( -0.7660212471507179544, -0.6427876096865405842, -0.005961354470445141482 ) ) ;
#48309 = DIRECTION ( 'NONE',  ( 0.5364919789714477361, 0.6444004775717706579, 0.5449076811759711036 ) ) ;
#48310 = VECTOR ( 'NONE', #51031, 999.9999999999998863 ) ;
#48311 = EDGE_CURVE ( 'NONE', #19751, #27927, #4256, .T. ) ;
#48312 = LINE ( 'NONE', #35546, #33196 ) ;
#48313 = VECTOR ( 'NONE', #47899, 1000.000000000000114 ) ;
#48314 = DIRECTION ( 'NONE',  ( 0.5364919789714477361, 0.6444004775717706579, 0.5449076811759711036 ) ) ;
#48315 = PLANE ( 'NONE',  #50585 ) ;
#48316 = CARTESIAN_POINT ( 'NONE',  ( -13.28410798335889176, 1.743523803501505709, 4.902739383989964672 ) ) ;
#48317 = ORIENTED_EDGE ( 'NONE', *, *, #52128, .T. ) ;
#48318 = DIRECTION ( 'NONE',  ( 0.005002170337468016433, -0.7660444431189770143, -0.6427681459581293666 ) ) ;
#48319 = PLANE ( 'NONE',  #9589 ) ;
#48320 = FACE_OUTER_BOUND ( 'NONE', #37306, .T. ) ;
#48321 = EDGE_LOOP ( 'NONE', ( #21569, #52972, #34842, #37100 ) ) ;
#48322 = LINE ( 'NONE', #43786, #267 ) ;
#48323 = CARTESIAN_POINT ( 'NONE',  ( -15.96710241509184058, -0.1191753592594218814, 13.13259134697452879 ) ) ;
#48324 = EDGE_LOOP ( 'NONE', ( #15301, #5588, #18642, #30085 ) ) ;
#48325 = EDGE_CURVE ( 'NONE', #24915, #1847, #20718, .T. ) ;
#48326 = VECTOR ( 'NONE', #33859, 1000.000000000000227 ) ;
#48327 = ADVANCED_FACE ( 'NONE', ( #51077 ), #55927, .F. ) ;
#48328 = EDGE_CURVE ( 'NONE', #8596, #8862, #38886, .T. ) ;
#48329 = CARTESIAN_POINT ( 'NONE',  ( -10.94028622754223967, 0.000000000000000000, 11.14038480894692995 ) ) ;
#48330 = CARTESIAN_POINT ( 'NONE',  ( -14.39030005034598148, 0.000000000000000000, 2.492426064285516940 ) ) ;
#48331 = AXIS2_PLACEMENT_3D ( 'NONE', #40933, #49176, #23365 ) ;
#48332 = DIRECTION ( 'NONE',  ( 0.007781995580012663651, -3.146120232559066537E-19, -0.9999697198139514409 ) ) ;
#48333 = EDGE_CURVE ( 'NONE', #29115, #5375, #35387, .T. ) ;
#48334 = CARTESIAN_POINT ( 'NONE',  ( -9.305160666641581813, 0.000000000000000000, 5.855988423053500647 ) ) ;
#48335 = ORIENTED_EDGE ( 'NONE', *, *, #26638, .T. ) ;
#48336 = VERTEX_POINT ( 'NONE', #31965 ) ;
#48337 = CARTESIAN_POINT ( 'NONE',  ( -18.92731312331513038, -2.622721114510660367, 4.149653773530951106 ) ) ;
#48338 = CARTESIAN_POINT ( 'NONE',  ( -17.69892174394995621, 0.000000000000000000, 9.683992987769761029 ) ) ;
#48339 = VECTOR ( 'NONE', #12810, 1000.000000000000114 ) ;
#48340 = LINE ( 'NONE', #10011, #31423 ) ;
#48341 = AXIS2_PLACEMENT_3D ( 'NONE', #7606, #15024, #45658 ) ;
#48342 = FACE_OUTER_BOUND ( 'NONE', #44593, .T. ) ;
#48343 = AXIS2_PLACEMENT_3D ( 'NONE', #45006, #53504, #27375 ) ;
#48344 = LINE ( 'NONE', #9456, #54565 ) ;
#48345 = ADVANCED_FACE ( 'NONE', ( #45306 ), #22879, .F. ) ;
#48346 = CARTESIAN_POINT ( 'NONE',  ( -17.68455147642353964, 0.000000000000000000, 7.837444471480940145 ) ) ;
#48347 = ORIENTED_EDGE ( 'NONE', *, *, #7894, .T. ) ;
#48348 = CARTESIAN_POINT ( 'NONE',  ( -14.09507759759798340, -4.565544526780662693, 9.649774915774109729 ) ) ;
#48349 = ADVANCED_FACE ( 'NONE', ( #36497 ), #6406, .F. ) ;
#48350 = VECTOR ( 'NONE', #55402, 1000.000000000000000 ) ;
#48351 = DIRECTION ( 'NONE',  ( 0.000000000000000000, -1.000000000000000000, 0.000000000000000000 ) ) ;
#48352 = VECTOR ( 'NONE', #6309, 1000.000000000000227 ) ;
#48353 = ORIENTED_EDGE ( 'NONE', *, *, #4675, .T. ) ;
#48354 = ADVANCED_FACE ( 'NONE', ( #15219 ), #53815, .F. ) ;
#48355 = CARTESIAN_POINT ( 'NONE',  ( -19.45503627000849889, -1.000000000000000000, 7.556996783084074742 ) ) ;
#48356 = PLANE ( 'NONE',  #17773 ) ;
#48357 = CARTESIAN_POINT ( 'NONE',  ( -14.02843573335194094, -0.1134144341941982215, 2.230747270852929454 ) ) ;
#48358 = ORIENTED_EDGE ( 'NONE', *, *, #24670, .F. ) ;
#48359 = EDGE_CURVE ( 'NONE', #54876, #12832, #23709, .T. ) ;
#48360 = CARTESIAN_POINT ( 'NONE',  ( -23.33849165029409889, 0.000000000000000000, 5.946783852668351855 ) ) ;
#48361 = ORIENTED_EDGE ( 'NONE', *, *, #36430, .T. ) ;
#48362 = VECTOR ( 'NONE', #46699, 1000.000000000000000 ) ;
#48363 = ORIENTED_EDGE ( 'NONE', *, *, #39715, .T. ) ;
#48364 = ORIENTED_EDGE ( 'NONE', *, *, #16073, .F. ) ;
#48365 = VERTEX_POINT ( 'NONE', #49003 ) ;
#48366 = CARTESIAN_POINT ( 'NONE',  ( -11.82127333340995179, 0.000000000000000000, 4.928417299286945052 ) ) ;
#48367 = ORIENTED_EDGE ( 'NONE', *, *, #16603, .T. ) ;
#48368 = AXIS2_PLACEMENT_3D ( 'NONE', #10182, #40843, #28330 ) ;
#48369 = CARTESIAN_POINT ( 'NONE',  ( -10.30072098979975692, -0.1191753592594199940, 1.516258932847700303 ) ) ;
#48370 = FACE_OUTER_BOUND ( 'NONE', #31505, .T. ) ;
#48371 = ORIENTED_EDGE ( 'NONE', *, *, #53363, .F. ) ;
#48372 = DIRECTION ( 'NONE',  ( -0.5364919789714478471, 0.6444004775717705469, -0.5449076811759709926 ) ) ;
#48373 = ORIENTED_EDGE ( 'NONE', *, *, #51519, .F. ) ;
#48374 = DIRECTION ( 'NONE',  ( 0.007781995580012663651, 0.000000000000000000, -0.9999697198139515519 ) ) ;
#48375 = VECTOR ( 'NONE', #35570, 1000.000000000000000 ) ;
#48376 = ORIENTED_EDGE ( 'NONE', *, *, #11932, .T. ) ;
#48377 = FACE_OUTER_BOUND ( 'NONE', #23934, .T. ) ;
#48378 = LINE ( 'NONE', #9492, #32044 ) ;
#48379 = DIRECTION ( 'NONE',  ( 0.9999697198139515519, 0.000000000000000000, 0.007781995580013368816 ) ) ;
#48380 = CARTESIAN_POINT ( 'NONE',  ( -11.75806593121445864, -0.1941918491731561003, 1.567865752637991994 ) ) ;
#48381 = FACE_OUTER_BOUND ( 'NONE', #6569, .T. ) ;
#48382 = AXIS2_PLACEMENT_3D ( 'NONE', #33073, #7232, #54938 ) ;
#48383 = DIRECTION ( 'NONE',  ( -0.7660212471507179544, -0.6427876096865405842, -0.005961354470445141482 ) ) ;
#48384 = ORIENTED_EDGE ( 'NONE', *, *, #33563, .F. ) ;
#48385 = EDGE_CURVE ( 'NONE', #22163, #31339, #49836, .T. ) ;
#48386 = CIRCLE ( 'NONE', #5758, 0.2499999999999997780 ) ;
#48387 = AXIS2_PLACEMENT_3D ( 'NONE', #11321, #24111, #7929 ) ;
#48388 = EDGE_LOOP ( 'NONE', ( #43901, #28133, #1770, #50165 ) ) ;
#48389 = CARTESIAN_POINT ( 'NONE',  ( -12.13851405436063047, 0.000000000000000000, 11.68505802764555135 ) ) ;
#48390 = CARTESIAN_POINT ( 'NONE',  ( -18.19747506107908563, 0.000000000000000000, 14.03856424583689311 ) ) ;
#48391 = EDGE_CURVE ( 'NONE', #52053, #51242, #51453, .T. ) ;
#48392 = LINE ( 'NONE', #1548, #38765 ) ;
#48393 = VECTOR ( 'NONE', #10395, 999.9999999999998863 ) ;
#48394 = VECTOR ( 'NONE', #33470, 999.9999999999998863 ) ;
#48395 = CARTESIAN_POINT ( 'NONE',  ( -20.54126990917373519, -0.1191753592594197858, 4.760553241521720658 ) ) ;
#48396 = ORIENTED_EDGE ( 'NONE', *, *, #11109, .T. ) ;
#48397 = LINE ( 'NONE', #53766, #46695 ) ;
#48398 = LINE ( 'NONE', #39329, #11411 ) ;
#48399 = ORIENTED_EDGE ( 'NONE', *, *, #5711, .T. ) ;
#48400 = DIRECTION ( 'NONE',  ( 0.9999697198139515519, 0.000000000000000000, 0.007781995580013368816 ) ) ;
#48401 = LINE ( 'NONE', #1255, #6794 ) ;
#48402 = ORIENTED_EDGE ( 'NONE', *, *, #14449, .T. ) ;
#48403 = EDGE_CURVE ( 'NONE', #12574, #26765, #49582, .T. ) ;
#48404 = ADVANCED_FACE ( 'NONE', ( #45047 ), #48744, .F. ) ;
#48405 = EDGE_CURVE ( 'NONE', #8121, #17210, #27149, .T. ) ;
#48406 = CARTESIAN_POINT ( 'NONE',  ( -18.67619601524082285, 0.000000000000000000, 3.936400510096834893 ) ) ;
#48407 = LINE ( 'NONE', #22006, #13339 ) ;
#48408 = LINE ( 'NONE', #18296, #40470 ) ;
#48409 = EDGE_CURVE ( 'NONE', #36728, #1702, #18633, .T. ) ;
#48410 = CARTESIAN_POINT ( 'NONE',  ( -12.28878428375632303, 0.000000000000000000, 5.294111090776699058 ) ) ;
#48411 = CARTESIAN_POINT ( 'NONE',  ( -27.06708303904391144, 0.000000000000000000, 7.395095371555332697 ) ) ;
#48412 = ORIENTED_EDGE ( 'NONE', *, *, #50958, .F. ) ;
#48413 = AXIS2_PLACEMENT_3D ( 'NONE', #7739, #54307, #15403 ) ;
#48414 = ORIENTED_EDGE ( 'NONE', *, *, #4088, .T. ) ;
#48415 = LINE ( 'NONE', #9532, #32113 ) ;
#48416 = CARTESIAN_POINT ( 'NONE',  ( 5.454439161952889137, 0.000000000000000000, 2.500037857468615510 ) ) ;
#48417 = CARTESIAN_POINT ( 'NONE',  ( -12.93729377823301618, -3.756034771668160577, 7.871508942076431481 ) ) ;
#48418 = VECTOR ( 'NONE', #31375, 1000.000000000000000 ) ;
#48419 = DIRECTION ( 'NONE',  ( 0.5364919789714477361, 0.6444004775717706579, 0.5449076811759711036 ) ) ;
#48420 = PLANE ( 'NONE',  #30372 ) ;
#48421 = VECTOR ( 'NONE', #20985, 1000.000000000000227 ) ;
#48422 = ORIENTED_EDGE ( 'NONE', *, *, #28039, .F. ) ;
#48423 = FACE_OUTER_BOUND ( 'NONE', #15117, .T. ) ;
#48424 = DIRECTION ( 'NONE',  ( 0.007781995580012663651, 0.000000000000000000, -0.9999697198139515519 ) ) ;
#48425 = EDGE_CURVE ( 'NONE', #37378, #43993, #23180, .T. ) ;
#48426 = FACE_OUTER_BOUND ( 'NONE', #22852, .T. ) ;
#48427 = CARTESIAN_POINT ( 'NONE',  ( -23.33693525117809386, 0.000000000000000000, 5.746789908705562944 ) ) ;
#48428 = EDGE_CURVE ( 'NONE', #28121, #17110, #17692, .T. ) ;
#48429 = VECTOR ( 'NONE', #3725, 1000.000000000000227 ) ;
#48430 = ORIENTED_EDGE ( 'NONE', *, *, #7998, .F. ) ;
#48431 = DIRECTION ( 'NONE',  ( 0.005002170337468016433, -0.7660444431189770143, -0.6427681459581293666 ) ) ;
#48432 = ORIENTED_EDGE ( 'NONE', *, *, #9650, .T. ) ;
#48433 = FACE_OUTER_BOUND ( 'NONE', #11853, .T. ) ;
#48434 = CARTESIAN_POINT ( 'NONE',  ( -11.40636015113596180, 0.000000000000000000, 11.32142374880780089 ) ) ;
#48435 = VECTOR ( 'NONE', #33516, 999.9999999999998863 ) ;
#48436 = EDGE_LOOP ( 'NONE', ( #19697, #28291, #55632, #44912 ) ) ;
#48437 = EDGE_CURVE ( 'NONE', #8206, #52695, #39566, .T. ) ;
#48438 = CARTESIAN_POINT ( 'NONE',  ( -14.46888367232926420, 0.000000000000000000, 12.59025272694991315 ) ) ;
#48439 = ORIENTED_EDGE ( 'NONE', *, *, #38161, .F. ) ;
#48440 = EDGE_CURVE ( 'NONE', #32882, #43375, #52872, .T. ) ;
#48441 = VECTOR ( 'NONE', #51831, 999.9999999999998863 ) ;
#48442 = ORIENTED_EDGE ( 'NONE', *, *, #36318, .F. ) ;
#48443 = ORIENTED_EDGE ( 'NONE', *, *, #25329, .T. ) ;
#48444 = CARTESIAN_POINT ( 'NONE',  ( -14.94916102560700821, 0.000000000000000000, 2.688082935172642962 ) ) ;
#48445 = VECTOR ( 'NONE', #4156, 999.9999999999998863 ) ;
#48446 = VERTEX_POINT ( 'NONE', #26214 ) ;
#48447 = ORIENTED_EDGE ( 'NONE', *, *, #16651, .T. ) ;
#48448 = CARTESIAN_POINT ( 'NONE',  ( -12.77485720952366677, 0.000000000000000000, 8.044978861108015522 ) ) ;
#48449 = CARTESIAN_POINT ( 'NONE',  ( 2.072287782118878319, 0.000000000000000000, -2.950529333540147015 ) ) ;
#48450 = ORIENTED_EDGE ( 'NONE', *, *, #31484, .F. ) ;
#48451 = EDGE_LOOP ( 'NONE', ( #9254, #55688, #40982, #12829 ) ) ;
#48452 = CARTESIAN_POINT ( 'NONE',  ( -12.74899072797612476, 0.000000000000000000, 4.721191531788137219 ) ) ;
#48453 = EDGE_LOOP ( 'NONE', ( #54126, #18876, #56065, #4787 ) ) ;
#48454 = EDGE_LOOP ( 'NONE', ( #3017, #35449, #13121, #12657 ) ) ;
#48455 = VECTOR ( 'NONE', #27875, 999.9999999999998863 ) ;
#48456 = LINE ( 'NONE', #27427, #43788 ) ;
#48457 = PLANE ( 'NONE',  #12170 ) ;
#48458 = PLANE ( 'NONE',  #35045 ) ;
#48459 = DIRECTION ( 'NONE',  ( 0.007781995580012663651, -3.146120232559066537E-19, -0.9999697198139514409 ) ) ;
#48460 = ORIENTED_EDGE ( 'NONE', *, *, #49458, .T. ) ;
#48461 = LINE ( 'NONE', #31448, #38267 ) ;
#48462 = VECTOR ( 'NONE', #55173, 1000.000000000000000 ) ;
#48463 = ORIENTED_EDGE ( 'NONE', *, *, #27869, .F. ) ;
#48464 = LINE ( 'NONE', #18662, #39346 ) ;
#48465 = DIRECTION ( 'NONE',  ( 0.9999697198139515519, 0.000000000000000000, 0.007781995580013368816 ) ) ;
#48466 = AXIS2_PLACEMENT_3D ( 'NONE', #30252, #43573, #47859 ) ;
#48467 = CARTESIAN_POINT ( 'NONE',  ( -14.01701317841955508, 0.000000000000000000, 2.326005055450897085 ) ) ;
#48468 = DIRECTION ( 'NONE',  ( 0.005002170337468016433, -0.7660444431189770143, -0.6427681459581293666 ) ) ;
#48469 = CARTESIAN_POINT ( 'NONE',  ( 5.282343268243065104, -1.069465939554116174, -2.393143853048730119 ) ) ;
#48470 = DIRECTION ( 'NONE',  ( 0.9999697198139515519, 0.000000000000000000, 0.007781995580013368816 ) ) ;
#48471 = AXIS2_PLACEMENT_3D ( 'NONE', #46190, #24343, #42510 ) ;
#48472 = CARTESIAN_POINT ( 'NONE',  ( -17.83139810946674686, -0.1191753592594197858, 13.85674710641801788 ) ) ;
#48473 = ORIENTED_EDGE ( 'NONE', *, *, #49174, .F. ) ;
#48474 = DIRECTION ( 'NONE',  ( -0.2426528472758541499, 0.7422098413412800966, -0.6246952433987894571 ) ) ;
#48475 = VECTOR ( 'NONE', #3625, 1000.000000000000114 ) ;
#48476 = ADVANCED_FACE ( 'NONE', ( #27055 ), #40098, .F. ) ;
#48477 = FACE_OUTER_BOUND ( 'NONE', #45234, .T. ) ;
#48478 = CARTESIAN_POINT ( 'NONE',  ( -17.83139810946674686, -0.1191753592594197858, 13.85674710641801788 ) ) ;
#48479 = CARTESIAN_POINT ( 'NONE',  ( -8.409922665610809034, 0.000000000000000000, 10.23674650875856962 ) ) ;
#48480 = CARTESIAN_POINT ( 'NONE',  ( -39.57685482548858147, 8.076517251137449449, -4.968603096491658100 ) ) ;
#48481 = CARTESIAN_POINT ( 'NONE',  ( -13.24528089218730287, 4.495856970884011261, 1.683407265882337134 ) ) ;
#48482 = EDGE_CURVE ( 'NONE', #54373, #5690, #18519, .T. ) ;
#48483 = EDGE_CURVE ( 'NONE', #7363, #47810, #8913, .T. ) ;
#48484 = FACE_OUTER_BOUND ( 'NONE', #33691, .T. ) ;
#48485 = AXIS2_PLACEMENT_3D ( 'NONE', #43534, #44106, #9174 ) ;
#48486 = FACE_OUTER_BOUND ( 'NONE', #47380, .T. ) ;
#48487 = VECTOR ( 'NONE', #17698, 999.9999999999998863 ) ;
#48488 = VERTEX_POINT ( 'NONE', #35032 ) ;
#48489 = CARTESIAN_POINT ( 'NONE',  ( -11.50051463717167621, 0.000000000000000000, 7.685564019862313856 ) ) ;
#48490 = CARTESIAN_POINT ( 'NONE',  ( -10.41011832185500019, 0.000000000000000000, 2.723406815044388196 ) ) ;
#48491 = PLANE ( 'NONE',  #9178 ) ;
#48492 = CARTESIAN_POINT ( 'NONE',  ( -19.52585474275619148, 0.000000000000000000, 5.607122604862315285 ) ) ;
#48493 = CARTESIAN_POINT ( 'NONE',  ( -17.74482636761137044, -0.1191753592594197858, 3.674319602356483916 ) ) ;
#48494 = DIRECTION ( 'NONE',  ( 0.000000000000000000, 0.000000000000000000, -1.000000000000000000 ) ) ;
#48495 = CARTESIAN_POINT ( 'NONE',  ( -17.37239704199277313, -2.946525016555660237, 8.265710246709229381 ) ) ;
#48496 = AXIS2_PLACEMENT_3D ( 'NONE', #9885, #512, #22394 ) ;
#48497 = DIRECTION ( 'NONE',  ( 0.007781995580012663651, 0.000000000000000000, -0.9999697198139515519 ) ) ;
#48498 = VECTOR ( 'NONE', #27851, 1000.000000000000000 ) ;
#48499 = DIRECTION ( 'NONE',  ( 0.5364919789714477361, 0.6444004775717706579, 0.5449076811759711036 ) ) ;
#48500 = VECTOR ( 'NONE', #28414, 999.9999999999998863 ) ;
#48501 = VERTEX_POINT ( 'NONE', #14294 ) ;
#48502 = AXIS2_PLACEMENT_3D ( 'NONE', #42327, #7974, #33785 ) ;
#48503 = EDGE_CURVE ( 'NONE', #33244, #52569, #22779, .T. ) ;
#48504 = ORIENTED_EDGE ( 'NONE', *, *, #21705, .F. ) ;
#48505 = VERTEX_POINT ( 'NONE', #30489 ) ;
#48506 = AXIS2_PLACEMENT_3D ( 'NONE', #53743, #32188, #23645 ) ;
#48507 = VECTOR ( 'NONE', #16850, 999.9999999999998863 ) ;
#48508 = ORIENTED_EDGE ( 'NONE', *, *, #52903, .F. ) ;
#48509 = EDGE_CURVE ( 'NONE', #1256, #38849, #13444, .T. ) ;
#48510 = VECTOR ( 'NONE', #53643, 1000.000000000000227 ) ;
#48511 = AXIS2_PLACEMENT_3D ( 'NONE', #49286, #15669, #5861 ) ;
#48512 = ORIENTED_EDGE ( 'NONE', *, *, #51737, .F. ) ;
#48513 = CARTESIAN_POINT ( 'NONE',  ( -16.74797317661480278, 0.000000000000000000, 6.906062944538641446 ) ) ;
#48514 = ADVANCED_FACE ( 'NONE', ( #17977 ), #5209, .F. ) ;
#48515 = LINE ( 'NONE', #18123, #50285 ) ;
#48516 = AXIS2_PLACEMENT_3D ( 'NONE', #3132, #46570, #7688 ) ;
#48517 = ORIENTED_EDGE ( 'NONE', *, *, #30691, .F. ) ;
#48518 = VERTEX_POINT ( 'NONE', #18232 ) ;
#48519 = EDGE_CURVE ( 'NONE', #42240, #693, #21934, .T. ) ;
#48520 = AXIS2_PLACEMENT_3D ( 'NONE', #44314, #5416, #22727 ) ;
#48521 = VECTOR ( 'NONE', #33392, 1000.000000000000114 ) ;
#48522 = CARTESIAN_POINT ( 'NONE',  ( -69.17625094509207884, -9.022378817169743215, -7.568661514997564232 ) ) ;
#48523 = ORIENTED_EDGE ( 'NONE', *, *, #39212, .F. ) ;
#48524 = DIRECTION ( 'NONE',  ( 0.7660212471507180654, -0.6427876096865404731, 0.005961354470445141482 ) ) ;
#48525 = CARTESIAN_POINT ( 'NONE',  ( -21.47263955680318404, 0.000000000000000000, 5.022634149262071190 ) ) ;
#48526 = ORIENTED_EDGE ( 'NONE', *, *, #3032, .F. ) ;
#48527 = CARTESIAN_POINT ( 'NONE',  ( -24.27063949748155380, 0.000000000000000000, 6.308861732390097288 ) ) ;
#48528 = ORIENTED_EDGE ( 'NONE', *, *, #2244, .T. ) ;
#48529 = CARTESIAN_POINT ( 'NONE',  ( -27.06630483948590893, -0.1191753592594197858, 7.295098399573937797 ) ) ;
#48530 = CARTESIAN_POINT ( 'NONE',  ( -9.964043400434892561, 0.000000000000000000, 5.112196705653958340 ) ) ;
#48531 = VECTOR ( 'NONE', #20637, 1000.000000000000227 ) ;
#48532 = LINE ( 'NONE', #40591, #10985 ) ;
#48533 = LINE ( 'NONE', #5948, #4272 ) ;
#48534 = ORIENTED_EDGE ( 'NONE', *, *, #8873, .F. ) ;
#48535 = DIRECTION ( 'NONE',  ( 0.9999697198139515519, 0.000000000000000000, 0.007781995580013368816 ) ) ;
#48536 = CARTESIAN_POINT ( 'NONE',  ( -24.96676581047183063, 18.24370688441070953, 4.565775410814726598 ) ) ;
#48538 = VECTOR ( 'NONE', #29455, 1000.000000000000227 ) ;
#48537 = CARTESIAN_POINT ( 'NONE',  ( -17.26532721389163072, 0.000000000000000000, 13.67648636611514590 ) ) ;
#48539 = ORIENTED_EDGE ( 'NONE', *, *, #2086, .F. ) ;
#48540 = CARTESIAN_POINT ( 'NONE',  ( -14.06092696710768664, -0.1191753592594177180, 7.026977187570086159 ) ) ;
#48541 = EDGE_CURVE ( 'NONE', #41332, #18331, #31311, .T. ) ;
#48542 = EDGE_LOOP ( 'NONE', ( #25600, #26707, #13, #22891 ) ) ;
#48543 = CIRCLE ( 'NONE', #1352, 3.000000000000001332 ) ;
#48544 = EDGE_CURVE ( 'NONE', #27953, #2695, #58, .T. ) ;
#48545 = FACE_OUTER_BOUND ( 'NONE', #25836, .T. ) ;
#48546 = CARTESIAN_POINT ( 'NONE',  ( -16.56142742775368149, 0.1245042932765021287, 3.518674714925085212 ) ) ;
#48547 = CARTESIAN_POINT ( 'NONE',  ( -16.83437808062778629, -0.1191753592594196748, 5.158733200673210284 ) ) ;
#48548 = FACE_OUTER_BOUND ( 'NONE', #11676, .T. ) ;
#48549 = VECTOR ( 'NONE', #34560, 999.9999999999998863 ) ;
#48550 = DIRECTION ( 'NONE',  ( 0.007781995580012662783, 0.000000000000000000, -0.9999697198139514409 ) ) ;
#48551 = FACE_OUTER_BOUND ( 'NONE', #36377, .T. ) ;
#48552 = ADVANCED_FACE ( 'NONE', ( #35560 ), #4909, .F. ) ;
#48553 = CARTESIAN_POINT ( 'NONE',  ( 1.086233639165236964, 0.000000000000000000, 2.796443541562362078 ) ) ;
#48555 = VECTOR ( 'NONE', #25917, 1000.000000000000227 ) ;
#48554 = LINE ( 'NONE', #1402, #36559 ) ;
#48556 = VECTOR ( 'NONE', #12787, 999.9999999999998863 ) ;
#48557 = CARTESIAN_POINT ( 'NONE',  ( -14.46888367232926420, 0.000000000000000000, 12.59025272694991315 ) ) ;
#48558 = EDGE_LOOP ( 'NONE', ( #7571, #27966, #52003, #24692 ) ) ;
#48559 = LINE ( 'NONE', #36331, #30251 ) ;
#48560 = CARTESIAN_POINT ( 'NONE',  ( 2.072287782118878319, 0.000000000000000000, -2.950529333540147015 ) ) ;
#48561 = CARTESIAN_POINT ( 'NONE',  ( -17.89161118178617826, 0.000000000000000000, 8.743823238175442825 ) ) ;
#48563 = AXIS2_PLACEMENT_3D ( 'NONE', #2994, #23491, #36274 ) ;
#48562 = CARTESIAN_POINT ( 'NONE',  ( -5.750715776775079391, -5.518302702908891355, -0.9846002728345305544 ) ) ;
#48564 = VECTOR ( 'NONE', #20784, 999.9999999999998863 ) ;
#48565 = CARTESIAN_POINT ( 'NONE',  ( -19.12512386491386707, 2.067327705546508021, 4.044820755108049504 ) ) ;
#48566 = CARTESIAN_POINT ( 'NONE',  ( -16.74222506960423829, 0.000000000000000000, 6.167443538023113625 ) ) ;
#48567 = CARTESIAN_POINT ( 'NONE',  ( -19.01034150907313247, 3.038739411681508518, 3.969242270749952617 ) ) ;
#48568 = EDGE_CURVE ( 'NONE', #37070, #26836, #48640, .T. ) ;
#48569 = ORIENTED_EDGE ( 'NONE', *, *, #33563, .T. ) ;
#48570 = AXIS2_PLACEMENT_3D ( 'NONE', #29932, #51230, #33367 ) ;
#48571 = VECTOR ( 'NONE', #12724, 1000.000000000000000 ) ;
#48572 = VERTEX_POINT ( 'NONE', #30762 ) ;
#48573 = LINE ( 'NONE', #10223, #44078 ) ;
#48574 = CARTESIAN_POINT ( 'NONE',  ( -58.00000000000000711, 2.000000000000000000, 3.000000000000008438 ) ) ;
#48575 = ORIENTED_EDGE ( 'NONE', *, *, #26887, .T. ) ;
#48576 = CARTESIAN_POINT ( 'NONE',  ( -14.96915702288384153, -4.565544526780664469, 2.550185285927776935 ) ) ;
#48577 = ORIENTED_EDGE ( 'NONE', *, *, #40525, .F. ) ;
#48578 = CARTESIAN_POINT ( 'NONE',  ( -10.00813838035478298, 0.000000000000000000, 10.77830692922518452 ) ) ;
#48579 = VECTOR ( 'NONE', #5986, 1000.000000000000114 ) ;
#48580 = EDGE_LOOP ( 'NONE', ( #15408, #6664, #44739, #38923, #2439 ) ) ;
#48581 = ORIENTED_EDGE ( 'NONE', *, *, #890, .T. ) ;
#48582 = ORIENTED_EDGE ( 'NONE', *, *, #39993, .F. ) ;
#48583 = VECTOR ( 'NONE', #43831, 1000.000000000000114 ) ;
#48584 = PLANE ( 'NONE',  #42921 ) ;
#48585 = FACE_OUTER_BOUND ( 'NONE', #34147, .T. ) ;
#48586 = VECTOR ( 'NONE', #18669, 1000.000000000000000 ) ;
#48587 = FACE_OUTER_BOUND ( 'NONE', #8571, .T. ) ;
#48588 = PLANE ( 'NONE',  #29316 ) ;
#48589 = VERTEX_POINT ( 'NONE', #48330 ) ;
#48590 = ADVANCED_FACE ( 'NONE', ( #9443 ), #53187, .F. ) ;
#48591 = VECTOR ( 'NONE', #10200, 1000.000000000000227 ) ;
#48592 = EDGE_LOOP ( 'NONE', ( #51188, #19222, #6695, #39148 ) ) ;
#48593 = AXIS2_PLACEMENT_3D ( 'NONE', #8037, #42651, #3747 ) ;
#48594 = DIRECTION ( 'NONE',  ( 0.5449076811759707706, 0.6444004775717708799, -0.5364919789714476250 ) ) ;
#48595 = ORIENTED_EDGE ( 'NONE', *, *, #31565, .F. ) ;
#48596 = CARTESIAN_POINT ( 'NONE',  ( -16.79925329029790149, 0.000000000000000000, 13.49544742625427496 ) ) ;
#48597 = VECTOR ( 'NONE', #20310, 999.9999999999998863 ) ;
#48598 = ORIENTED_EDGE ( 'NONE', *, *, #22834, .T. ) ;
#48599 = DIRECTION ( 'NONE',  ( 0.007781995580012662783, 0.000000000000000000, -0.9999697198139514409 ) ) ;
#48600 = CARTESIAN_POINT ( 'NONE',  ( -9.961169346929608537, 0.000000000000000000, 4.742887002396194873 ) ) ;
#48601 = VECTOR ( 'NONE', #33889, 999.9999999999998863 ) ;
#48602 = ADVANCED_FACE ( 'NONE', ( #21678 ), #38993, .F. ) ;
#48603 = VERTEX_POINT ( 'NONE', #41973 ) ;
#48604 = AXIS2_PLACEMENT_3D ( 'NONE', #43087, #25474, #4201 ) ;
#48605 = FACE_OUTER_BOUND ( 'NONE', #36422, .T. ) ;
#48606 = ORIENTED_EDGE ( 'NONE', *, *, #47390, .T. ) ;
#48607 = ADVANCED_FACE ( 'NONE', ( #27843 ), #33213, .F. ) ;
#48608 = EDGE_CURVE ( 'NONE', #47316, #43061, #19583, .T. ) ;
#48609 = VECTOR ( 'NONE', #36996, 1000.000000000000227 ) ;
#48610 = DIRECTION ( 'NONE',  ( -0.5449076811759708816, 0.6444004775717707689, 0.5364919789714475140 ) ) ;
#48611 = VECTOR ( 'NONE', #13307, 1000.000000000000114 ) ;
#48612 = ORIENTED_EDGE ( 'NONE', *, *, #23614, .T. ) ;
#48613 = CARTESIAN_POINT ( 'NONE',  ( -18.67775241435682432, 0.000000000000000000, 4.136394454059623804 ) ) ;
#48614 = CARTESIAN_POINT ( 'NONE',  ( -24.26908309836554878, 0.000000000000000000, 6.108867788427308376 ) ) ;
#48615 = LINE ( 'NONE', #14524, #35587 ) ;
#48616 = EDGE_CURVE ( 'NONE', #56109, #42504, #23558, .T. ) ;
#48617 = ORIENTED_EDGE ( 'NONE', *, *, #12316, .F. ) ;
#48618 = PLANE ( 'NONE',  #12971 ) ;
#48619 = EDGE_CURVE ( 'NONE', #49950, #23038, #6511, .T. ) ;
#48620 = DIRECTION ( 'NONE',  ( 0.7660212471507180654, -0.6427876096865404731, 0.005961354470445141482 ) ) ;
#48621 = DIRECTION ( 'NONE',  ( 0.5364919789714477361, 0.6444004775717706579, 0.5449076811759711036 ) ) ;
#48622 = CARTESIAN_POINT ( 'NONE',  ( -56.00000000000000711, 3.800000000000001599, -1.887458608817680794 ) ) ;
#48623 = DIRECTION ( 'NONE',  ( 0.7660212471507180654, -0.6427876096865404731, 0.005961354470445141482 ) ) ;
#48624 = EDGE_CURVE ( 'NONE', #17655, #13435, #2530, .T. ) ;
#48625 = DIRECTION ( 'NONE',  ( 0.5364919789714477361, 0.6444004775717706579, 0.5449076811759711036 ) ) ;
#48626 = VECTOR ( 'NONE', #31683, 1000.000000000000227 ) ;
#48627 = DIRECTION ( 'NONE',  ( 0.007781995580012663651, -3.146120232559066537E-19, -0.9999697198139514409 ) ) ;
#48628 = ORIENTED_EDGE ( 'NONE', *, *, #18083, .T. ) ;
#48629 = DIRECTION ( 'NONE',  ( -0.005961354470445682716, -0.6427876096865404731, 0.7660212471507180654 ) ) ;
#48630 = CARTESIAN_POINT ( 'NONE',  ( -21.47419595591918906, 0.000000000000000000, 5.222628093224860102 ) ) ;
#48631 = CARTESIAN_POINT ( 'NONE',  ( -21.47263955680318404, 0.000000000000000000, 5.022634149262071190 ) ) ;
#48632 = VERTEX_POINT ( 'NONE', #45984 ) ;
#48633 = LINE ( 'NONE', #35857, #48352 ) ;
#48634 = DIRECTION ( 'NONE',  ( 0.6427681459581294776, -0.7660444431189769032, 0.005002170337467562802 ) ) ;
#48635 = VECTOR ( 'NONE', #965, 1000.000000000000227 ) ;
#48636 = ORIENTED_EDGE ( 'NONE', *, *, #9713, .T. ) ;
#48637 = ADVANCED_FACE ( 'NONE', ( #11038 ), #32905, .F. ) ;
#48638 = CARTESIAN_POINT ( 'NONE',  ( -8.568815055522351898, 0.000000000000000000, 4.953728681663013056 ) ) ;
#48639 = AXIS2_PLACEMENT_3D ( 'NONE', #27473, #2478, #2180 ) ;
#48640 = LINE ( 'NONE', #13697, #25744 ) ;
#48641 = CARTESIAN_POINT ( 'NONE',  ( -61.38973930853472893, 7.404220597074750998, -3.000000000000006661 ) ) ;
#48642 = DIRECTION ( 'NONE',  ( 0.000000000000000000, -1.000000000000000000, 0.000000000000000000 ) ) ;
#48643 = ADVANCED_FACE ( 'NONE', ( #55069 ), #15318, .F. ) ;
#48644 = ORIENTED_EDGE ( 'NONE', *, *, #5423, .F. ) ;
#48645 = AXIS2_PLACEMENT_3D ( 'NONE', #31527, #27237, #40305 ) ;
#48646 = ORIENTED_EDGE ( 'NONE', *, *, #51890, .T. ) ;
#48647 = DIRECTION ( 'NONE',  ( -0.9999697198139514409, -0.000000000000000000, -0.007781995580013368816 ) ) ;
#48648 = FACE_OUTER_BOUND ( 'NONE', #8738, .T. ) ;
#48649 = DIRECTION ( 'NONE',  ( 0.005002170337468016433, -0.7660444431189770143, -0.6427681459581293666 ) ) ;
#48650 = AXIS2_PLACEMENT_3D ( 'NONE', #847, #31797, #35786 ) ;
#48651 = CARTESIAN_POINT ( 'NONE',  ( -10.00813838035478298, 0.000000000000000000, 10.77830692922518452 ) ) ;
#48653 = DIRECTION ( 'NONE',  ( -0.5364919789714478471, 0.6444004775717705469, -0.5449076811759709926 ) ) ;
#48652 = VECTOR ( 'NONE', #24853, 1000.000000000000000 ) ;
#48654 = LINE ( 'NONE', #35049, #52129 ) ;
#48655 = ORIENTED_EDGE ( 'NONE', *, *, #14504, .F. ) ;
#48656 = DIRECTION ( 'NONE',  ( -0.7660212471507179544, -0.6427876096865405842, -0.005961354470445141482 ) ) ;
#48657 = AXIS2_PLACEMENT_3D ( 'NONE', #18976, #44806, #23514 ) ;
#48658 = CIRCLE ( 'NONE', #24168, 0.5000000000000004441 ) ;
#48659 = DIRECTION ( 'NONE',  ( -0.6427681459581293666, -0.7660444431189770143, -0.005002170337467561935 ) ) ;
#48660 = ORIENTED_EDGE ( 'NONE', *, *, #36328, .T. ) ;
#48661 = CARTESIAN_POINT ( 'NONE',  ( -29.86352658060627618, 0.000000000000000000, 8.481329010720569883 ) ) ;
#48662 = CARTESIAN_POINT ( 'NONE',  ( -24.26908309836554878, 0.000000000000000000, 6.108867788427308376 ) ) ;
#48663 = CARTESIAN_POINT ( 'NONE',  ( -16.81345671998191449, 0.000000000000000000, 3.412238694616132495 ) ) ;
#48664 = ORIENTED_EDGE ( 'NONE', *, *, #9721, .T. ) ;
#48665 = CARTESIAN_POINT ( 'NONE',  ( -26.13493519185646008, 0.000000000000000000, 7.033017491833586377 ) ) ;
#48666 = ADVANCED_FACE ( 'NONE', ( #36919 ), #28665, .F. ) ;
#48667 = ORIENTED_EDGE ( 'NONE', *, *, #9369, .T. ) ;
#48668 = AXIS2_PLACEMENT_3D ( 'NONE', #43444, #35769, #44547 ) ;
#48669 = EDGE_LOOP ( 'NONE', ( #54579, #17097, #23753, #51221 ) ) ;
#48670 = VERTEX_POINT ( 'NONE', #41695 ) ;
#48671 = VERTEX_POINT ( 'NONE', #45152 ) ;
#48672 = CARTESIAN_POINT ( 'NONE',  ( -67.14101802347384762, -8.387388012353506284, -2.442027903730112026 ) ) ;
#48673 = B_SPLINE_SURFACE_WITH_KNOTS ( 'NONE', 1, 3, ( 
 ( #41388, #27779, #50158, #45099, #25195, #55839, #46445, #46756, #47038, #2722, #8138, #21184, #42496, #42213 ),
 ( #38509, #3323, #37374, #3586, #33681, #55540, #46180, #16949, #38219, #20895, #28882, #7563, #29740, #16643 ) ),
 .UNSPECIFIED., .F., .F., .F.,
 ( 2, 2 ),
 ( 4, 2, 2, 2, 2, 2, 4 ),
 ( 0.000000000000000000, 1.000000000000000000 ),
 ( 0.000000000000000000, 0.1159099261691615840, 0.2318198523383231680, 0.4636397046766463359, 0.6954595570149695316, 0.9272794093532926718, 1.000000000000000000 ),
 .UNSPECIFIED. ) ;
#48674 = ORIENTED_EDGE ( 'NONE', *, *, #19223, .T. ) ;
#48675 = LINE ( 'NONE', #18008, #45779 ) ;
#48676 = PLANE ( 'NONE',  #5030 ) ;
#48677 = ADVANCED_FACE ( 'NONE', ( #7092 ), #50524, .F. ) ;
#48678 = VERTEX_POINT ( 'NONE', #20407 ) ;
#48679 = PLANE ( 'NONE',  #38609 ) ;
#48680 = AXIS2_PLACEMENT_3D ( 'NONE', #10379, #49568, #23982 ) ;
#48681 = ORIENTED_EDGE ( 'NONE', *, *, #45178, .T. ) ;
#48682 = CARTESIAN_POINT ( 'NONE',  ( -16.06709938707323460, 0.000000000000000000, 13.13181314741652628 ) ) ;
#48683 = ORIENTED_EDGE ( 'NONE', *, *, #16794, .F. ) ;
#48684 = EDGE_CURVE ( 'NONE', #20189, #36118, #11623, .T. ) ;
#48685 = VECTOR ( 'NONE', #2767, 999.9999999999998863 ) ;
#48686 = DIRECTION ( 'NONE',  ( 0.000000000000000000, -0.000000000000000000, -1.000000000000000000 ) ) ;
#48687 = FACE_OUTER_BOUND ( 'NONE', #14867, .T. ) ;
#48688 = CARTESIAN_POINT ( 'NONE',  ( -15.05780494465513897, 0.000000000000000000, 2.856563456659266809 ) ) ;
#48689 = DIRECTION ( 'NONE',  ( 0.007781995580012662783, 0.000000000000000000, -0.9999697198139514409 ) ) ;
#48690 = DIRECTION ( 'NONE',  ( 0.5364919789714477361, 0.6444004775717706579, 0.5449076811759711036 ) ) ;
#48691 = DIRECTION ( 'NONE',  ( 0.9999697198139515519, 0.000000000000000000, 0.007781995580013368816 ) ) ;
#48692 = ORIENTED_EDGE ( 'NONE', *, *, #25878, .F. ) ;
#48693 = ORIENTED_EDGE ( 'NONE', *, *, #57, .F. ) ;
#48694 = VECTOR ( 'NONE', #44534, 1000.000000000000114 ) ;
#48695 = EDGE_CURVE ( 'NONE', #9006, #4182, #20106, .T. ) ;
#48696 = DIRECTION ( 'NONE',  ( 0.005002170337468016433, -0.7660444431189770143, -0.6427681459581293666 ) ) ;
#48697 = LINE ( 'NONE', #1546, #43915 ) ;
#48698 = ADVANCED_FACE ( 'NONE', ( #3076 ), #37439, .F. ) ;
#48699 = DIRECTION ( 'NONE',  ( -0.005002170337468016433, -0.7660444431189770143, 0.6427681459581293666 ) ) ;
#48700 = VECTOR ( 'NONE', #24959, 999.9999999999998863 ) ;
#48701 = LINE ( 'NONE', #9805, #32183 ) ;
#48702 = ORIENTED_EDGE ( 'NONE', *, *, #50119, .F. ) ;
#48703 = DIRECTION ( 'NONE',  ( 0.000000000000000000, -0.000000000000000000, -1.000000000000000000 ) ) ;
#48704 = CARTESIAN_POINT ( 'NONE',  ( -15.88053067323646417, -0.1191753592594197858, 2.950163842912994383 ) ) ;
#48705 = ORIENTED_EDGE ( 'NONE', *, *, #39770, .T. ) ;
#48706 = LINE ( 'NONE', #44696, #15708 ) ;
#48707 = CARTESIAN_POINT ( 'NONE',  ( -9.075990533167328067, 0.000000000000000000, 10.41622904950343909 ) ) ;
#48708 = ORIENTED_EDGE ( 'NONE', *, *, #2239, .T. ) ;
#48709 = EDGE_CURVE ( 'NONE', #38932, #39994, #49402, .T. ) ;
#48710 = CARTESIAN_POINT ( 'NONE',  ( -11.34801427605302138, 0.000000000000000000, 3.824104101281660562 ) ) ;
#48711 = DIRECTION ( 'NONE',  ( 0.005002170337468016433, -0.7660444431189770143, -0.6427681459581293666 ) ) ;
#48712 = CARTESIAN_POINT ( 'NONE',  ( -12.15271748404464880, 0.000000000000000000, 1.601849296007406664 ) ) ;
#48713 = LINE ( 'NONE', #19423, #53207 ) ;
#48714 = VECTOR ( 'NONE', #20789, 999.9999999999998863 ) ;
#48715 = DIRECTION ( 'NONE',  ( -0.7660212471507179544, -0.6427876096865405842, -0.005961354470445141482 ) ) ;
#48716 = EDGE_CURVE ( 'NONE', #52840, #46588, #19282, .T. ) ;
#48717 = VERTEX_POINT ( 'NONE', #32628 ) ;
#48718 = ORIENTED_EDGE ( 'NONE', *, *, #25731, .T. ) ;
#48719 = CARTESIAN_POINT ( 'NONE',  ( -20.74129076085852930, 1.743523803501506819, 7.799362421763929909 ) ) ;
#48720 = DIRECTION ( 'NONE',  ( 0.007781995580012663651, -3.146120232559066537E-19, -0.9999697198139514409 ) ) ;
#48721 = DIRECTION ( 'NONE',  ( 0.9999697198139515519, 0.000000000000000000, 0.007781995580013368816 ) ) ;
#48722 = CARTESIAN_POINT ( 'NONE',  ( -18.66354898467281132, 0.000000000000000000, 14.21960318569776582 ) ) ;
#48723 = VECTOR ( 'NONE', #36160, 1000.000000000000227 ) ;
#48724 = LINE ( 'NONE', #35958, #29390 ) ;
#48725 = ORIENTED_EDGE ( 'NONE', *, *, #20069, .T. ) ;
#48726 = CARTESIAN_POINT ( 'NONE',  ( -13.29351286303141322, 24.98326261593401298, -3.566503301129331227 ) ) ;
#48727 = CARTESIAN_POINT ( 'NONE',  ( -32.65919192261063841, -0.1191753592594197858, 9.467565677904410393 ) ) ;
#48729 = VECTOR ( 'NONE', #46103, 1000.000000000000000 ) ;
#48728 = DIRECTION ( 'NONE',  ( 0.005002170337468016433, -0.7660444431189770143, -0.6427681459581293666 ) ) ;
#48730 = DIRECTION ( 'NONE',  ( -0.6427681459581293666, -0.7660444431189770143, -0.005002170337467561935 ) ) ;
#48731 = ORIENTED_EDGE ( 'NONE', *, *, #29913, .F. ) ;
#48732 = DIRECTION ( 'NONE',  ( 0.9999697198139515519, 0.000000000000000000, 0.007781995580013368816 ) ) ;
#48733 = EDGE_LOOP ( 'NONE', ( #943, #10801, #37326, #44391 ) ) ;
#48734 = CARTESIAN_POINT ( 'NONE',  ( 1.086233639165236964, 0.000000000000000000, 2.796443541562362078 ) ) ;
#48735 = ADVANCED_FACE ( 'NONE', ( #45680 ), #7936, .F. ) ;
#48736 = CARTESIAN_POINT ( 'NONE',  ( -19.77061338776520216, 21.24370688441071664, 4.270755533188014930 ) ) ;
#48737 = VERTEX_POINT ( 'NONE', #13018 ) ;
#48738 = VECTOR ( 'NONE', #30550, 1000.000000000000114 ) ;
#48739 = DIRECTION ( 'NONE',  ( 0.007781995580012663651, -3.146120232559066537E-19, -0.9999697198139514409 ) ) ;
#48740 = ADVANCED_FACE ( 'NONE', ( #46511 ), #20957, .F. ) ;
#48741 = ORIENTED_EDGE ( 'NONE', *, *, #6596, .T. ) ;
#48742 = ORIENTED_EDGE ( 'NONE', *, *, #42966, .F. ) ;
#48743 = VERTEX_POINT ( 'NONE', #17262 ) ;
#48744 = PLANE ( 'NONE',  #46602 ) ;
#48745 = EDGE_LOOP ( 'NONE', ( #40777, #13031, #10105, #18801 ) ) ;
#48746 = EDGE_CURVE ( 'NONE', #30407, #4309, #38279, .T. ) ;
#48747 = ORIENTED_EDGE ( 'NONE', *, *, #24056, .F. ) ;
#48748 = DIRECTION ( 'NONE',  ( -0.7886751345948130876, 0.2113248654051844977, -0.5773502691896263972 ) ) ;
#48749 = CARTESIAN_POINT ( 'NONE',  ( -13.22224978533305695, 0.000000000000000000, 5.825504729793420822 ) ) ;
#48751 = ADVANCED_FACE ( 'NONE', ( #38579 ), #16711, .F. ) ;
#48750 = EDGE_LOOP ( 'NONE', ( #16456, #38776, #23333, #46065 ) ) ;
#48752 = ADVANCED_FACE ( 'NONE', ( #55908 ), #34044, .F. ) ;
#48753 = ADVANCED_FACE ( 'NONE', ( #4239 ), #51367, .F. ) ;
#48754 = EDGE_LOOP ( 'NONE', ( #9564, #23452, #55139, #11691 ) ) ;
#48755 = LINE ( 'NONE', #26307, #28549 ) ;
#48756 = ORIENTED_EDGE ( 'NONE', *, *, #27019, .T. ) ;
#48757 = ORIENTED_EDGE ( 'NONE', *, *, #21474, .F. ) ;
#48758 = CARTESIAN_POINT ( 'NONE',  ( -13.70413100320583943, 0.000000000000000000, 8.037747037571998376 ) ) ;
#48759 = CARTESIAN_POINT ( 'NONE',  ( 2.072287782118878319, 0.000000000000000000, -2.950529333540147015 ) ) ;
#48760 = DIRECTION ( 'NONE',  ( -0.9999697198139514409, -0.000000000000000000, -0.007781995580013368816 ) ) ;
#48761 = LINE ( 'NONE', #36000, #43182 ) ;
#48762 = ORIENTED_EDGE ( 'NONE', *, *, #28084, .T. ) ;
#48763 = DIRECTION ( 'NONE',  ( 0.007781995580012663651, -3.146120232559066537E-19, -0.9999697198139514409 ) ) ;
#48764 = ORIENTED_EDGE ( 'NONE', *, *, #29169, .F. ) ;
#48765 = ADVANCED_FACE ( 'NONE', ( #29793 ), #42818, .F. ) ;
#48766 = DIRECTION ( 'NONE',  ( -0.7660212471507179544, -0.6427876096865405842, -0.005961354470445141482 ) ) ;
#48767 = EDGE_CURVE ( 'NONE', #8862, #9909, #4501, .T. ) ;
#48768 = CARTESIAN_POINT ( 'NONE',  ( -14.94760462649100496, 0.000000000000000000, 2.488088991209854051 ) ) ;
#48769 = VECTOR ( 'NONE', #53271, 999.9999999999998863 ) ;
#48770 = DIRECTION ( 'NONE',  ( 0.9999697198139515519, 0.000000000000000000, 0.007781995580013368816 ) ) ;
#48771 = CARTESIAN_POINT ( 'NONE',  ( -12.29010193814559848, 0.000000000000000000, 5.463426850071675389 ) ) ;
#48772 = FACE_OUTER_BOUND ( 'NONE', #2383, .T. ) ;
#48773 = ADVANCED_FACE ( 'NONE', ( #51899 ), #56178, .F. ) ;
#48774 = DIRECTION ( 'NONE',  ( 0.9999697198139515519, 0.000000000000000000, 0.007781995580013368816 ) ) ;
#48775 = DIRECTION ( 'NONE',  ( 0.005002170337468016433, -0.7660444431189770143, -0.6427681459581293666 ) ) ;
#48776 = ORIENTED_EDGE ( 'NONE', *, *, #52345, .F. ) ;
#48777 = CARTESIAN_POINT ( 'NONE',  ( -13.73280004183141401, 5.629170628041515023, 1.836617620612386537 ) ) ;
#48778 = ORIENTED_EDGE ( 'NONE', *, *, #48849, .T. ) ;
#48779 = EDGE_CURVE ( 'NONE', #29572, #6907, #33739, .T. ) ;
#48780 = VECTOR ( 'NONE', #34433, 1000.000000000000000 ) ;
#48781 = CARTESIAN_POINT ( 'NONE',  ( 2.072287782118878319, 0.000000000000000000, -2.950529333540147015 ) ) ;
#48782 = DIRECTION ( 'NONE',  ( 0.6427681459581294776, -0.7660444431189769032, 0.005002170337467562802 ) ) ;
#48783 = DIRECTION ( 'NONE',  ( 0.7660212471507180654, -0.6427876096865404731, 0.005961354470445141482 ) ) ;
#48784 = CARTESIAN_POINT ( 'NONE',  ( -10.47421230394850866, 0.000000000000000000, 10.95934586908605723 ) ) ;
#48785 = DIRECTION ( 'NONE',  ( 0.7660212471507180654, -0.6427876096865404731, 0.005961354470445141482 ) ) ;
#48786 = EDGE_CURVE ( 'NONE', #11442, #45245, #47360, .T. ) ;
#48787 = CARTESIAN_POINT ( 'NONE',  ( -18.19747506107908563, 0.000000000000000000, 14.03856424583689311 ) ) ;
#48788 = CARTESIAN_POINT ( 'NONE',  ( -69.91114979398979301, 1.920123671898648382E-16, -8.803577518029833016 ) ) ;
#48789 = VERTEX_POINT ( 'NONE', #47666 ) ;
#48790 = CARTESIAN_POINT ( 'NONE',  ( -17.64806569016193194, 1.419719901456505617, 3.491743278477204449 ) ) ;
#48791 = LINE ( 'NONE', #22928, #21291 ) ;
#48792 = DIRECTION ( 'NONE',  ( -0.7660212471507179544, -0.6427876096865405842, -0.005961354470445141482 ) ) ;
#48793 = CARTESIAN_POINT ( 'NONE',  ( -18.86354292863559579, 0.000000000000000000, 14.21804678658176080 ) ) ;
#48794 = CARTESIAN_POINT ( 'NONE',  ( -19.31455064293810509, -1.975113310420659740, 4.320732056343596028 ) ) ;
#48795 = CARTESIAN_POINT ( 'NONE',  ( -20.22944524586242210, 0.6102101463440047224, 4.520266361366938490 ) ) ;
#48796 = CARTESIAN_POINT ( 'NONE',  ( -10.47421230394850866, 0.000000000000000000, 10.95934586908605723 ) ) ;
#48797 = CARTESIAN_POINT ( 'NONE',  ( -68.46484361067732038, -9.679563055349168721, 6.116987600435763284 ) ) ;
#48798 = LINE ( 'NONE', #32320, #33754 ) ;
#48799 = ORIENTED_EDGE ( 'NONE', *, *, #45706, .T. ) ;
#48800 = ORIENTED_EDGE ( 'NONE', *, *, #17916, .F. ) ;
#48801 = ORIENTED_EDGE ( 'NONE', *, *, #26233, .F. ) ;
#48802 = ORIENTED_EDGE ( 'NONE', *, *, #35440, .F. ) ;
#48803 = ORIENTED_EDGE ( 'NONE', *, *, #14977, .T. ) ;
#48804 = PLANE ( 'NONE',  #7886 ) ;
#48805 = PLANE ( 'NONE',  #1322 ) ;
#48806 = EDGE_CURVE ( 'NONE', #29609, #3681, #8784, .T. ) ;
#48807 = EDGE_CURVE ( 'NONE', #20913, #48789, #5852, .T. ) ;
#48808 = VECTOR ( 'NONE', #52260, 1000.000000000000114 ) ;
#48809 = ORIENTED_EDGE ( 'NONE', *, *, #47951, .F. ) ;
#48810 = EDGE_LOOP ( 'NONE', ( #14704, #32030, #28006, #35303 ) ) ;
#48811 = EDGE_LOOP ( 'NONE', ( #22881, #5678, #28772, #18072 ) ) ;
#48812 = EDGE_CURVE ( 'NONE', #10313, #48572, #25800, .T. ) ;
#48813 = DIRECTION ( 'NONE',  ( 2.551063935260010306E-17, -4.081702296416016490E-16, 1.000000000000000000 ) ) ;
#48814 = ORIENTED_EDGE ( 'NONE', *, *, #55092, .T. ) ;
#48815 = CARTESIAN_POINT ( 'NONE',  ( 5.681647518099907757, -6.217723448642448858, 2.166220689508503661 ) ) ;
#48816 = DIRECTION ( 'NONE',  ( -0.5449076811759708816, 0.6444004775717707689, 0.5364919789714475140 ) ) ;
#48817 = ORIENTED_EDGE ( 'NONE', *, *, #21273, .T. ) ;
#48818 = DIRECTION ( 'NONE',  ( 0.007781995580012663651, -3.146120232559066537E-19, -0.9999697198139514409 ) ) ;
#48819 = ORIENTED_EDGE ( 'NONE', *, *, #13677, .T. ) ;
#48820 = DIRECTION ( 'NONE',  ( 0.000000000000000000, -1.000000000000000000, 0.000000000000000000 ) ) ;
#48821 = PLANE ( 'NONE',  #14860 ) ;
#48822 = ADVANCED_FACE ( 'NONE', ( #33477 ), #50781, .F. ) ;
#48823 = DIRECTION ( 'NONE',  ( 0.9999697198139515519, 0.000000000000000000, 0.007781995580013368816 ) ) ;
#48824 = PLANE ( 'NONE',  #23321 ) ;
#48825 = ORIENTED_EDGE ( 'NONE', *, *, #45210, .T. ) ;
#48826 = DIRECTION ( 'NONE',  ( 0.5364919789714477361, 0.6444004775717706579, 0.5449076811759711036 ) ) ;
#48827 = CARTESIAN_POINT ( 'NONE',  ( -19.52142429013490599, 0.000000000000000000, 5.037818957641762019 ) ) ;
#48828 = CARTESIAN_POINT ( 'NONE',  ( -16.46895995621009234, 0.000000000000000000, 5.061573940901824997 ) ) ;
#48829 = ORIENTED_EDGE ( 'NONE', *, *, #55303, .F. ) ;
#48830 = CARTESIAN_POINT ( 'NONE',  ( -12.23851102634202448, -0.1191753592594197858, 11.68427982808754884 ) ) ;
#48831 = ORIENTED_EDGE ( 'NONE', *, *, #27910, .F. ) ;
#48832 = EDGE_CURVE ( 'NONE', #21379, #7579, #46824, .T. ) ;
#48833 = LINE ( 'NONE', #52519, #21966 ) ;
#48834 = DIRECTION ( 'NONE',  ( 0.007781995580012663651, -3.146120232559066537E-19, -0.9999697198139514409 ) ) ;
#48835 = DIRECTION ( 'NONE',  ( 0.5364919789714477361, 0.6444004775717706579, 0.5449076811759711036 ) ) ;
#48836 = CARTESIAN_POINT ( 'NONE',  ( -9.508028664109653860, 0.000000000000000000, 6.223741727195261753 ) ) ;
#48837 = DIRECTION ( 'NONE',  ( 0.3535533905932752297, -0.6123724356957952475, 0.7071067811865462405 ) ) ;
#48838 = EDGE_CURVE ( 'NONE', #15196, #48501, #9040, .T. ) ;
#48839 = FACE_OUTER_BOUND ( 'NONE', #19050, .T. ) ;
#48840 = PLANE ( 'NONE',  #38839 ) ;
#48841 = DIRECTION ( 'NONE',  ( -0.6427681459581293666, -0.7660444431189770143, -0.005002170337467561935 ) ) ;
#48843 = EDGE_CURVE ( 'NONE', #3673, #44660, #5072, .T. ) ;
#48842 =( LENGTH_UNIT ( ) NAMED_UNIT ( * ) SI_UNIT ( .MILLI., .METRE. ) );
#48844 = LINE ( 'NONE', #27530, #41912 ) ;
#48845 = ORIENTED_EDGE ( 'NONE', *, *, #39371, .F. ) ;
#48846 = LINE ( 'NONE', #9943, #26634 ) ;
#48847 = CARTESIAN_POINT ( 'NONE',  ( -18.71591809603438961, -0.1191753592594151645, 8.098747179663282836 ) ) ;
#48849 = EDGE_CURVE ( 'NONE', #27501, #20973, #39968, .T. ) ;
#48848 = CARTESIAN_POINT ( 'NONE',  ( -15.92234860797731066, -0.1191753592594211320, 7.381823243755817110 ) ) ;
#48850 = CARTESIAN_POINT ( 'NONE',  ( -14.56888064431065821, -0.1191753592594197858, 12.58947452739191064 ) ) ;
#48851 = VECTOR ( 'NONE', #27896, 1000.000000000000000 ) ;
#48852 = ADVANCED_FACE ( 'NONE', ( #36030 ), #26343, .F. ) ;
#48853 = LINE ( 'NONE', #32627, #10097 ) ;
#48854 = CARTESIAN_POINT ( 'NONE',  ( -20.05727171210132198, 2.067327705546508021, 4.406898634829794936 ) ) ;
#48855 = CARTESIAN_POINT ( 'NONE',  ( -19.60912206198628027, -0.1191753592594197858, 4.398475361799976113 ) ) ;
#48856 = ORIENTED_EDGE ( 'NONE', *, *, #17842, .F. ) ;
#48857 = EDGE_LOOP ( 'NONE', ( #52315, #7418, #35605 ) ) ;
#48858 = CARTESIAN_POINT ( 'NONE',  ( -17.73140113748535285, 0.000000000000000000, 13.85752530597602039 ) ) ;
#48859 = CARTESIAN_POINT ( 'NONE',  ( -14.89804774976630597, 0.000000000000000000, 8.028455701383972354 ) ) ;
#48860 = VERTEX_POINT ( 'NONE', #18689 ) ;
#48861 = DIRECTION ( 'NONE',  ( 0.000000000000000000, -1.000000000000000000, 0.000000000000000000 ) ) ;
#48862 = VERTEX_POINT ( 'NONE', #27469 ) ;
#48863 = CARTESIAN_POINT ( 'NONE',  ( -12.26866590921934552, 0.000000000000000000, 2.708943167972348132 ) ) ;
#48864 = ORIENTED_EDGE ( 'NONE', *, *, #51997, .F. ) ;
#48865 = ORIENTED_EDGE ( 'NONE', *, *, #40217, .F. ) ;
#48866 = EDGE_LOOP ( 'NONE', ( #25545, #11966, #27561, #30738 ) ) ;
#48867 = CARTESIAN_POINT ( 'NONE',  ( -10.00813838035478298, 0.000000000000000000, 10.77830692922518452 ) ) ;
#48868 = CARTESIAN_POINT ( 'NONE',  ( 2.072287782118878319, 0.000000000000000000, -2.950529333540147015 ) ) ;
#48869 = CARTESIAN_POINT ( 'NONE',  ( 2.072287782118878319, 0.000000000000000000, -2.950529333540147015 ) ) ;
#48870 = EDGE_CURVE ( 'NONE', #3819, #8281, #53337, .T. ) ;
#48871 = DIRECTION ( 'NONE',  ( 0.007781995580012663651, -3.146120232559066537E-19, -0.9999697198139514409 ) ) ;
#48872 = ORIENTED_EDGE ( 'NONE', *, *, #2710, .F. ) ;
#48873 = VERTEX_POINT ( 'NONE', #22932 ) ;
#48874 = EDGE_CURVE ( 'NONE', #40198, #54534, #1053, .T. ) ;
#48875 = EDGE_CURVE ( 'NONE', #49166, #49589, #23233, .T. ) ;
#48876 = CARTESIAN_POINT ( 'NONE',  ( -24.62525945952572215, 18.15220053346460105, -4.657437592157546824 ) ) ;
#48877 = ORIENTED_EDGE ( 'NONE', *, *, #7804, .T. ) ;
#48878 = DIRECTION ( 'NONE',  ( 0.5449076811759707706, 0.6444004775717708799, -0.5364919789714476250 ) ) ;
#48879 = EDGE_LOOP ( 'NONE', ( #18566, #35642, #35127, #27220 ) ) ;
#48880 = DIRECTION ( 'NONE',  ( 0.9999697198139515519, 0.000000000000000000, 0.007781995580013368816 ) ) ;
#48881 = DIRECTION ( 'NONE',  ( 0.007781995580012662783, 0.000000000000000000, -0.9999697198139514409 ) ) ;
#48882 =( GEOMETRIC_REPRESENTATION_CONTEXT ( 3 ) GLOBAL_UNCERTAINTY_ASSIGNED_CONTEXT ( ( #33645 ) ) GLOBAL_UNIT_ASSIGNED_CONTEXT ( ( #27242, #35778, #14477 ) ) REPRESENTATION_CONTEXT ( 'NONE', 'WORKASPACE' ) );
#48883 = ORIENTED_EDGE ( 'NONE', *, *, #12634, .T. ) ;
#48884 = PLANE ( 'NONE',  #24067 ) ;
#48885 = ORIENTED_EDGE ( 'NONE', *, *, #48172, .T. ) ;
#48886 = ADVANCED_FACE ( 'NONE', ( #35723 ), #40254, .F. ) ;
#48887 = PLANE ( 'NONE',  #20912 ) ;
#48888 = VERTEX_POINT ( 'NONE', #5352 ) ;
#48889 = LINE ( 'NONE', #26445, #46677 ) ;
#48890 = PLANE ( 'NONE',  #35754 ) ;
#48891 = LINE ( 'NONE', #15100, #12846 ) ;
#48892 = ORIENTED_EDGE ( 'NONE', *, *, #34646, .F. ) ;
#48893 = CARTESIAN_POINT ( 'NONE',  ( -14.36685551739899758, -4.403642575758163424, 2.321396446839630201 ) ) ;
#48894 = DIRECTION ( 'NONE',  ( -0.7660212471507179544, -0.6427876096865405842, -0.005961354470445141482 ) ) ;
#48895 = PLANE ( 'NONE',  #50412 ) ;
#48896 = EDGE_CURVE ( 'NONE', #9006, #43180, #39717, .T. ) ;
#48897 = CARTESIAN_POINT ( 'NONE',  ( -25.20278734466900517, 0.000000000000000000, 6.670939612111840944 ) ) ;
#48898 = LINE ( 'NONE', #23058, #9785 ) ;
#48899 = CARTESIAN_POINT ( 'NONE',  ( -67.25083081275441543, -9.540336332378162254, -3.375551560942574358 ) ) ;
#48900 = VERTEX_POINT ( 'NONE', #206 ) ;
#48901 = LINE ( 'NONE', #39820, #27078 ) ;
#48902 = DIRECTION ( 'NONE',  ( -0.9999697198139514409, -0.000000000000000000, -0.007781995580013368816 ) ) ;
#48903 = FACE_OUTER_BOUND ( 'NONE', #53503, .T. ) ;
#48904 = VERTEX_POINT ( 'NONE', #47942 ) ;
#48905 = DIRECTION ( 'NONE',  ( 0.007781995580012663651, 0.000000000000000000, -0.9999697198139515519 ) ) ;
#48906 = CARTESIAN_POINT ( 'NONE',  ( -13.73672976910459909, 0.000000000000000000, 12.22661844811216270 ) ) ;
#48907 = EDGE_LOOP ( 'NONE', ( #39667, #41102, #21570 ) ) ;
#48908 = DIRECTION ( 'NONE',  ( -0.6427681459581293666, -0.7660444431189770143, -0.005002170337467561935 ) ) ;
#48909 = EDGE_CURVE ( 'NONE', #16440, #20884, #10150, .T. ) ;
#48910 = DIRECTION ( 'NONE',  ( 0.9999697198139515519, 0.000000000000000000, 0.007781995580013368816 ) ) ;
#48911 = PLANE ( 'NONE',  #24206 ) ;
#48912 = LINE ( 'NONE', #13699, #34673 ) ;
#48913 = ORIENTED_EDGE ( 'NONE', *, *, #41169, .T. ) ;
#48914 = ORIENTED_EDGE ( 'NONE', *, *, #126, .T. ) ;
#48915 = CARTESIAN_POINT ( 'NONE',  ( -12.60458797795435615, 0.000000000000000000, 11.86609696750642229 ) ) ;
#48916 = CARTESIAN_POINT ( 'NONE',  ( -9.870572735022063782, -0.1191753592594185784, 5.951591283708881797 ) ) ;
#48917 = CARTESIAN_POINT ( 'NONE',  ( -15.40103151951671734, 0.000000000000000000, 12.95233060667165681 ) ) ;
#48918 = EDGE_CURVE ( 'NONE', #33161, #27147, #43948, .T. ) ;
#48919 = DIRECTION ( 'NONE',  ( -0.005961354470445682716, -0.6427876096865404731, 0.7660212471507180654 ) ) ;
#48920 = DIRECTION ( 'NONE',  ( -0.005002170337468016433, -0.7660444431189770143, 0.6427681459581293666 ) ) ;
#48921 = ORIENTED_EDGE ( 'NONE', *, *, #37264, .F. ) ;
#48922 = CARTESIAN_POINT ( 'NONE',  ( -18.47913287522675674, -4.241740624735661491, 10.82127350084811290 ) ) ;
#48924 = EDGE_CURVE ( 'NONE', #18021, #15763, #52479, .T. ) ;
#48923 = VERTEX_POINT ( 'NONE', #52737 ) ;
#48925 = CARTESIAN_POINT ( 'NONE',  ( -8.621502653355362256, 6.299122464087065332, 0.1305108423619513736 ) ) ;
#48926 = ADVANCED_FACE ( 'NONE', ( #48194 ), #14156, .F. ) ;
#48927 = DIRECTION ( 'NONE',  ( -0.7660212471507179544, -0.6427876096865405842, -0.005961354470445141482 ) ) ;
#48928 = ORIENTED_EDGE ( 'NONE', *, *, #43668, .T. ) ;
#48929 = LINE ( 'NONE', #40115, #7494 ) ;
#48930 = EDGE_CURVE ( 'NONE', #17110, #20373, #9615, .T. ) ;
#48931 = CARTESIAN_POINT ( 'NONE',  ( -29.86274838104827367, -0.1191753592594197858, 8.381332038739175871 ) ) ;
#48932 = CARTESIAN_POINT ( 'NONE',  ( -22.36868959911851462, 19.74370688441071309, -4.433759251830043269 ) ) ;
#48933 = VERTEX_POINT ( 'NONE', #22399 ) ;
#48934 = FACE_OUTER_BOUND ( 'NONE', #28111, .T. ) ;
#48935 = ADVANCED_FACE ( 'NONE', ( #31171 ), #26936, .F. ) ;
#48936 = EDGE_LOOP ( 'NONE', ( #30569, #38076, #42593 ) ) ;
#48937 = EDGE_CURVE ( 'NONE', #33164, #22818, #5609, .T. ) ;
#48938 = VERTEX_POINT ( 'NONE', #53583 ) ;
#48939 = EDGE_LOOP ( 'NONE', ( #27852, #39256, #1830, #6341 ) ) ;
#48940 = ORIENTED_EDGE ( 'NONE', *, *, #5515, .T. ) ;
#48941 = CARTESIAN_POINT ( 'NONE',  ( -68.50231803695028532, -8.543494007632164156, -5.847034362371243965 ) ) ;
#48942 = ORIENTED_EDGE ( 'NONE', *, *, #11401, .T. ) ;
#48943 = CARTESIAN_POINT ( 'NONE',  ( 2.072287782118878319, 0.000000000000000000, -2.950529333540147015 ) ) ;
#48944 = DIRECTION ( 'NONE',  ( -0.9999697198139514409, -0.000000000000000000, -0.007781995580013368816 ) ) ;
#48945 = ADVANCED_FACE ( 'NONE', ( #50455 ), #15798, .F. ) ;
#48946 = ORIENTED_EDGE ( 'NONE', *, *, #53779, .F. ) ;
#48947 = ORIENTED_EDGE ( 'NONE', *, *, #28585, .F. ) ;
#48948 = CARTESIAN_POINT ( 'NONE',  ( -13.27065584551087163, 0.000000000000000000, 12.04557950825129176 ) ) ;
#48949 = VERTEX_POINT ( 'NONE', #54688 ) ;
#48950 = EDGE_CURVE ( 'NONE', #2679, #34678, #10979, .T. ) ;
#48951 = FACE_OUTER_BOUND ( 'NONE', #14850, .T. ) ;
#48952 = DIRECTION ( 'NONE',  ( -0.5364919789714478471, 0.6444004775717705469, -0.5449076811759709926 ) ) ;
#48953 = DIRECTION ( 'NONE',  ( 0.007781995580012663651, 0.000000000000000000, -0.9999697198139515519 ) ) ;
#48954 = CARTESIAN_POINT ( 'NONE',  ( 2.072287782118878319, 0.000000000000000000, -2.950529333540147015 ) ) ;
#48955 = CARTESIAN_POINT ( 'NONE',  ( -21.47419595591918906, 0.000000000000000000, 5.222628093224860102 ) ) ;
#48956 = SURFACE_STYLE_USAGE ( .BOTH. , #18871 ) ;
#48957 = VERTEX_POINT ( 'NONE', #33138 ) ;
#48958 = ORIENTED_EDGE ( 'NONE', *, *, #10539, .F. ) ;
#48959 = CARTESIAN_POINT ( 'NONE',  ( -6.110905869600904872, 1.712176620043476140E-14, 3.600000000000000089 ) ) ;
#48960 = DIRECTION ( 'NONE',  ( 0.5364919789714477361, 0.6444004775717706579, 0.5449076811759711036 ) ) ;
#48961 = FACE_OUTER_BOUND ( 'NONE', #51148, .T. ) ;
#48962 = CARTESIAN_POINT ( 'NONE',  ( -18.96000877805918350, -2.622721114510659035, 8.350975192617999809 ) ) ;
#48963 = ORIENTED_EDGE ( 'NONE', *, *, #53436, .F. ) ;
#48964 = CARTESIAN_POINT ( 'NONE',  ( -21.51982916103365540, 5.467268677019013978, 4.866529699019949362 ) ) ;
#48965 = CARTESIAN_POINT ( 'NONE',  ( -14.20280369269832832, 0.000000000000000000, 12.40765738797303719 ) ) ;
#48966 = ORIENTED_EDGE ( 'NONE', *, *, #50044, .T. ) ;
#48967 = FACE_OUTER_BOUND ( 'NONE', #4295, .T. ) ;
#48968 = CARTESIAN_POINT ( 'NONE',  ( -12.15193928448664629, -0.1191753592594197858, 1.501852324026012209 ) ) ;
#48969 = ORIENTED_EDGE ( 'NONE', *, *, #33660, .T. ) ;
#48970 = CARTESIAN_POINT ( 'NONE',  ( -69.11692417668358246, -9.015782624321049710, -7.493102809087829108 ) ) ;
#48971 = CARTESIAN_POINT ( 'NONE',  ( -17.83139810946674686, -0.1191753592594197858, 13.85674710641801788 ) ) ;
#48972 = ADVANCED_FACE ( 'NONE', ( #46176 ), #2174, .F. ) ;
#48973 = DIRECTION ( 'NONE',  ( -0.5364919789714478471, 0.6444004775717705469, -0.5449076811759709926 ) ) ;
#48974 = DIRECTION ( 'NONE',  ( -0.7660212471507179544, -0.6427876096865405842, -0.005961354470445141482 ) ) ;
#48975 = DIRECTION ( 'NONE',  ( -0.5364919789714478471, 0.6444004775717705469, -0.5449076811759709926 ) ) ;
#48976 = ORIENTED_EDGE ( 'NONE', *, *, #52566, .T. ) ;
#48977 = VERTEX_POINT ( 'NONE', #20046 ) ;
#48978 = LINE ( 'NONE', #22319, #19408 ) ;
#48979 = PLANE ( 'NONE',  #31315 ) ;
#48980 = DIRECTION ( 'NONE',  ( 0.7660212471507180654, -0.6427876096865404731, 0.005961354470445141482 ) ) ;
#48981 = EDGE_CURVE ( 'NONE', #12878, #21230, #7279, .T. ) ;
#48982 = CARTESIAN_POINT ( 'NONE',  ( -11.63409325785757353, 0.000000000000000000, 6.576528270728981163 ) ) ;
#48983 = CARTESIAN_POINT ( 'NONE',  ( -8.957215931586203439, 8.728699564772798070, 6.697660431825324778 ) ) ;
#48984 = VERTEX_POINT ( 'NONE', #49630 ) ;
#48985 = CARTESIAN_POINT ( 'NONE',  ( -13.09680306462247046, 25.09683307099765770, -3.525414222879889259 ) ) ;
#48986 = CARTESIAN_POINT ( 'NONE',  ( -24.27063949748155380, 0.000000000000000000, 6.308861732390097288 ) ) ;
#48987 = EDGE_CURVE ( 'NONE', #18068, #42908, #12155, .T. ) ;
#48988 = VECTOR ( 'NONE', #34315, 999.9999999999998863 ) ;
#48989 = CARTESIAN_POINT ( 'NONE',  ( -22.40634380310664397, 0.000000000000000000, 5.584705972946605534 ) ) ;
#48990 = DIRECTION ( 'NONE',  ( -0.6427681459581293666, -0.7660444431189770143, -0.005002170337467561935 ) ) ;
#48991 = ORIENTED_EDGE ( 'NONE', *, *, #17194, .T. ) ;
#48992 = CARTESIAN_POINT ( 'NONE',  ( -11.67244013076689946, 0.000000000000000000, 11.50401908778467863 ) ) ;
#48993 = ORIENTED_EDGE ( 'NONE', *, *, #43247, .F. ) ;
#48994 = LINE ( 'NONE', #48734, #19587 ) ;
#48995 = DIRECTION ( 'NONE',  ( -0.5449076811759708816, 0.6444004775717707689, 0.5364919789714475140 ) ) ;
#48996 = EDGE_LOOP ( 'NONE', ( #51929, #42933, #9851, #13448 ) ) ;
#48997 = LINE ( 'NONE', #27143, #16341 ) ;
#48998 = EDGE_CURVE ( 'NONE', #41994, #16631, #40560, .T. ) ;
#48999 = ORIENTED_EDGE ( 'NONE', *, *, #21094, .T. ) ;
#49000 = ADVANCED_FACE ( 'NONE', ( #32836 ), #54163, .F. ) ;
#49001 = ORIENTED_EDGE ( 'NONE', *, *, #29648, .T. ) ;
#49002 = ORIENTED_EDGE ( 'NONE', *, *, #8092, .T. ) ;
#49003 = CARTESIAN_POINT ( 'NONE',  ( -13.94578152804187710, 0.000000000000000000, 5.081209898857876439 ) ) ;
#49004 = VERTEX_POINT ( 'NONE', #49335 ) ;
#49005 = ORIENTED_EDGE ( 'NONE', *, *, #49440, .T. ) ;
#49006 = LINE ( 'NONE', #14932, #2995 ) ;
#49007 = DIRECTION ( 'NONE',  ( -0.7660212471507179544, -0.6427876096865405842, -0.005961354470445141482 ) ) ;
#49008 = ORIENTED_EDGE ( 'NONE', *, *, #40746, .F. ) ;
#49009 = ADVANCED_FACE ( 'NONE', ( #41383 ), #2474, .F. ) ;
#49010 = ORIENTED_EDGE ( 'NONE', *, *, #11307, .F. ) ;
#49011 = LINE ( 'NONE', #44749, #12260 ) ;
#49012 = VERTEX_POINT ( 'NONE', #27774 ) ;
#49013 = VERTEX_POINT ( 'NONE', #45095 ) ;
#49014 = EDGE_CURVE ( 'NONE', #44514, #40957, #19507, .T. ) ;
#49015 = CARTESIAN_POINT ( 'NONE',  ( -28.93060053386082231, -0.1191753592594197858, 8.019254159017428663 ) ) ;
#49016 = PLANE ( 'NONE',  #2185 ) ;
#49017 = CARTESIAN_POINT ( 'NONE',  ( -26.13337879274045505, 0.000000000000000000, 6.833023547870798353 ) ) ;
#49018 = CARTESIAN_POINT ( 'NONE',  ( -9.342070512798265725, 0.000000000000000000, 10.59882438848031505 ) ) ;
#49019 = ORIENTED_EDGE ( 'NONE', *, *, #39929, .F. ) ;
#49020 = DIRECTION ( 'NONE',  ( 0.7660212471507180654, -0.6427876096865404731, 0.005961354470445141482 ) ) ;
#49021 = ORIENTED_EDGE ( 'NONE', *, *, #7854, .T. ) ;
#49022 = DIRECTION ( 'NONE',  ( -0.6427681459581293666, -0.7660444431189770143, -0.005002170337467561935 ) ) ;
#49023 = AXIS2_PLACEMENT_3D ( 'NONE', #28151, #10281, #49473 ) ;
#49024 = LINE ( 'NONE', #10124, #53288 ) ;
#49025 = CARTESIAN_POINT ( 'NONE',  ( -67.79584355022304010, 0.1329320821914128370, -3.347029521210270531 ) ) ;
#49026 = FACE_OUTER_BOUND ( 'NONE', #9697, .T. ) ;
#49027 = DIRECTION ( 'NONE',  ( -0.05705673239519650636, 0.9983709377222390602, 2.351258244848514932E-16 ) ) ;
#49028 = PLANE ( 'NONE',  #10497 ) ;
#49029 = VERTEX_POINT ( 'NONE', #41082 ) ;
#49030 = CARTESIAN_POINT ( 'NONE',  ( -12.07861178016168502, 0.000000000000000000, 3.987744436156619887 ) ) ;
#49031 = ORIENTED_EDGE ( 'NONE', *, *, #17428, .F. ) ;
#49032 = LINE ( 'NONE', #5893, #42838 ) ;
#49033 = CARTESIAN_POINT ( 'NONE',  ( -18.33612970409028264, 0.000000000000000000, 6.155039403603081105 ) ) ;
#49034 = PLANE ( 'NONE',  #50796 ) ;
#49035 = EDGE_CURVE ( 'NONE', #17943, #45757, #40817, .T. ) ;
#49036 = CARTESIAN_POINT ( 'NONE',  ( -25.20123094555300369, 0.000000000000000000, 6.470945668149052032 ) ) ;
#49037 = DIRECTION ( 'NONE',  ( 0.6427681459581294776, -0.7660444431189769032, 0.005002170337467562802 ) ) ;
#49038 = CARTESIAN_POINT ( 'NONE',  ( -69.75862673655984736, 5.509042946743876566E-16, 8.593930712158172724 ) ) ;
#49039 = EDGE_CURVE ( 'NONE', #18181, #54123, #11262, .T. ) ;
#49040 = EDGE_LOOP ( 'NONE', ( #25375, #51838, #35394, #50740 ) ) ;
#49041 = EDGE_CURVE ( 'NONE', #18842, #32386, #36549, .T. ) ;
#49042 = DIRECTION ( 'NONE',  ( -0.005961354470445682716, -0.6427876096865404731, 0.7660212471507180654 ) ) ;
#49043 = DIRECTION ( 'NONE',  ( -0.7660212471507179544, -0.6427876096865405842, -0.005961354470445141482 ) ) ;
#49044 = PLANE ( 'NONE',  #41784 ) ;
#49045 = ADVANCED_FACE ( 'NONE', ( #14979 ), #45344, .F. ) ;
#49046 = EDGE_CURVE ( 'NONE', #9899, #15809, #54411, .T. ) ;
#49047 = EDGE_CURVE ( 'NONE', #24514, #13246, #50153, .T. ) ;
#49048 = AXIS2_PLACEMENT_3D ( 'NONE', #3668, #46544, #51399 ) ;
#49049 = CARTESIAN_POINT ( 'NONE',  ( -10.47421230394850866, 0.000000000000000000, 10.95934586908605723 ) ) ;
#49050 = CARTESIAN_POINT ( 'NONE',  ( -16.81345671998191449, 0.000000000000000000, 3.412238694616132495 ) ) ;
#49051 = CARTESIAN_POINT ( 'NONE',  ( -15.87975247367846166, 0.000000000000000000, 2.850166870931599927 ) ) ;
#49052 = DIRECTION ( 'NONE',  ( 0.007781995580012663651, 0.000000000000000000, -0.9999697198139515519 ) ) ;
#49053 = DIRECTION ( 'NONE',  ( 0.005002170337468016433, -0.7660444431189770143, -0.6427681459581293666 ) ) ;
#49054 = LINE ( 'NONE', #19795, #6566 ) ;
#49055 = EDGE_LOOP ( 'NONE', ( #46501, #20098, #52005, #37244 ) ) ;
#49056 = VECTOR ( 'NONE', #45438, 1000.000000000000227 ) ;
#49057 = EDGE_CURVE ( 'NONE', #33913, #24475, #47290, .T. ) ;
#49058 = AXIS2_PLACEMENT_3D ( 'NONE', #32310, #48792, #14430 ) ;
#49059 = ADVANCED_FACE ( 'NONE', ( #16349 ), #20890, .F. ) ;
#49060 = ORIENTED_EDGE ( 'NONE', *, *, #5906, .F. ) ;
#49061 = ORIENTED_EDGE ( 'NONE', *, *, #28706, .T. ) ;
#49062 = ORIENTED_EDGE ( 'NONE', *, *, #53812, .T. ) ;
#49063 = ADVANCED_FACE ( 'NONE', ( #55001 ), #29429, .F. ) ;
#49064 = EDGE_LOOP ( 'NONE', ( #2074, #43070, #25569, #17738 ) ) ;
#49065 = CARTESIAN_POINT ( 'NONE',  ( -15.87975247367846166, 0.000000000000000000, 2.850166870931599927 ) ) ;
#49066 = DIRECTION ( 'NONE',  ( -0.005961354470445682716, -0.6427876096865404731, 0.7660212471507180654 ) ) ;
#49067 = ADVANCED_FACE ( 'NONE', ( #4160 ), #37677, .F. ) ;
#49068 = VERTEX_POINT ( 'NONE', #51573 ) ;
#49069 = ORIENTED_EDGE ( 'NONE', *, *, #9891, .F. ) ;
#49070 = ORIENTED_EDGE ( 'NONE', *, *, #9048, .T. ) ;
#49071 = CARTESIAN_POINT ( 'NONE',  ( -65.95191306736235504, -9.257581959793618864, -4.848827299324492301 ) ) ;
#49072 = DIRECTION ( 'NONE',  ( -0.9983709377222390602, -0.05705673239519638146, 0.000000000000000000 ) ) ;
#49073 = PLANE ( 'NONE',  #44016 ) ;
#49074 = ORIENTED_EDGE ( 'NONE', *, *, #30660, .F. ) ;
#49075 = FACE_OUTER_BOUND ( 'NONE', #27036, .T. ) ;
#49076 = ORIENTED_EDGE ( 'NONE', *, *, #26905, .F. ) ;
#49077 = VECTOR ( 'NONE', #52735, 999.9999999999998863 ) ;
#49078 = AXIS2_PLACEMENT_3D ( 'NONE', #1081, #32046, #44530 ) ;
#49079 = CARTESIAN_POINT ( 'NONE',  ( -13.50701111274833011, 0.000000000000000000, 8.408613139945765980 ) ) ;
#49080 = CARTESIAN_POINT ( 'NONE',  ( -27.99767448711536133, 0.000000000000000000, 7.557179307314289218 ) ) ;
#49081 = CARTESIAN_POINT ( 'NONE',  ( -15.89855235162775848, 0.4483081953215033444, 2.843166003391808694 ) ) ;
#49082 = CARTESIAN_POINT ( 'NONE',  ( -14.86887539286270687, -2.784623065533160524, 2.568053214010371565 ) ) ;
#49083 = DIRECTION ( 'NONE',  ( -0.6427681459581293666, -0.7660444431189770143, -0.005002170337467561935 ) ) ;
#49084 = CARTESIAN_POINT ( 'NONE',  ( -25.83279121425626812, 17.74370688441070953, 4.604227610039242968 ) ) ;
#49085 = DIRECTION ( 'NONE',  ( 0.6427681459581294776, -0.7660444431189769032, 0.005002170337467562802 ) ) ;
#49086 = ORIENTED_EDGE ( 'NONE', *, *, #37563, .T. ) ;
#49087 = DIRECTION ( 'NONE',  ( 0.9999697198139515519, 0.000000000000000000, 0.007781995580013368816 ) ) ;
#49088 = VERTEX_POINT ( 'NONE', #38214 ) ;
#49089 = FACE_OUTER_BOUND ( 'NONE', #2457, .T. ) ;
#49090 = DIRECTION ( 'NONE',  ( 0.007781995580012662783, 0.000000000000000000, -0.9999697198139514409 ) ) ;
#49091 = CARTESIAN_POINT ( 'NONE',  ( -13.21650167832249245, 0.000000000000000000, 5.086885323277891224 ) ) ;
#49092 = DIRECTION ( 'NONE',  ( 0.8660254037844380415, 0.5000000000000011102, 0.000000000000000000 ) ) ;
#49093 = ADVANCED_FACE ( 'NONE', ( #8400 ), #50723, .F. ) ;
#49094 = LINE ( 'NONE', #39758, #14155 ) ;
#49095 = CARTESIAN_POINT ( 'NONE',  ( 1.086233639165236964, 0.000000000000000000, 2.796443541562362078 ) ) ;
#49096 = CARTESIAN_POINT ( 'NONE',  ( -24.96676581047183063, 18.24370688441070953, -4.657437592157546824 ) ) ;
#49097 = VECTOR ( 'NONE', #23522, 1000.000000000000227 ) ;
#49098 = DIRECTION ( 'NONE',  ( -0.5364919789714478471, 0.6444004775717705469, -0.5449076811759709926 ) ) ;
#49099 = FILL_AREA_STYLE_COLOUR ( '', #24385 ) ;
#49100 = CARTESIAN_POINT ( 'NONE',  ( -13.27065584551087163, 0.000000000000000000, 12.04557950825129176 ) ) ;
#49101 = EDGE_LOOP ( 'NONE', ( #37390, #38239, #18552, #54939 ) ) ;
#49102 = CARTESIAN_POINT ( 'NONE',  ( -13.00369386594929288, 0.000000000000000000, 3.441887150067862056 ) ) ;
#49103 = CARTESIAN_POINT ( 'NONE',  ( -15.78652251423055830, -5.536956232915666298, 2.836684681291425925 ) ) ;
#49104 = PLANE ( 'NONE',  #20961 ) ;
#49105 = EDGE_CURVE ( 'NONE', #2279, #10471, #56116, .T. ) ;
#49106 = CARTESIAN_POINT ( 'NONE',  ( -29.86274838104827367, -0.1191753592594197858, 8.381332038739175871 ) ) ;
#49107 = ADVANCED_FACE ( 'NONE', ( #25190 ), #38805, .F. ) ;
#49108 = EDGE_CURVE ( 'NONE', #42922, #18997, #47591, .T. ) ;
#49109 = PLANE ( 'NONE',  #20937 ) ;
#49110 = ADVANCED_FACE ( 'NONE', ( #43051 ), #46442, .F. ) ;
#49111 = DIRECTION ( 'NONE',  ( 0.007781995580012663651, -3.146120232559066537E-19, -0.9999697198139514409 ) ) ;
#49112 = VERTEX_POINT ( 'NONE', #17202 ) ;
#49113 = ORIENTED_EDGE ( 'NONE', *, *, #37628, .T. ) ;
#49114 = DIRECTION ( 'NONE',  ( 0.007781995580012662783, 0.000000000000000000, -0.9999697198139514409 ) ) ;
#49115 = PLANE ( 'NONE',  #1438 ) ;
#49116 = VECTOR ( 'NONE', #53582, 999.9999999999998863 ) ;
#49117 = VECTOR ( 'NONE', #19116, 999.9999999999998863 ) ;
#49118 = EDGE_LOOP ( 'NONE', ( #2379, #54231, #37460, #2418 ) ) ;
#49119 = DIRECTION ( 'NONE',  ( 0.005002170337468016433, -0.7660444431189770143, -0.6427681459581293666 ) ) ;
#49120 = ORIENTED_EDGE ( 'NONE', *, *, #13668, .F. ) ;
#49121 = CARTESIAN_POINT ( 'NONE',  ( -18.67697421479882181, -0.1191753592594197858, 4.036397482078229793 ) ) ;
#49122 = EDGE_CURVE ( 'NONE', #50938, #47628, #21486, .T. ) ;
#49123 = ORIENTED_EDGE ( 'NONE', *, *, #51011, .T. ) ;
#49124 = ORIENTED_EDGE ( 'NONE', *, *, #10122, .T. ) ;
#49125 = VERTEX_POINT ( 'NONE', #16944 ) ;
#49126 = EDGE_CURVE ( 'NONE', #49857, #39974, #47033, .T. ) ;
#49127 = DIRECTION ( 'NONE',  ( 0.5449076811759707706, 0.6444004775717708799, -0.5364919789714476250 ) ) ;
#49128 = DIRECTION ( 'NONE',  ( 0.000000000000000000, -0.000000000000000000, -1.000000000000000000 ) ) ;
#49129 = DIRECTION ( 'NONE',  ( 0.000000000000000000, -0.000000000000000000, -1.000000000000000000 ) ) ;
#49130 = EDGE_CURVE ( 'NONE', #48024, #44458, #55535, .T. ) ;
#49131 = CARTESIAN_POINT ( 'NONE',  ( -19.60990026154428278, 0.000000000000000000, 4.498472333781370125 ) ) ;
#49132 = ORIENTED_EDGE ( 'NONE', *, *, #48083, .T. ) ;
#49133 = VECTOR ( 'NONE', #39099, 1000.000000000000114 ) ;
#49134 = ORIENTED_EDGE ( 'NONE', *, *, #31038, .F. ) ;
#49135 = EDGE_CURVE ( 'NONE', #53347, #46741, #24589, .T. ) ;
#49136 = VECTOR ( 'NONE', #7448, 1000.000000000000227 ) ;
#49137 = CARTESIAN_POINT ( 'NONE',  ( -21.47419595591918906, 0.000000000000000000, 5.222628093224860102 ) ) ;
#49138 = ORIENTED_EDGE ( 'NONE', *, *, #46332, .T. ) ;
#49139 = DIRECTION ( 'NONE',  ( 0.9999697198139515519, 0.000000000000000000, 0.007781995580013368816 ) ) ;
#49140 = EDGE_LOOP ( 'NONE', ( #35214, #12084, #22519, #16306 ) ) ;
#49141 = DIRECTION ( 'NONE',  ( -0.5364919789714478471, 0.6444004775717705469, -0.5449076811759709926 ) ) ;
#49142 = DIRECTION ( 'NONE',  ( 0.000000000000000000, -0.000000000000000000, -1.000000000000000000 ) ) ;
#49143 = ORIENTED_EDGE ( 'NONE', *, *, #31330, .T. ) ;
#49144 = CARTESIAN_POINT ( 'NONE',  ( -17.73140113748535285, 0.000000000000000000, 13.85752530597602039 ) ) ;
#49145 = ORIENTED_EDGE ( 'NONE', *, *, #31173, .F. ) ;
#49146 = DIRECTION ( 'NONE',  ( 0.000000000000000000, -1.000000000000000000, 0.000000000000000000 ) ) ;
#49147 = ORIENTED_EDGE ( 'NONE', *, *, #17132, .T. ) ;
#49148 = CARTESIAN_POINT ( 'NONE',  ( -29.86352658060627618, 0.000000000000000000, 8.481329010720569883 ) ) ;
#49149 = LINE ( 'NONE', #27585, #13982 ) ;
#49150 = CARTESIAN_POINT ( 'NONE',  ( -22.09649345868086812, -4.727446477803164626, 5.313519283068141696 ) ) ;
#49151 = EDGE_LOOP ( 'NONE', ( #21578, #3745, #9724, #18312 ) ) ;
#49152 = CIRCLE ( 'NONE', #39185, 2.125000000000000000 ) ;
#49153 = AXIS2_PLACEMENT_3D ( 'NONE', #42592, #54512, #3425 ) ;
#49154 = CARTESIAN_POINT ( 'NONE',  ( -18.60652076397914811, 0.000000000000000000, 6.891599297466603602 ) ) ;
#49155 = CARTESIAN_POINT ( 'NONE',  ( -22.78182334992371594, 5.305366725996514710, 5.361896619375292161 ) ) ;
#49156 = DIRECTION ( 'NONE',  ( 0.005961354470445682716, -0.6427876096865404731, -0.7660212471507180654 ) ) ;
#49157 = DIRECTION ( 'NONE',  ( 0.005002170337468016433, -0.7660444431189770143, -0.6427681459581293666 ) ) ;
#49158 = FACE_OUTER_BOUND ( 'NONE', #36122, .T. ) ;
#49159 = CARTESIAN_POINT ( 'NONE',  ( -14.69670185910160143, -4.241740624735665044, 2.454685487473226679 ) ) ;
#49160 = CARTESIAN_POINT ( 'NONE',  ( -66.00830372752703568, -11.27715573706296404, -6.184885810267199524 ) ) ;
#49161 = AXIS2_PLACEMENT_3D ( 'NONE', #36670, #1995, #32671 ) ;
#49162 = ORIENTED_EDGE ( 'NONE', *, *, #37010, .T. ) ;
#49163 = DIRECTION ( 'NONE',  ( 0.007781995580012662783, 0.000000000000000000, -0.9999697198139514409 ) ) ;
#49164 = CARTESIAN_POINT ( 'NONE',  ( -61.38973930853472893, 7.404220597074750998, -3.000000000000006661 ) ) ;
#49165 = CARTESIAN_POINT ( 'NONE',  ( -67.13867486860780787, -0.6008876313341391384, 1.704803601115378431 ) ) ;
#49166 = VERTEX_POINT ( 'NONE', #20336 ) ;
#49167 = LINE ( 'NONE', #36683, #53785 ) ;
#49168 = LINE ( 'NONE', #11400, #14572 ) ;
#49169 = ORIENTED_EDGE ( 'NONE', *, *, #397, .F. ) ;
#49170 = EDGE_CURVE ( 'NONE', #48176, #6556, #7559, .T. ) ;
#49171 = LINE ( 'NONE', #45464, #30405 ) ;
#49172 = PRESENTATION_LAYER_ASSIGNMENT (  '', '', ( #31960 ) ) ;
#49173 = EDGE_CURVE ( 'NONE', #21011, #55542, #20641, .T. ) ;
#49174 = EDGE_CURVE ( 'NONE', #38344, #25308, #18612, .T. ) ;
#49175 = CARTESIAN_POINT ( 'NONE',  ( -15.56870600992515108, 0.6102101463440035012, 2.709876962758211771 ) ) ;
#49176 = DIRECTION ( 'NONE',  ( 0.000000000000000000, -1.000000000000000000, 0.000000000000000000 ) ) ;
#49177 = VERTEX_POINT ( 'NONE', #35649 ) ;
#49178 = ORIENTED_EDGE ( 'NONE', *, *, #33640, .F. ) ;
#49179 = LINE ( 'NONE', #54012, #35020 ) ;
#49180 = CARTESIAN_POINT ( 'NONE',  ( -65.33751984935661028, 2.000000000000018652, -1.324960789524834315 ) ) ;
#49181 = DIRECTION ( 'NONE',  ( -0.005961354470445682716, -0.6427876096865404731, 0.7660212471507180654 ) ) ;
#49182 = CARTESIAN_POINT ( 'NONE',  ( -16.81267852042391198, -0.1191753592594197858, 3.312241722634738039 ) ) ;
#49183 = EDGE_LOOP ( 'NONE', ( #47112, #49138, #43305, #23552 ) ) ;
#49184 = DIRECTION ( 'NONE',  ( 0.007781995580012663651, -3.146120232559066537E-19, -0.9999697198139514409 ) ) ;
#49185 = VECTOR ( 'NONE', #23147, 1000.000000000000227 ) ;
#49186 = ORIENTED_EDGE ( 'NONE', *, *, #8094, .T. ) ;
#49187 = DIRECTION ( 'NONE',  ( 0.000000000000000000, 0.000000000000000000, 1.000000000000000000 ) ) ;
#49188 = DIRECTION ( 'NONE',  ( 0.7660212471507180654, -0.6427876096865404731, 0.005961354470445141482 ) ) ;
#49189 = ORIENTED_EDGE ( 'NONE', *, *, #19798, .T. ) ;
#49190 = DIRECTION ( 'NONE',  ( 0.005961354470445682716, -0.6427876096865404731, -0.7660212471507180654 ) ) ;
#49191 = AXIS2_PLACEMENT_3D ( 'NONE', #8663, #15450, #41582 ) ;
#49192 = CARTESIAN_POINT ( 'NONE',  ( -11.73774248290225408, -0.1191753592594185784, 7.045056746410134352 ) ) ;
#49193 = PLANE ( 'NONE',  #25775 ) ;
#49194 = ORIENTED_EDGE ( 'NONE', *, *, #22506, .F. ) ;
#49195 = VECTOR ( 'NONE', #37679, 999.9999999999998863 ) ;
#49196 = VECTOR ( 'NONE', #47644, 1000.000000000000227 ) ;
#49197 = CARTESIAN_POINT ( 'NONE',  ( -15.12932141704740197, -3.594132820645660420, 8.457258234613435732 ) ) ;
#49198 = ORIENTED_EDGE ( 'NONE', *, *, #22764, .F. ) ;
#49199 = EDGE_CURVE ( 'NONE', #8011, #51712, #13514, .T. ) ;
#49200 = ORIENTED_EDGE ( 'NONE', *, *, #14407, .F. ) ;
#49201 = VECTOR ( 'NONE', #216, 999.9999999999998863 ) ;
#49202 = ORIENTED_EDGE ( 'NONE', *, *, #46659, .F. ) ;
#49203 = CARTESIAN_POINT ( 'NONE',  ( -13.73672976910459909, 0.000000000000000000, 12.22661844811216270 ) ) ;
#49204 = AXIS2_PLACEMENT_3D ( 'NONE', #41136, #19264, #54743 ) ;
#49205 = EDGE_CURVE ( 'NONE', #43426, #55768, #26857, .T. ) ;
#49206 = VERTEX_POINT ( 'NONE', #44180 ) ;
#49207 = DIRECTION ( 'NONE',  ( 0.5449076811759707706, 0.6444004775717708799, -0.5364919789714476250 ) ) ;
#49208 = EDGE_CURVE ( 'NONE', #16314, #29707, #34807, .T. ) ;
#49209 = VERTEX_POINT ( 'NONE', #40182 ) ;
#49210 = DIRECTION ( 'NONE',  ( 0.6427681459581294776, -0.7660444431189769032, 0.005002170337467562802 ) ) ;
#49211 = DIRECTION ( 'NONE',  ( 0.005961354470445682716, -0.6427876096865404731, -0.7660212471507180654 ) ) ;
#49212 = ORIENTED_EDGE ( 'NONE', *, *, #17842, .T. ) ;
#49213 = EDGE_CURVE ( 'NONE', #35002, #8314, #52418, .T. ) ;
#49215 = AXIS2_PLACEMENT_3D ( 'NONE', #34020, #29477, #46797 ) ;
#49214 = DIRECTION ( 'NONE',  ( 0.6427681459581294776, -0.7660444431189769032, 0.005002170337467562802 ) ) ;
#49216 = ORIENTED_EDGE ( 'NONE', *, *, #14912, .T. ) ;
#49217 = AXIS2_PLACEMENT_3D ( 'NONE', #34144, #38683, #38951 ) ;
#49218 = FACE_OUTER_BOUND ( 'NONE', #51539, .T. ) ;
#49219 = CARTESIAN_POINT ( 'NONE',  ( -11.20636620717317378, 0.000000000000000000, 11.32298014792380414 ) ) ;
#49220 = CARTESIAN_POINT ( 'NONE',  ( -6.646477795989845561, 6.490377269657392922, 5.800091266962301262 ) ) ;
#49221 = DIRECTION ( 'NONE',  ( 0.5449076811759707706, 0.6444004775717708799, -0.5364919789714476250 ) ) ;
#49222 = CARTESIAN_POINT ( 'NONE',  ( -21.93567689722629765, 19.99370688441071309, 4.408989160011352659 ) ) ;
#49223 = LINE ( 'NONE', #10048, #16480 ) ;
#49224 = LINE ( 'NONE', #18577, #3891 ) ;
#49225 = ORIENTED_EDGE ( 'NONE', *, *, #33533, .T. ) ;
#49226 = AXIS2_PLACEMENT_3D ( 'NONE', #45315, #20300, #3273 ) ;
#49227 = ORIENTED_EDGE ( 'NONE', *, *, #5359, .F. ) ;
#49228 = FACE_OUTER_BOUND ( 'NONE', #10934, .T. ) ;
#49229 = FACE_OUTER_BOUND ( 'NONE', #31888, .T. ) ;
#49230 = VECTOR ( 'NONE', #12797, 999.9999999999998863 ) ;
#49231 = DIRECTION ( 'NONE',  ( -0.9999697198139514409, -0.000000000000000000, -0.007781995580013368816 ) ) ;
#49232 = CYLINDRICAL_SURFACE ( 'NONE', #44905, 2.125000000000000000 ) ;
#49233 = ORIENTED_EDGE ( 'NONE', *, *, #52873, .T. ) ;
#49234 = CARTESIAN_POINT ( 'NONE',  ( -9.342070512798265725, 0.000000000000000000, 10.59882438848031505 ) ) ;
#49235 = CARTESIAN_POINT ( 'NONE',  ( -14.14002736499410062, 0.000000000000000000, 4.341034093226343593 ) ) ;
#49236 = ORIENTED_EDGE ( 'NONE', *, *, #40650, .F. ) ;
#49238 = DIRECTION ( 'NONE',  ( -0.6427681459581293666, -0.7660444431189770143, -0.005002170337467561935 ) ) ;
#49237 = VECTOR ( 'NONE', #3093, 999.9999999999998863 ) ;
#49239 = EDGE_CURVE ( 'NONE', #19103, #904, #39065, .T. ) ;
#49240 = LINE ( 'NONE', #19415, #38576 ) ;
#49241 = ORIENTED_EDGE ( 'NONE', *, *, #13460, .T. ) ;
#49242 = VECTOR ( 'NONE', #11599, 1000.000000000000114 ) ;
#49243 = VECTOR ( 'NONE', #22304, 999.9999999999998863 ) ;
#49244 = CARTESIAN_POINT ( 'NONE',  ( -66.83458874347479650, -8.753654600338279579, -2.670129092015951944 ) ) ;
#49245 = LINE ( 'NONE', #18295, #43263 ) ;
#49246 = LINE ( 'NONE', #15434, #46774 ) ;
#49247 = EDGE_CURVE ( 'NONE', #485, #2953, #48724, .T. ) ;
#49248 = EDGE_CURVE ( 'NONE', #44511, #12432, #9825, .T. ) ;
#49249 = DIRECTION ( 'NONE',  ( 0.007781995580012663651, -3.146120232559066537E-19, -0.9999697198139514409 ) ) ;
#49250 = DIRECTION ( 'NONE',  ( 0.005002170337468016433, -0.7660444431189770143, -0.6427681459581293666 ) ) ;
#49251 = ORIENTED_EDGE ( 'NONE', *, *, #16702, .F. ) ;
#49252 = AXIS2_PLACEMENT_3D ( 'NONE', #13177, #25972, #47232 ) ;
#49253 = VECTOR ( 'NONE', #45080, 999.9999999999998863 ) ;
#49254 = ORIENTED_EDGE ( 'NONE', *, *, #44272, .T. ) ;
#49255 = CARTESIAN_POINT ( 'NONE',  ( -29.86197018149027116, 0.000000000000000000, 8.281335066757780083 ) ) ;
#49256 = CARTESIAN_POINT ( 'NONE',  ( -23.23471098716119698, 19.24370920290025566, -4.480780584866845828 ) ) ;
#49257 = LINE ( 'NONE', #15199, #10677 ) ;
#49258 = DIRECTION ( 'NONE',  ( 0.5364919789714477361, 0.6444004775717706579, 0.5449076811759711036 ) ) ;
#49259 = VECTOR ( 'NONE', #12454, 1000.000000000000000 ) ;
#49260 = DIRECTION ( 'NONE',  ( -0.5364919789714478471, 0.6444004775717705469, -0.5449076811759709926 ) ) ;
#49261 = ORIENTED_EDGE ( 'NONE', *, *, #20488, .F. ) ;
#49263 = VECTOR ( 'NONE', #50683, 1000.000000000000227 ) ;
#49262 = CARTESIAN_POINT ( 'NONE',  ( 5.618093201498282063, -1.050357395465043364, -2.260480044901387764 ) ) ;
#49264 = CARTESIAN_POINT ( 'NONE',  ( -14.94916102560700821, 0.000000000000000000, 2.688082935172642962 ) ) ;
#49265 = ADVANCED_FACE ( 'NONE', ( #53275 ), #31408, .F. ) ;
#49266 = CARTESIAN_POINT ( 'NONE',  ( -7.020097852742797073, 1.644072297827783524, 8.920596959107028212 ) ) ;
#49267 = CARTESIAN_POINT ( 'NONE',  ( -18.36642663825911015, 0.000000000000000000, 10.04813038014351356 ) ) ;
#49268 = ORIENTED_EDGE ( 'NONE', *, *, #13043, .F. ) ;
#49269 = DIRECTION ( 'NONE',  ( 0.5364919789714477361, 0.6444004775717706579, 0.5449076811759711036 ) ) ;
#49270 = ORIENTED_EDGE ( 'NONE', *, *, #39371, .T. ) ;
#49271 = FACE_OUTER_BOUND ( 'NONE', #12257, .T. ) ;
#49272 =( REPRESENTATION_RELATIONSHIP ('NONE','NONE', #51076, #55389 ) REPRESENTATION_RELATIONSHIP_WITH_TRANSFORMATION ( #17546 )SHAPE_REPRESENTATION_RELATIONSHIP( ) );
#49273 = AXIS2_PLACEMENT_3D ( 'NONE', #25686, #47845, #34484 ) ;
#49274 = CARTESIAN_POINT ( 'NONE',  ( -13.04471763214503000, 0.9340140483890038148, 1.719143122047526395 ) ) ;
#49275 = ORIENTED_EDGE ( 'NONE', *, *, #41083, .T. ) ;
#49276 = DIRECTION ( 'NONE',  ( -0.9999697198139514409, -0.000000000000000000, -0.007781995580013368816 ) ) ;
#49277 = VECTOR ( 'NONE', #55393, 1000.000000000000114 ) ;
#49278 = ORIENTED_EDGE ( 'NONE', *, *, #17496, .T. ) ;
#49279 = ORIENTED_EDGE ( 'NONE', *, *, #30412, .T. ) ;
#49280 = ORIENTED_EDGE ( 'NONE', *, *, #2500, .F. ) ;
#49281 = DIRECTION ( 'NONE',  ( -0.6427681459581293666, -0.7660444431189770143, -0.005002170337467561935 ) ) ;
#49282 = ORIENTED_EDGE ( 'NONE', *, *, #34618, .T. ) ;
#49283 = ORIENTED_EDGE ( 'NONE', *, *, #16493, .T. ) ;
#49284 = VECTOR ( 'NONE', #18546, 999.9999999999998863 ) ;
#49285 = CARTESIAN_POINT ( 'NONE',  ( 2.072287782118878319, 0.000000000000000000, -2.950529333540147015 ) ) ;
#49286 = CARTESIAN_POINT ( 'NONE',  ( -16.53317331066696383, 0.000000000000000000, 13.31285208727739899 ) ) ;
#49287 = VERTEX_POINT ( 'NONE', #48131 ) ;
#49288 = VECTOR ( 'NONE', #6788, 1000.000000000000227 ) ;
#49289 = VERTEX_POINT ( 'NONE', #4994 ) ;
#49290 = CARTESIAN_POINT ( 'NONE',  ( -19.60834386242827776, 0.000000000000000000, 4.298478389818581213 ) ) ;
#49291 = EDGE_CURVE ( 'NONE', #50240, #3658, #35178, .T. ) ;
#49292 = ORIENTED_EDGE ( 'NONE', *, *, #53313, .F. ) ;
#49293 = VERTEX_POINT ( 'NONE', #43348 ) ;
#49294 = AXIS2_PLACEMENT_3D ( 'NONE', #26169, #13403, #55695 ) ;
#49295 = CIRCLE ( 'NONE', #18480, 6.000000000000001776 ) ;
#49296 = CARTESIAN_POINT ( 'NONE',  ( -11.87243407472968926, 0.000000000000000000, 11.50246268866867361 ) ) ;
#49297 = CYLINDRICAL_SURFACE ( 'NONE', #51160, 6.999999999999988454 ) ;
#49298 = DIRECTION ( 'NONE',  ( -0.005961354470445682716, -0.6427876096865404731, 0.7660212471507180654 ) ) ;
#49299 = CARTESIAN_POINT ( 'NONE',  ( -27.99767448711536133, 0.000000000000000000, 7.557179307314289218 ) ) ;
#49300 = ORIENTED_EDGE ( 'NONE', *, *, #21401, .F. ) ;
#49301 = LINE ( 'NONE', #45584, #23758 ) ;
#49302 = ORIENTED_EDGE ( 'NONE', *, *, #43166, .T. ) ;
#49303 = EDGE_CURVE ( 'NONE', #19083, #17592, #4441, .T. ) ;
#49304 = LINE ( 'NONE', #40534, #19385 ) ;
#49305 = ADVANCED_FACE ( 'NONE', ( #22323 ), #48420, .F. ) ;
#49306 = EDGE_CURVE ( 'NONE', #36934, #12677, #39651, .T. ) ;
#49307 = LINE ( 'NONE', #5882, #44152 ) ;
#49308 = CARTESIAN_POINT ( 'NONE',  ( -1.086233639165236964, 0.000000000000000000, -2.796443541562362078 ) ) ;
#49309 = DIRECTION ( 'NONE',  ( 0.007781995580012662783, 0.000000000000000000, -0.9999697198139514409 ) ) ;
#49310 = AXIS2_PLACEMENT_3D ( 'NONE', #23926, #54041, #2617 ) ;
#49311 = LINE ( 'NONE', #18947, #14866 ) ;
#49312 = DIRECTION ( 'NONE',  ( 0.007781995580012663651, 0.000000000000000000, -0.9999697198139515519 ) ) ;
#49313 = ORIENTED_EDGE ( 'NONE', *, *, #21807, .F. ) ;
#49314 = DIRECTION ( 'NONE',  ( 0.6427681459581294776, -0.7660444431189769032, 0.005002170337467562802 ) ) ;
#49315 = EDGE_CURVE ( 'NONE', #54647, #19170, #17475, .T. ) ;
#49316 = AXIS2_PLACEMENT_3D ( 'NONE', #21785, #767, #5041 ) ;
#49317 = ORIENTED_EDGE ( 'NONE', *, *, #17818, .T. ) ;
#49318 = DIRECTION ( 'NONE',  ( -1.000000000000000000, 0.000000000000000000, -0.000000000000000000 ) ) ;
#49319 = FACE_OUTER_BOUND ( 'NONE', #1954, .T. ) ;
#49320 = EDGE_CURVE ( 'NONE', #3513, #52053, #14147, .T. ) ;
#49321 = DIRECTION ( 'NONE',  ( 0.3583679495452941066, 0.9335804264972041855, -0.000000000000000000 ) ) ;
#49322 = VECTOR ( 'NONE', #48470, 999.9999999999998863 ) ;
#49323 = CARTESIAN_POINT ( 'NONE',  ( -10.88625143271721996, 0.000000000000000000, 4.197029716307435265 ) ) ;
#49324 = ADVANCED_FACE ( 'NONE', ( #47880 ), #26283, .F. ) ;
#49325 = FACE_OUTER_BOUND ( 'NONE', #8333, .T. ) ;
#49326 = PLANE ( 'NONE',  #43850 ) ;
#49327 = ORIENTED_EDGE ( 'NONE', *, *, #46153, .T. ) ;
#49328 = AXIS2_PLACEMENT_3D ( 'NONE', #42067, #29290, #7424 ) ;
#49329 = DIRECTION ( 'NONE',  ( -0.005961354470445682716, -0.6427876096865404731, 0.7660212471507180654 ) ) ;
#49330 = FACE_OUTER_BOUND ( 'NONE', #8145, .T. ) ;
#49331 = FACE_OUTER_BOUND ( 'NONE', #40939, .T. ) ;
#49332 = VECTOR ( 'NONE', #36591, 999.9999999999998863 ) ;
#49333 = EDGE_CURVE ( 'NONE', #27150, #621, #731, .T. ) ;
#49334 = LINE ( 'NONE', #23499, #52721 ) ;
#49335 = CARTESIAN_POINT ( 'NONE',  ( 3.882677180727608590, -1.000000000000000000, 1.710209902397122672 ) ) ;
#49336 = LINE ( 'NONE', #6734, #2036 ) ;
#49337 = EDGE_CURVE ( 'NONE', #42498, #21652, #36475, .T. ) ;
#49338 = VECTOR ( 'NONE', #2243, 999.9999999999998863 ) ;
#49339 = VECTOR ( 'NONE', #14616, 999.9999999999998863 ) ;
#49340 = FACE_OUTER_BOUND ( 'NONE', #2541, .T. ) ;
#49341 = CARTESIAN_POINT ( 'NONE',  ( -23.33849165029409889, 0.000000000000000000, 5.946783852668351855 ) ) ;
#49342 = ORIENTED_EDGE ( 'NONE', *, *, #26541, .F. ) ;
#49343 = AXIS2_PLACEMENT_3D ( 'NONE', #44468, #5573, #18652 ) ;
#49344 = ORIENTED_EDGE ( 'NONE', *, *, #42546, .T. ) ;
#49345 = ORIENTED_EDGE ( 'NONE', *, *, #32752, .T. ) ;
#49346 = ORIENTED_EDGE ( 'NONE', *, *, #23312, .T. ) ;
#49347 = VECTOR ( 'NONE', #21892, 999.9999999999998863 ) ;
#49348 = ORIENTED_EDGE ( 'NONE', *, *, #11175, .T. ) ;
#49349 = CARTESIAN_POINT ( 'NONE',  ( -10.84028925556084388, -0.1191753592594197858, 11.14116300850493246 ) ) ;
#49350 = LINE ( 'NONE', #27795, #9475 ) ;
#49351 = AXIS2_PLACEMENT_3D ( 'NONE', #48390, #27667, #19123 ) ;
#49352 = ORIENTED_EDGE ( 'NONE', *, *, #45467, .T. ) ;
#49353 = ORIENTED_EDGE ( 'NONE', *, *, #20124, .T. ) ;
#49354 = EDGE_CURVE ( 'NONE', #27552, #43561, #10372, .T. ) ;
#49355 = ORIENTED_EDGE ( 'NONE', *, *, #6917, .F. ) ;
#49356 = AXIS2_PLACEMENT_3D ( 'NONE', #34607, #17036, #3953 ) ;
#49357 = CARTESIAN_POINT ( 'NONE',  ( -67.99506003422921196, -9.491878211616041838, -8.456585623303142896 ) ) ;
#49358 = AXIS2_PLACEMENT_3D ( 'NONE', #6275, #50244, #1709 ) ;
#49359 = DIRECTION ( 'NONE',  ( 0.9999697198139515519, 0.000000000000000000, 0.007781995580013368816 ) ) ;
#49360 = CARTESIAN_POINT ( 'NONE',  ( -17.71921124711865048, 0.9340140483890049250, 5.296940688622762572 ) ) ;
#49361 = VERTEX_POINT ( 'NONE', #10673 ) ;
#49362 = LINE ( 'NONE', #1660, #10149 ) ;
#49363 = ADVANCED_FACE ( 'NONE', ( #36778 ), #2664, .F. ) ;
#49364 = EDGE_CURVE ( 'NONE', #53438, #44267, #15203, .T. ) ;
#49365 = VECTOR ( 'NONE', #15842, 999.9999999999998863 ) ;
#49366 = ORIENTED_EDGE ( 'NONE', *, *, #30532, .T. ) ;
#49367 = CARTESIAN_POINT ( 'NONE',  ( -14.14445781761538790, 0.000000000000000000, 4.910337740446896859 ) ) ;
#49368 = PLANE ( 'NONE',  #48368 ) ;
#49369 = EDGE_CURVE ( 'NONE', #10323, #6907, #54353, .T. ) ;
#49370 = AXIS2_PLACEMENT_3D ( 'NONE', #3854, #34520, #29134 ) ;
#49371 = CARTESIAN_POINT ( 'NONE',  ( -17.67149886328640918, 0.000000000000000000, 6.160211714487092927 ) ) ;
#49372 = CARTESIAN_POINT ( 'NONE',  ( -14.00280974873554030, 0.000000000000000000, 12.40921378708904044 ) ) ;
#49373 = AXIS2_PLACEMENT_3D ( 'NONE', #25376, #7791, #20824 ) ;
#49374 = CARTESIAN_POINT ( 'NONE',  ( -27.06708303904391144, 0.000000000000000000, 7.395095371555332697 ) ) ;
#49375 = DIRECTION ( 'NONE',  ( 0.6427681459581294776, -0.7660444431189769032, 0.005002170337467562802 ) ) ;
#49376 = DIRECTION ( 'NONE',  ( 0.6427681459581294776, -0.7660444431189769032, 0.005002170337467562802 ) ) ;
#49377 = VERTEX_POINT ( 'NONE', #27700 ) ;
#49378 = DIRECTION ( 'NONE',  ( -0.9999697198139514409, -0.000000000000000000, -0.007781995580013368816 ) ) ;
#49379 = ORIENTED_EDGE ( 'NONE', *, *, #17643, .T. ) ;
#49380 = DIRECTION ( 'NONE',  ( 0.005961354470445682716, -0.6427876096865404731, -0.7660212471507180654 ) ) ;
#49381 = LINE ( 'NONE', #11315, #43172 ) ;
#49382 = DIRECTION ( 'NONE',  ( 0.005002170337468016433, -0.7660444431189770143, -0.6427681459581293666 ) ) ;
#49383 = EDGE_CURVE ( 'NONE', #6267, #54772, #15447, .T. ) ;
#49384 = CARTESIAN_POINT ( 'NONE',  ( -18.39746900504187010, 0.000000000000000000, 14.03700784672088808 ) ) ;
#49385 = DIRECTION ( 'NONE',  ( 0.005961354470445682716, -0.6427876096865404731, -0.7660212471507180654 ) ) ;
#49386 = PLANE ( 'NONE',  #52122 ) ;
#49387 = FACE_OUTER_BOUND ( 'NONE', #6323, .T. ) ;
#49388 = EDGE_CURVE ( 'NONE', #43351, #17276, #19984, .T. ) ;
#49389 = AXIS2_PLACEMENT_3D ( 'NONE', #44012, #12596, #28353 ) ;
#49390 = DIRECTION ( 'NONE',  ( 0.007781995580012662783, 0.000000000000000000, -0.9999697198139514409 ) ) ;
#49391 = VECTOR ( 'NONE', #50229, 1000.000000000000000 ) ;
#49392 = DIRECTION ( 'NONE',  ( 0.7660212471507180654, -0.6427876096865404731, 0.005961354470445141482 ) ) ;
#49393 = ORIENTED_EDGE ( 'NONE', *, *, #42215, .T. ) ;
#49394 = LINE ( 'NONE', #1408, #11226 ) ;
#49395 = CARTESIAN_POINT ( 'NONE',  ( -8.470913937488239398, -0.1191753592594177180, 5.223819612497378806 ) ) ;
#49396 = DIRECTION ( 'NONE',  ( 0.7660212471507180654, -0.6427876096865404731, 0.005961354470445141482 ) ) ;
#49397 = VECTOR ( 'NONE', #53375, 1000.000000000000227 ) ;
#49398 = LINE ( 'NONE', #5671, #6806 ) ;
#49399 = EDGE_CURVE ( 'NONE', #54019, #29728, #11192, .T. ) ;
#49400 = LINE ( 'NONE', #10518, #22777 ) ;
#49401 = VECTOR ( 'NONE', #22972, 1000.000000000000227 ) ;
#49402 = LINE ( 'NONE', #24125, #356 ) ;
#49403 = DIRECTION ( 'NONE',  ( 0.5364919789714477361, 0.6444004775717706579, 0.5449076811759711036 ) ) ;
#49404 = CARTESIAN_POINT ( 'NONE',  ( -16.33815322254335456, -3.917936722690661178, 9.458226927869903378 ) ) ;
#49405 = VERTEX_POINT ( 'NONE', #32518 ) ;
#49406 = AXIS2_PLACEMENT_3D ( 'NONE', #27670, #6637, #32498 ) ;
#49407 = ORIENTED_EDGE ( 'NONE', *, *, #9110, .T. ) ;
#49408 = LINE ( 'NONE', #40880, #45028 ) ;
#49409 = VECTOR ( 'NONE', #44743, 999.9999999999998863 ) ;
#49410 = DIRECTION ( 'NONE',  ( 0.005002170337468016433, -0.7660444431189770143, -0.6427681459581293666 ) ) ;
#49411 = VECTOR ( 'NONE', #19006, 999.9999999999998863 ) ;
#49412 = ORIENTED_EDGE ( 'NONE', *, *, #1235, .F. ) ;
#49413 = DIRECTION ( 'NONE',  ( 0.007781995580012663651, -3.146120232559066537E-19, -0.9999697198139514409 ) ) ;
#49414 = ORIENTED_EDGE ( 'NONE', *, *, #52843, .T. ) ;
#49415 = CARTESIAN_POINT ( 'NONE',  ( -12.13851405436063047, 0.000000000000000000, 11.68505802764555135 ) ) ;
#49416 = VECTOR ( 'NONE', #28234, 1000.000000000000227 ) ;
#49417 = ORIENTED_EDGE ( 'NONE', *, *, #22344, .T. ) ;
#49418 = VECTOR ( 'NONE', #43570, 999.9999999999998863 ) ;
#49419 = ORIENTED_EDGE ( 'NONE', *, *, #52504, .T. ) ;
#49420 = EDGE_LOOP ( 'NONE', ( #24248, #21893, #12111, #16657 ) ) ;
#49421 = FACE_OUTER_BOUND ( 'NONE', #30226, .T. ) ;
#49422 = PLANE ( 'NONE',  #43191 ) ;
#49423 = DIRECTION ( 'NONE',  ( -0.005002170337468016433, -0.7660444431189770143, 0.6427681459581293666 ) ) ;
#49424 = EDGE_CURVE ( 'NONE', #41786, #32587, #49820, .T. ) ;
#49425 = ORIENTED_EDGE ( 'NONE', *, *, #9583, .F. ) ;
#49427 = ORIENTED_EDGE ( 'NONE', *, *, #1443, .T. ) ;
#49426 = EDGE_CURVE ( 'NONE', #46034, #32323, #45839, .T. ) ;
#49428 = AXIS2_PLACEMENT_3D ( 'NONE', #22854, #54089, #28229 ) ;
#49429 = DIRECTION ( 'NONE',  ( -0.7660212471507179544, -0.6427876096865405842, -0.005961354470445141482 ) ) ;
#49430 = VECTOR ( 'NONE', #8157, 1000.000000000000227 ) ;
#49432 = EDGE_CURVE ( 'NONE', #27005, #39305, #49563, .T. ) ;
#49431 = ORIENTED_EDGE ( 'NONE', *, *, #10640, .T. ) ;
#49433 = DIRECTION ( 'NONE',  ( 0.000000000000000000, -1.000000000000000000, 0.000000000000000000 ) ) ;
#49434 = ORIENTED_EDGE ( 'NONE', *, *, #40845, .T. ) ;
#49435 = AXIS2_PLACEMENT_3D ( 'NONE', #23673, #6373, #2080 ) ;
#49436 = DIRECTION ( 'NONE',  ( -0.5449076811759708816, 0.6444004775717707689, 0.5364919789714475140 ) ) ;
#49437 = DIRECTION ( 'NONE',  ( 0.9999697198139515519, 0.000000000000000000, 0.007781995580013368816 ) ) ;
#49438 = EDGE_CURVE ( 'NONE', #21318, #38106, #6964, .T. ) ;
#49439 = EDGE_CURVE ( 'NONE', #18068, #48023, #24271, .T. ) ;
#49440 = EDGE_CURVE ( 'NONE', #47558, #37012, #23439, .T. ) ;
#49441 = ORIENTED_EDGE ( 'NONE', *, *, #24597, .F. ) ;
#49442 = LINE ( 'NONE', #18489, #41301 ) ;
#49443 = VECTOR ( 'NONE', #13554, 1000.000000000000227 ) ;
#49444 = ADVANCED_FACE ( 'NONE', ( #45287, #27396, #14621 ), #1574, .T. ) ;
#49445 = CARTESIAN_POINT ( 'NONE',  ( -16.79925329029790149, 0.000000000000000000, 13.49544742625427496 ) ) ;
#49446 = VECTOR ( 'NONE', #40990, 1000.000000000000227 ) ;
#49447 = ORIENTED_EDGE ( 'NONE', *, *, #30429, .F. ) ;
#49448 = LINE ( 'NONE', #50266, #35831 ) ;
#49449 = CARTESIAN_POINT ( 'NONE',  ( -13.56180142820320711, -0.1191753592594188560, 2.598876660244924697 ) ) ;
#49450 = AXIS2_PLACEMENT_3D ( 'NONE', #12639, #34771, #25688 ) ;
#49451 = CARTESIAN_POINT ( 'NONE',  ( -19.34018785077573455, 2.876837460659008361, 4.102531311383550872 ) ) ;
#49452 = ORIENTED_EDGE ( 'NONE', *, *, #14484, .F. ) ;
#49453 = VECTOR ( 'NONE', #1629, 999.9999999999998863 ) ;
#49454 = VECTOR ( 'NONE', #30084, 1000.000000000000227 ) ;
#49455 = DIRECTION ( 'NONE',  ( 0.007781995580012663651, -3.146120232559066537E-19, -0.9999697198139514409 ) ) ;
#49456 = DIRECTION ( 'NONE',  ( -0.005002170337468016433, -0.7660444431189770143, 0.6427681459581293666 ) ) ;
#49457 = CARTESIAN_POINT ( 'NONE',  ( -19.60990026154428278, 0.000000000000000000, 4.498472333781370125 ) ) ;
#49458 = EDGE_CURVE ( 'NONE', #50643, #46950, #6662, .T. ) ;
#49459 = DIRECTION ( 'NONE',  ( -0.6427681459581293666, -0.7660444431189770143, -0.005002170337467561935 ) ) ;
#49460 = DIRECTION ( 'NONE',  ( 0.9999697198139515519, 0.000000000000000000, 0.007781995580013368816 ) ) ;
#49461 = FACE_OUTER_BOUND ( 'NONE', #24832, .T. ) ;
#49462 = AXIS2_PLACEMENT_3D ( 'NONE', #33684, #30284, #24898 ) ;
#49463 = EDGE_CURVE ( 'NONE', #345, #36408, #2402, .T. ) ;
#49464 = AXIS2_PLACEMENT_3D ( 'NONE', #38414, #16854, #32144 ) ;
#49465 = CARTESIAN_POINT ( 'NONE',  ( -65.13797212185212970, -11.17735115307608496, 3.962576710796439805 ) ) ;
#49466 = ORIENTED_EDGE ( 'NONE', *, *, #12437, .F. ) ;
#49467 = CARTESIAN_POINT ( 'NONE',  ( -9.908141408373387193, -0.1191753592594197858, 10.77908512878318703 ) ) ;
#49468 = DIRECTION ( 'NONE',  ( 0.5449076811759707706, 0.6444004775717708799, -0.5364919789714476250 ) ) ;
#49469 = EDGE_CURVE ( 'NONE', #8976, #42837, #10083, .T. ) ;
#49470 = CARTESIAN_POINT ( 'NONE',  ( -66.10170264776731130, 5.898059818321144121E-14, 3.765673540401780262 ) ) ;
#49471 = VERTEX_POINT ( 'NONE', #25123 ) ;
#49472 = CARTESIAN_POINT ( 'NONE',  ( -27.99923088623136636, 0.000000000000000000, 7.757173251277078130 ) ) ;
#49473 = DIRECTION ( 'NONE',  ( 0.6427681459581294776, -0.7660444431189769032, 0.005002170337467562802 ) ) ;
#49474 = EDGE_CURVE ( 'NONE', #12755, #33580, #56056, .T. ) ;
#49475 = CARTESIAN_POINT ( 'NONE',  ( -19.12962290826653700, 0.000000000000000000, 14.40064212555863854 ) ) ;
#49476 = FACE_OUTER_BOUND ( 'NONE', #15920, .T. ) ;
#49477 = EDGE_CURVE ( 'NONE', #6615, #23586, #36732, .T. ) ;
#49478 = DIRECTION ( 'NONE',  ( 0.000000000000000000, -0.000000000000000000, -1.000000000000000000 ) ) ;
#49479 = VECTOR ( 'NONE', #2598, 1000.000000000000227 ) ;
#49480 = ORIENTED_EDGE ( 'NONE', *, *, #55513, .T. ) ;
#49481 = ORIENTED_EDGE ( 'NONE', *, *, #3546, .F. ) ;
#49482 = VECTOR ( 'NONE', #18175, 999.9999999999998863 ) ;
#49483 = CARTESIAN_POINT ( 'NONE',  ( 2.072287782118878319, 0.000000000000000000, -2.950529333540147015 ) ) ;
#49484 = CARTESIAN_POINT ( 'NONE',  ( -18.76354595665420177, -0.1191753592594177458, 14.21882498613976331 ) ) ;
#49485 = VECTOR ( 'NONE', #40234, 1000.000000000000227 ) ;
#49486 = DIRECTION ( 'NONE',  ( 0.005002170337468016433, -0.7660444431189770143, -0.6427681459581293666 ) ) ;
#49487 = ORIENTED_EDGE ( 'NONE', *, *, #52504, .F. ) ;
#49488 = DIRECTION ( 'NONE',  ( 0.2426528472758541499, 0.7422098413412800966, 0.6246952433987894571 ) ) ;
#49489 = ORIENTED_EDGE ( 'NONE', *, *, #20055, .T. ) ;
#49490 = CARTESIAN_POINT ( 'NONE',  ( -19.39860431275361918, 21.26603824944624677, 4.250162336167266020 ) ) ;
#49491 = VECTOR ( 'NONE', #52920, 999.9999999999998863 ) ;
#49493 = VERTEX_POINT ( 'NONE', #51516 ) ;
#49492 = VECTOR ( 'NONE', #17228, 1000.000000000000227 ) ;
#49494 = PLANE ( 'NONE',  #3882 ) ;
#49495 = CARTESIAN_POINT ( 'NONE',  ( -9.309591119262865533, 0.000000000000000000, 6.425292070274053913 ) ) ;
#49496 = CARTESIAN_POINT ( 'NONE',  ( -20.54049170961573267, 0.000000000000000000, 4.660556269540326646 ) ) ;
#49497 = AXIS2_PLACEMENT_3D ( 'NONE', #5530, #31394, #4690 ) ;
#49498 = ORIENTED_EDGE ( 'NONE', *, *, #18343, .F. ) ;
#49499 = VECTOR ( 'NONE', #35689, 1000.000000000000000 ) ;
#49500 = CARTESIAN_POINT ( 'NONE',  ( -11.87243407472968926, 0.000000000000000000, 11.50246268866867361 ) ) ;
#49501 = VECTOR ( 'NONE', #28096, 999.9999999999998863 ) ;
#49502 = ORIENTED_EDGE ( 'NONE', *, *, #241, .F. ) ;
#49503 = VECTOR ( 'NONE', #8930, 1000.000000000000114 ) ;
#49504 = ORIENTED_EDGE ( 'NONE', *, *, #20470, .T. ) ;
#49505 = VECTOR ( 'NONE', #16340, 1000.000000000000000 ) ;
#49506 = ORIENTED_EDGE ( 'NONE', *, *, #10139, .T. ) ;
#49507 = CARTESIAN_POINT ( 'NONE',  ( -9.208861310085005414, 0.000000000000000000, 6.795408042747278721 ) ) ;
#49508 = VERTEX_POINT ( 'NONE', #12610 ) ;
#49509 = DIRECTION ( 'NONE',  ( 0.000000000000000000, -0.000000000000000000, -1.000000000000000000 ) ) ;
#49510 = VERTEX_POINT ( 'NONE', #42430 ) ;
#49511 = CARTESIAN_POINT ( 'NONE',  ( -13.94158982014731585, 0.000000000000000000, 4.542584436305137530 ) ) ;
#49512 = CARTESIAN_POINT ( 'NONE',  ( -13.08486533123210194, 0.000000000000000000, 1.963927175729152541 ) ) ;
#49513 = EDGE_CURVE ( 'NONE', #4495, #40047, #8073, .T. ) ;
#49514 = EDGE_CURVE ( 'NONE', #5690, #24397, #38434, .T. ) ;
#49515 = ORIENTED_EDGE ( 'NONE', *, *, #21811, .T. ) ;
#49516 = FACE_OUTER_BOUND ( 'NONE', #25124, .T. ) ;
#49517 = ORIENTED_EDGE ( 'NONE', *, *, #43340, .F. ) ;
#49518 = EDGE_CURVE ( 'NONE', #21707, #51781, #8332, .T. ) ;
#49519 = AXIS2_PLACEMENT_3D ( 'NONE', #2854, #24199, #20491 ) ;
#49520 = CARTESIAN_POINT ( 'NONE',  ( -11.88464697727586916, 25.79667171432705430, 3.467463535836658561 ) ) ;
#49521 = PLANE ( 'NONE',  #30227 ) ;
#49522 = CARTESIAN_POINT ( 'NONE',  ( -26.13337879274045505, 0.000000000000000000, 6.833023547870798353 ) ) ;
#49523 = LINE ( 'NONE', #14871, #29344 ) ;
#49524 = DIRECTION ( 'NONE',  ( 0.9999697198139515519, 0.000000000000000000, 0.007781995580013368816 ) ) ;
#49525 = PLANE ( 'NONE',  #55477 ) ;
#49526 = PLANE ( 'NONE',  #2949 ) ;
#49527 = AXIS2_PLACEMENT_3D ( 'NONE', #31920, #2642, #45522 ) ;
#49528 = ORIENTED_EDGE ( 'NONE', *, *, #52482, .F. ) ;
#49529 = VERTEX_POINT ( 'NONE', #50664 ) ;
#49530 = PLANE ( 'NONE',  #48217 ) ;
#49531 = DIRECTION ( 'NONE',  ( 0.6246952433987893460, 0.7422098413412802076, -0.2426528472758539279 ) ) ;
#49532 = AXIS2_PLACEMENT_3D ( 'NONE', #53916, #15035, #6785 ) ;
#49533 = LINE ( 'NONE', #6365, #49661 ) ;
#49534 = AXIS2_PLACEMENT_3D ( 'NONE', #55961, #38914, #31220 ) ;
#49535 = VECTOR ( 'NONE', #51478, 999.9999999999998863 ) ;
#49536 = LINE ( 'NONE', #10654, #49446 ) ;
#49537 = VERTEX_POINT ( 'NONE', #42979 ) ;
#49538 = LINE ( 'NONE', #18882, #53994 ) ;
#49539 = DIRECTION ( 'NONE',  ( 0.000000000000000000, -1.000000000000000000, 0.000000000000000000 ) ) ;
#49540 = ORIENTED_EDGE ( 'NONE', *, *, #31513, .F. ) ;
#49541 = PLANE ( 'NONE',  #34733 ) ;
#49542 = LINE ( 'NONE', #14351, #40355 ) ;
#49543 = ORIENTED_EDGE ( 'NONE', *, *, #36843, .F. ) ;
#49544 = AXIS2_PLACEMENT_3D ( 'NONE', #1608, #22627, #39934 ) ;
#49545 = LINE ( 'NONE', #2084, #41540 ) ;
#49546 = DIRECTION ( 'NONE',  ( -0.005961354470445682716, -0.6427876096865404731, 0.7660212471507180654 ) ) ;
#49547 = VECTOR ( 'NONE', #38835, 999.9999999999998863 ) ;
#49548 = DIRECTION ( 'NONE',  ( -0.7660212471507179544, -0.6427876096865405842, -0.005961354470445141482 ) ) ;
#49549 = EDGE_CURVE ( 'NONE', #25319, #53748, #25654, .T. ) ;
#49550 = DIRECTION ( 'NONE',  ( 0.000000000000000000, -1.000000000000000000, 0.000000000000000000 ) ) ;
#49551 = VECTOR ( 'NONE', #19672, 999.9999999999998863 ) ;
#49552 = DIRECTION ( 'NONE',  ( 0.007781995580012663651, -3.146120232559066537E-19, -0.9999697198139514409 ) ) ;
#49553 = ORIENTED_EDGE ( 'NONE', *, *, #22061, .F. ) ;
#49554 = VECTOR ( 'NONE', #47215, 999.9999999999998863 ) ;
#49555 = ADVANCED_FACE ( 'NONE', ( #37893 ), #46971, .F. ) ;
#49556 = ORIENTED_EDGE ( 'NONE', *, *, #50337, .F. ) ;
#49557 = CARTESIAN_POINT ( 'NONE',  ( -19.79569077582305070, 0.000000000000000000, 14.58012466630350445 ) ) ;
#49558 = DIRECTION ( 'NONE',  ( 0.000000000000000000, -1.000000000000000000, 0.000000000000000000 ) ) ;
#49559 = LINE ( 'NONE', #44713, #54183 ) ;
#49560 = ADVANCED_FACE ( 'NONE', ( #21418 ), #33356, .F. ) ;
#49561 = CARTESIAN_POINT ( 'NONE',  ( 2.072287782118878319, 0.000000000000000000, -2.950529333540147015 ) ) ;
#49562 = EDGE_CURVE ( 'NONE', #40568, #33926, #11493, .T. ) ;
#49563 = LINE ( 'NONE', #6134, #33974 ) ;
#49564 = ORIENTED_EDGE ( 'NONE', *, *, #7778, .F. ) ;
#49565 = PLANE ( 'NONE',  #16561 ) ;
#49566 = VECTOR ( 'NONE', #27985, 1000.000000000000227 ) ;
#49567 = PLANE ( 'NONE',  #32305 ) ;
#49568 = DIRECTION ( 'NONE',  ( 0.005961354470445682716, -0.6427876096865404731, -0.7660212471507180654 ) ) ;
#49569 = ORIENTED_EDGE ( 'NONE', *, *, #29521, .T. ) ;
#49570 = LINE ( 'NONE', #40190, #42876 ) ;
#49571 = EDGE_LOOP ( 'NONE', ( #3604, #23685, #48831, #14500 ) ) ;
#49572 = DIRECTION ( 'NONE',  ( 0.7660212471507180654, -0.6427876096865404731, 0.005961354470445141482 ) ) ;
#49573 = VECTOR ( 'NONE', #4549, 999.9999999999998863 ) ;
#49574 = PLANE ( 'NONE',  #27511 ) ;
#49575 = VERTEX_POINT ( 'NONE', #25381 ) ;
#49576 = CARTESIAN_POINT ( 'NONE',  ( -8.831901609284649624, 0.000000000000000000, 4.751675225048217044 ) ) ;
#49577 = AXIS2_PLACEMENT_3D ( 'NONE', #20414, #38021, #21255 ) ;
#49578 = ORIENTED_EDGE ( 'NONE', *, *, #53231, .F. ) ;
#49579 = VERTEX_POINT ( 'NONE', #16289 ) ;
#49580 = VECTOR ( 'NONE', #11800, 1000.000000000000227 ) ;
#49581 = ORIENTED_EDGE ( 'NONE', *, *, #42416, .T. ) ;
#49582 = LINE ( 'NONE', #36236, #48393 ) ;
#49583 = VERTEX_POINT ( 'NONE', #7221 ) ;
#49584 = ORIENTED_EDGE ( 'NONE', *, *, #38087, .T. ) ;
#49585 = CARTESIAN_POINT ( 'NONE',  ( -17.66443310188656213, 0.000000000000000000, 5.252276548676588774 ) ) ;
#49586 = ORIENTED_EDGE ( 'NONE', *, *, #27211, .F. ) ;
#49587 = EDGE_CURVE ( 'NONE', #16962, #17624, #20572, .T. ) ;
#49588 = AXIS2_PLACEMENT_3D ( 'NONE', #37020, #36738, #41548 ) ;
#49589 = VERTEX_POINT ( 'NONE', #29360 ) ;
#49590 = DIRECTION ( 'NONE',  ( -0.6427681459581293666, -0.7660444431189770143, -0.005002170337467561935 ) ) ;
#49591 = EDGE_LOOP ( 'NONE', ( #6515, #16938, #21030, #56137 ) ) ;
#49592 = ORIENTED_EDGE ( 'NONE', *, *, #5709, .F. ) ;
#49593 = EDGE_CURVE ( 'NONE', #37525, #36530, #24817, .T. ) ;
#49594 = ADVANCED_FACE ( 'NONE', ( #46377 ), #46676, .F. ) ;
#49595 = AXIS2_PLACEMENT_3D ( 'NONE', #32853, #46771, #55018 ) ;
#49596 = VECTOR ( 'NONE', #45681, 1000.000000000000000 ) ;
#49597 = CARTESIAN_POINT ( 'NONE',  ( -9.403061784675696089, -0.1191753592594190225, 5.585897492219126015 ) ) ;
#49598 = CARTESIAN_POINT ( 'NONE',  ( -14.63915290389857304, 0.000000000000000000, 8.769134620551508164 ) ) ;
#49599 = FACE_OUTER_BOUND ( 'NONE', #33539, .T. ) ;
#49600 = DIRECTION ( 'NONE',  ( 0.9321478471874541372, 0.000000000000000000, -0.3620778797217453771 ) ) ;
#49601 = ORIENTED_EDGE ( 'NONE', *, *, #2718, .F. ) ;
#49602 = DIRECTION ( 'NONE',  ( 0.6427681459581294776, -0.7660444431189769032, 0.005002170337467562802 ) ) ;
#49603 = VERTEX_POINT ( 'NONE', #42684 ) ;
#49604 = ORIENTED_EDGE ( 'NONE', *, *, #16608, .T. ) ;
#49605 = CARTESIAN_POINT ( 'NONE',  ( -11.40636015113596180, 0.000000000000000000, 11.32142374880780089 ) ) ;
#49606 = AXIS2_PLACEMENT_3D ( 'NONE', #7982, #42871, #54813 ) ;
#49607 = ADVANCED_FACE ( 'NONE', ( #28816 ), #24524, .F. ) ;
#49608 = PLANE ( 'NONE',  #2472 ) ;
#49609 = DIRECTION ( 'NONE',  ( 0.005002170337468016433, -0.7660444431189770143, -0.6427681459581293666 ) ) ;
#49610 = LINE ( 'NONE', #27446, #32099 ) ;
#49611 = DIRECTION ( 'NONE',  ( -0.7660212471507179544, -0.6427876096865405842, -0.005961354470445141482 ) ) ;
#49612 = VERTEX_POINT ( 'NONE', #37601 ) ;
#49613 = LINE ( 'NONE', #45329, #28357 ) ;
#49614 = EDGE_LOOP ( 'NONE', ( #25352, #43016, #34278, #28177 ) ) ;
#49615 = LINE ( 'NONE', #41068, #43813 ) ;
#49616 = DIRECTION ( 'NONE',  ( 0.9999697198139515519, 0.000000000000000000, 0.007781995580013368816 ) ) ;
#49618 = DIRECTION ( 'NONE',  ( 0.6427681459581294776, -0.7660444431189769032, 0.005002170337467562802 ) ) ;
#49617 = VECTOR ( 'NONE', #29364, 999.9999999999998863 ) ;
#49619 = DIRECTION ( 'NONE',  ( -0.7660212471507179544, -0.6427876096865405842, -0.005961354470445141482 ) ) ;
#49620 = CARTESIAN_POINT ( 'NONE',  ( -12.13851405436063047, 0.000000000000000000, 11.68505802764555135 ) ) ;
#49621 = VECTOR ( 'NONE', #6122, 1000.000000000000227 ) ;
#49622 =( BOUNDED_SURFACE ( )  B_SPLINE_SURFACE ( 2, 3, ( 
 ( #11762, #41844, #2944, #23986 ),
 ( #20277, #29079, #41588, #46383 ),
 ( #3528, #12348, #32777, #37061 ) ),
 .UNSPECIFIED., .F., .F., .F. ) 
 B_SPLINE_SURFACE_WITH_KNOTS ( ( 3, 3 ),
 ( 4, 4 ),
 ( 0.000000000000000000, 1.000000000000000000 ),
 ( 0.0004250000000000007895, 0.002075000000000026476 ),
 .UNSPECIFIED. ) 
 GEOMETRIC_REPRESENTATION_ITEM ( )  RATIONAL_B_SPLINE_SURFACE ( (
 ( 1.000000000000000000, 1.000000000000000000, 1.000000000000000000, 1.000000000000000000),
 ( 0.7071067811865484609, 0.7071067811865484609, 0.7071067811865475727, 0.7071067811865475727),
 ( 1.000000000000000000, 1.000000000000000000, 1.000000000000000000, 1.000000000000000000) ) ) 
 REPRESENTATION_ITEM ( '' )  SURFACE ( )  );
#49623 = ORIENTED_EDGE ( 'NONE', *, *, #15764, .F. ) ;
#49624 = CARTESIAN_POINT ( 'NONE',  ( -56.20083583094844926, 4.876814673940706335, 2.999999999999993339 ) ) ;
#49625 = DIRECTION ( 'NONE',  ( 0.005002170337468016433, -0.7660444431189770143, -0.6427681459581293666 ) ) ;
#49626 = CARTESIAN_POINT ( 'NONE',  ( 2.072287782118878319, 0.000000000000000000, -2.950529333540147015 ) ) ;
#49627 = VECTOR ( 'NONE', #51873, 999.9999999999998863 ) ;
#49628 = DIRECTION ( 'NONE',  ( -0.005002170337468016433, -0.7660444431189770143, 0.6427681459581293666 ) ) ;
#49629 = EDGE_CURVE ( 'NONE', #3020, #40968, #54927, .T. ) ;
#49630 = CARTESIAN_POINT ( 'NONE',  ( -16.92365703814605027, 0.000000000000000000, 3.780713160065547029 ) ) ;
#49631 = CARTESIAN_POINT ( 'NONE',  ( -19.60990026154428278, 0.000000000000000000, 4.498472333781370125 ) ) ;
#49632 = CARTESIAN_POINT ( 'NONE',  ( -22.29929853844754462, 4.657758921906511418, 13.18730186385467462 ) ) ;
#49633 = AXIS2_PLACEMENT_3D ( 'NONE', #38146, #46674, #42428 ) ;
#49634 = CARTESIAN_POINT ( 'NONE',  ( -12.85428006665745215, 2.876837460659007473, 6.595740411778870715 ) ) ;
#49635 = PLANE ( 'NONE',  #8392 ) ;
#49636 = ORIENTED_EDGE ( 'NONE', *, *, #53780, .F. ) ;
#49637 = EDGE_CURVE ( 'NONE', #47161, #42624, #7799, .T. ) ;
#49638 = ORIENTED_EDGE ( 'NONE', *, *, #31406, .F. ) ;
#49639 = ADVANCED_FACE ( 'NONE', ( #47520 ), #43289, .F. ) ;
#49641 = ADVANCED_FACE ( 'NONE', ( #31326 ), #17705, .F. ) ;
#49640 = ADVANCED_BREP_SHAPE_REPRESENTATION ( '', ( #2411, #2610 ), #38910 ) ;
#49642 = ORIENTED_EDGE ( 'NONE', *, *, #49041, .F. ) ;
#49643 = EDGE_LOOP ( 'NONE', ( #42619, #46548, #54235, #9512 ) ) ;
#49644 = ORIENTED_EDGE ( 'NONE', *, *, #5, .F. ) ;
#49645 = VERTEX_POINT ( 'NONE', #920 ) ;
#49646 = DIRECTION ( 'NONE',  ( 0.007781995580012663651, -3.146120232559066537E-19, -0.9999697198139514409 ) ) ;
#49647 = ADVANCED_FACE ( 'NONE', ( #12876 ), #5220, .F. ) ;
#49648 = CARTESIAN_POINT ( 'NONE',  ( -15.79438930050108780, 0.000000000000000000, 3.789501382717568312 ) ) ;
#49650 = EDGE_CURVE ( 'NONE', #33225, #55548, #48654, .T. ) ;
#49649 = ORIENTED_EDGE ( 'NONE', *, *, #44801, .T. ) ;
#49651 = ORIENTED_EDGE ( 'NONE', *, *, #6171, .F. ) ;
#49652 = EDGE_LOOP ( 'NONE', ( #46422, #7906, #24396, #5788 ) ) ;
#49653 = ADVANCED_FACE ( 'NONE', ( #22533 ), #21948, .F. ) ;
#49654 = VECTOR ( 'NONE', #33670, 1000.000000000000227 ) ;
#49655 = DIRECTION ( 'NONE',  ( 0.7660212471507180654, -0.6427876096865404731, 0.005961354470445141482 ) ) ;
#49656 = LINE ( 'NONE', #36880, #32798 ) ;
#49657 = DIRECTION ( 'NONE',  ( -0.5364919789714478471, 0.6444004775717705469, -0.5449076811759709926 ) ) ;
#49658 = ORIENTED_EDGE ( 'NONE', *, *, #41605, .F. ) ;
#49659 = CARTESIAN_POINT ( 'NONE',  ( -13.65814614712131636, 0.000000000000000000, 2.128791785447766483 ) ) ;
#49660 = ADVANCED_FACE ( 'NONE', ( #364 ), #4636, .F. ) ;
#49661 = VECTOR ( 'NONE', #36450, 1000.000000000000227 ) ;
#49662 = DIRECTION ( 'NONE',  ( -0.7660212471507179544, -0.6427876096865405842, -0.005961354470445141482 ) ) ;
#49663 = LINE ( 'NONE', #36058, #8498 ) ;
#49664 = EDGE_CURVE ( 'NONE', #39014, #55340, #52610, .T. ) ;
#49665 = CARTESIAN_POINT ( 'NONE',  ( -58.00000000000000711, -9.000000000000000000, 7.102951435054649637E-15 ) ) ;
#49666 = DIRECTION ( 'NONE',  ( -0.9999697198139514409, -0.000000000000000000, -0.007781995580013368816 ) ) ;
#49667 = CARTESIAN_POINT ( 'NONE',  ( -15.47613562217328287, 1.581621852479004442, 5.488488676526967147 ) ) ;
#49668 = DIRECTION ( 'NONE',  ( 0.007781995580012663651, 0.000000000000000000, -0.9999697198139515519 ) ) ;
#49669 = LINE ( 'NONE', #10763, #46641 ) ;
#49670 = DIRECTION ( 'NONE',  ( 0.000000000000000000, -0.000000000000000000, -1.000000000000000000 ) ) ;
#49671 = EDGE_LOOP ( 'NONE', ( #44071, #43737, #4627 ) ) ;
#49672 = FACE_OUTER_BOUND ( 'NONE', #42714, .T. ) ;
#49673 = ORIENTED_EDGE ( 'NONE', *, *, #41680, .T. ) ;
#49674 = FACE_OUTER_BOUND ( 'NONE', #39194, .T. ) ;
#49675 = LINE ( 'NONE', #24104, #30496 ) ;
#49676 = DIRECTION ( 'NONE',  ( 0.5449076811759707706, 0.6444004775717708799, -0.5364919789714476250 ) ) ;
#49677 = DIRECTION ( 'NONE',  ( 0.5000000000000011102, -0.8660254037844380415, 0.000000000000000000 ) ) ;
#49678 = PLANE ( 'NONE',  #51353 ) ;
#49679 = CARTESIAN_POINT ( 'NONE',  ( -20.16176772743538237, -0.1191753592594197858, 14.76194180572237968 ) ) ;
#49680 = CARTESIAN_POINT ( 'NONE',  ( 2.072287782118878319, 0.000000000000000000, -2.950529333540147015 ) ) ;
#49681 = PLANE ( 'NONE',  #16649 ) ;
#49682 =( LENGTH_UNIT ( ) NAMED_UNIT ( * ) SI_UNIT ( .MILLI., .METRE. ) );
#49683 = DIRECTION ( 'NONE',  ( 0.9999697198139515519, 0.000000000000000000, 0.007781995580013368816 ) ) ;
#49684 = LINE ( 'NONE', #32377, #31177 ) ;
#49685 = LINE ( 'NONE', #50777, #18583 ) ;
#49686 = FACE_OUTER_BOUND ( 'NONE', #1262, .T. ) ;
#49687 = DIRECTION ( 'NONE',  ( -0.005961354470445682716, -0.6427876096865404731, 0.7660212471507180654 ) ) ;
#49688 = DIRECTION ( 'NONE',  ( 0.9999697198139515519, 0.000000000000000000, 0.007781995580013368816 ) ) ;
#49689 = EDGE_CURVE ( 'NONE', #7355, #44724, #34735, .T. ) ;
#49690 = DIRECTION ( 'NONE',  ( -0.5449076811759708816, 0.6444004775717707689, 0.5364919789714475140 ) ) ;
#49691 = DIRECTION ( 'NONE',  ( -0.5364919789714478471, 0.6444004775717705469, -0.5449076811759709926 ) ) ;
#49692 = DIRECTION ( 'NONE',  ( 0.6427681459581294776, -0.7660444431189769032, 0.005002170337467562802 ) ) ;
#49693 = VERTEX_POINT ( 'NONE', #39842 ) ;
#49694 = ORIENTED_EDGE ( 'NONE', *, *, #48425, .T. ) ;
#49695 = CARTESIAN_POINT ( 'NONE',  ( -18.29747203306047609, -0.1191753592594177458, 14.03778604627889059 ) ) ;
#49696 = DIRECTION ( 'NONE',  ( 0.007781995580012663651, -3.146120232559066537E-19, -0.9999697198139514409 ) ) ;
#49697 = AXIS2_PLACEMENT_3D ( 'NONE', #19339, #53696, #23878 ) ;
#49698 = VERTEX_POINT ( 'NONE', #4922 ) ;
#49699 = LINE ( 'NONE', #2257, #23162 ) ;
#49700 = ORIENTED_EDGE ( 'NONE', *, *, #43624, .F. ) ;
#49701 = DIRECTION ( 'NONE',  ( -0.005002170337468016433, -0.7660444431189770143, 0.6427681459581293666 ) ) ;
#49702 = ADVANCED_FACE ( 'NONE', ( #13708 ), #40109, .F. ) ;
#49703 = ORIENTED_EDGE ( 'NONE', *, *, #51923, .F. ) ;
#49704 = ORIENTED_EDGE ( 'NONE', *, *, #8814, .F. ) ;
#49705 = ORIENTED_EDGE ( 'NONE', *, *, #11147, .T. ) ;
#49706 = DIRECTION ( 'NONE',  ( 0.6427681459581294776, -0.7660444431189769032, 0.005002170337467562802 ) ) ;
#49707 = LINE ( 'NONE', #31817, #14168 ) ;
#49708 = FACE_OUTER_BOUND ( 'NONE', #38451, .T. ) ;
#49709 = EDGE_CURVE ( 'NONE', #22830, #50706, #31025, .T. ) ;
#49710 = VERTEX_POINT ( 'NONE', #48346 ) ;
#49711 = ORIENTED_EDGE ( 'NONE', *, *, #56142, .F. ) ;
#49712 = ADVANCED_FACE ( 'NONE', ( #71 ), #4379, .F. ) ;
#49713 = DIRECTION ( 'NONE',  ( 0.007781995580012663651, 0.000000000000000000, -0.9999697198139515519 ) ) ;
#49714 = ORIENTED_EDGE ( 'NONE', *, *, #16680, .F. ) ;
#49715 = DIRECTION ( 'NONE',  ( 0.007781995580012662783, 0.000000000000000000, -0.9999697198139514409 ) ) ;
#49716 = ORIENTED_EDGE ( 'NONE', *, *, #43556, .F. ) ;
#49717 = CARTESIAN_POINT ( 'NONE',  ( -10.47421230394850866, 0.000000000000000000, 10.95934586908605723 ) ) ;
#49718 = LINE ( 'NONE', #36951, #24013 ) ;
#49719 = EDGE_CURVE ( 'NONE', #44308, #54486, #26781, .T. ) ;
#49720 = ORIENTED_EDGE ( 'NONE', *, *, #14688, .F. ) ;
#49721 = CARTESIAN_POINT ( 'NONE',  ( -20.06177075545399191, 0.000000000000000000, 14.76272000528038220 ) ) ;
#49722 = ADVANCED_FACE ( 'NONE', ( #44375 ), #5476, .F. ) ;
#49723 = CARTESIAN_POINT ( 'NONE',  ( -12.31143384783145045, -0.8417996532631565332, 2.845647379707433089 ) ) ;
#49724 = EDGE_LOOP ( 'NONE', ( #37230, #47862, #19708, #42524 ) ) ;
#49725 = CARTESIAN_POINT ( 'NONE',  ( -14.66887761629205222, 0.000000000000000000, 12.58869632783390990 ) ) ;
#49726 = DIRECTION ( 'NONE',  ( -0.005961354470445682716, -0.6427876096865404731, 0.7660212471507180654 ) ) ;
#49727 = CARTESIAN_POINT ( 'NONE',  ( -17.46532115785441519, 0.000000000000000000, 13.67492996699914265 ) ) ;
#49728 = ORIENTED_EDGE ( 'NONE', *, *, #28588, .F. ) ;
#49729 = VECTOR ( 'NONE', #47987, 1000.000000000000000 ) ;
#49730 = CARTESIAN_POINT ( 'NONE',  ( -16.68496742766923191, 1.905425754524007198, 6.489457369783435681 ) ) ;
#49731 = DIRECTION ( 'NONE',  ( 0.7660212471507180654, -0.6427876096865404731, 0.005961354470445141482 ) ) ;
#49732 = CARTESIAN_POINT ( 'NONE',  ( -16.81345671998191449, 0.000000000000000000, 3.412238694616132495 ) ) ;
#49733 = PLANE ( 'NONE',  #30490 ) ;
#49734 = CARTESIAN_POINT ( 'NONE',  ( -16.81345671998191449, 0.000000000000000000, 3.412238694616132495 ) ) ;
#49735 = DIRECTION ( 'NONE',  ( -0.005002170337468016433, -0.7660444431189770143, 0.6427681459581293666 ) ) ;
#49736 = DIRECTION ( 'NONE',  ( 0.007781995580012663651, 0.000000000000000000, -0.9999697198139515519 ) ) ;
#49737 = ORIENTED_EDGE ( 'NONE', *, *, #25977, .F. ) ;
#49738 = LINE ( 'NONE', #6866, #39840 ) ;
#49739 = DIRECTION ( 'NONE',  ( -0.005961354470445682716, -0.6427876096865404731, 0.7660212471507180654 ) ) ;
#49740 = CARTESIAN_POINT ( 'NONE',  ( -66.61623392118266906, 1.734723475976807094E-15, 5.190771789781507550 ) ) ;
#49741 = ORIENTED_EDGE ( 'NONE', *, *, #43186, .F. ) ;
#49742 = CARTESIAN_POINT ( 'NONE',  ( -11.88160593113000907, -1.975113310420658852, 4.538648407496340020 ) ) ;
#49743 = CARTESIAN_POINT ( 'NONE',  ( -21.79697860796153464, 3.524445264749008988, 11.13222295634402137 ) ) ;
#49744 = EDGE_CURVE ( 'NONE', #33688, #44617, #34458, .T. ) ;
#49745 = DIRECTION ( 'NONE',  ( 0.007781995580012662783, 0.000000000000000000, -0.9999697198139514409 ) ) ;
#49746 = EDGE_CURVE ( 'NONE', #49698, #1575, #26224, .T. ) ;
#49747 = DIRECTION ( 'NONE',  ( -0.6427681459581293666, -0.7660444431189770143, -0.005002170337467561935 ) ) ;
#49748 = LINE ( 'NONE', #15374, #22933 ) ;
#49749 = ORIENTED_EDGE ( 'NONE', *, *, #31022, .T. ) ;
#49750 = EDGE_CURVE ( 'NONE', #21379, #8596, #10603, .T. ) ;
#49751 = VERTEX_POINT ( 'NONE', #54286 ) ;
#49752 = ADVANCED_FACE ( 'NONE', ( #32165 ), #19081, .F. ) ;
#49753 = LINE ( 'NONE', #14832, #10534 ) ;
#49754 = EDGE_CURVE ( 'NONE', #9106, #33384, #6067, .T. ) ;
#49755 = EDGE_CURVE ( 'NONE', #38597, #18224, #24203, .T. ) ;
#49756 = ADVANCED_FACE ( 'NONE', ( #15136 ), #10300, .F. ) ;
#49757 = CARTESIAN_POINT ( 'NONE',  ( -15.53681210902263921, 0.000000000000000000, 4.699496061180079565 ) ) ;
#49758 = ORIENTED_EDGE ( 'NONE', *, *, #12853, .F. ) ;
#49759 = LINE ( 'NONE', #50008, #25828 ) ;
#49760 = ORIENTED_EDGE ( 'NONE', *, *, #9442, .T. ) ;
#49761 = CARTESIAN_POINT ( 'NONE',  ( -32.10901097986136676, -1.000000000000000000, 16.76339505873265168 ) ) ;
#49762 = ORIENTED_EDGE ( 'NONE', *, *, #34376, .F. ) ;
#49763 = EDGE_LOOP ( 'NONE', ( #15353, #25313, #38985, #44886 ) ) ;
#49764 = DIRECTION ( 'NONE',  ( -0.5449076811759708816, 0.6444004775717707689, 0.5364919789714475140 ) ) ;
#49765 = PLANE ( 'NONE',  #6904 ) ;
#49766 = CARTESIAN_POINT ( 'NONE',  ( -12.06424151263527023, 0.000000000000000000, 2.141195919867798558 ) ) ;
#49767 = ORIENTED_EDGE ( 'NONE', *, *, #46193, .T. ) ;
#49768 = AXIS2_PLACEMENT_3D ( 'NONE', #51204, #47805, #20556 ) ;
#49769 = CARTESIAN_POINT ( 'NONE',  ( -15.88053067323646417, -0.1191753592594197858, 2.950163842912994383 ) ) ;
#49770 = EDGE_CURVE ( 'NONE', #15428, #10587, #4059, .T. ) ;
#49771 = EDGE_LOOP ( 'NONE', ( #35808, #18117, #3284, #6745 ) ) ;
#49773 = EDGE_LOOP ( 'NONE', ( #1696, #14731, #53320, #42011 ) ) ;
#49772 = EDGE_CURVE ( 'NONE', #12737, #31264, #6884, .T. ) ;
#49774 = EDGE_LOOP ( 'NONE', ( #41898, #48347, #45640, #53724 ) ) ;
#49775 = CARTESIAN_POINT ( 'NONE',  ( -20.16884058355513432, -2.946525016555658905, 9.351943885874463902 ) ) ;
#49776 = EDGE_CURVE ( 'NONE', #43469, #50912, #1504, .T. ) ;
#49777 = EDGE_LOOP ( 'NONE', ( #26047, #25262, #18754, #3950 ) ) ;
#49778 = CARTESIAN_POINT ( 'NONE',  ( -9.908141408373387193, -0.1191753592594197858, 10.77908512878318703 ) ) ;
#49779 = EDGE_LOOP ( 'NONE', ( #758, #5776, #28309, #31954 ) ) ;
#49780 = CARTESIAN_POINT ( 'NONE',  ( -15.86710544311044302, 0.000000000000000000, 13.13336954653252953 ) ) ;
#49781 = DIRECTION ( 'NONE',  ( 0.6427681459581294776, -0.7660444431189769032, 0.005002170337467562802 ) ) ;
#49782 = EDGE_CURVE ( 'NONE', #9324, #13476, #49759, .T. ) ;
#49783 = ORIENTED_EDGE ( 'NONE', *, *, #19738, .F. ) ;
#49784 = DIRECTION ( 'NONE',  ( 0.000000000000000000, -0.000000000000000000, -1.000000000000000000 ) ) ;
#49785 = EDGE_LOOP ( 'NONE', ( #13760, #44972, #27154, #6308 ) ) ;
#49786 = FACE_OUTER_BOUND ( 'NONE', #18632, .T. ) ;
#49787 = CARTESIAN_POINT ( 'NONE',  ( -17.74560456716937296, 0.000000000000000000, 3.774316574337878372 ) ) ;
#49788 = CARTESIAN_POINT ( 'NONE',  ( -14.94916102560700821, 0.000000000000000000, 2.688082935172642962 ) ) ;
#49789 = DIRECTION ( 'NONE',  ( 0.6427681459581294776, -0.7660444431189769032, 0.005002170337467562802 ) ) ;
#49790 = PLANE ( 'NONE',  #7840 ) ;
#49791 = DIRECTION ( 'NONE',  ( 0.007781995580012662783, 0.000000000000000000, -0.9999697198139514409 ) ) ;
#49792 = FACE_OUTER_BOUND ( 'NONE', #7263, .T. ) ;
#49793 = ORIENTED_EDGE ( 'NONE', *, *, #29872, .T. ) ;
#49794 = ORIENTED_EDGE ( 'NONE', *, *, #46328, .T. ) ;
#49795 = CARTESIAN_POINT ( 'NONE',  ( -56.56281744964225311, 4.044141780346881099, 2.346371251900079447 ) ) ;
#49796 = CARTESIAN_POINT ( 'NONE',  ( -68.83743834501466097, -9.171101568560214190, 7.487530722355575818 ) ) ;
#49797 = CARTESIAN_POINT ( 'NONE',  ( -13.00788557384385413, 0.000000000000000000, 3.980512612620602297 ) ) ;
#49798 = CARTESIAN_POINT ( 'NONE',  ( -20.37303252807906162, -1.003701604285655469, 6.242754764109628596 ) ) ;
#49799 = DIRECTION ( 'NONE',  ( 0.5449076811759707706, 0.6444004775717708799, -0.5364919789714476250 ) ) ;
#49800 = EDGE_LOOP ( 'NONE', ( #11945, #30594, #52588, #12545 ) ) ;
#49801 = CARTESIAN_POINT ( 'NONE',  ( -11.77243710274829525, -0.1191753592594197858, 11.50324088822667612 ) ) ;
#49802 = DIRECTION ( 'NONE',  ( 0.000000000000000000, -0.000000000000000000, -1.000000000000000000 ) ) ;
#49803 = ORIENTED_EDGE ( 'NONE', *, *, #3742, .T. ) ;
#49804 = LINE ( 'NONE', #32748, #20251 ) ;
#49805 = CARTESIAN_POINT ( 'NONE',  ( -21.47263955680318404, 0.000000000000000000, 5.022634149262071190 ) ) ;
#49806 = VERTEX_POINT ( 'NONE', #36990 ) ;
#49807 = CARTESIAN_POINT ( 'NONE',  ( -69.23012684808540484, 1.999999999999999112, -6.702751532743288720 ) ) ;
#49808 = DIRECTION ( 'NONE',  ( 0.005002170337468016433, -0.7660444431189770143, -0.6427681459581293666 ) ) ;
#49809 = CARTESIAN_POINT ( 'NONE',  ( -16.29638889291085135, 0.000000000000000000, 8.586911613300497237 ) ) ;
#49810 = CARTESIAN_POINT ( 'NONE',  ( -12.37052422292021348, 4.010151117816511679, 1.359118628339639256 ) ) ;
#49811 = LINE ( 'NONE', #33347, #52828 ) ;
#49812 = ORIENTED_EDGE ( 'NONE', *, *, #7350, .F. ) ;
#49813 = EDGE_LOOP ( 'NONE', ( #32699, #18336, #1217, #43586 ) ) ;
#49814 = DIRECTION ( 'NONE',  ( 0.9999697198139515519, 0.000000000000000000, 0.007781995580013368816 ) ) ;
#49815 = CARTESIAN_POINT ( 'NONE',  ( -10.47421230394850866, 0.000000000000000000, 10.95934586908605723 ) ) ;
#49816 = CARTESIAN_POINT ( 'NONE',  ( -13.69263478918470867, 0.000000000000000000, 6.560508224540939182 ) ) ;
#49817 = ADVANCED_FACE ( 'NONE', ( #15385 ), #40940, .F. ) ;
#49818 = EDGE_CURVE ( 'NONE', #11345, #10380, #1923, .T. ) ;
#49819 = LINE ( 'NONE', #45543, #50029 ) ;
#49820 = LINE ( 'NONE', #14908, #28532 ) ;
#49822 = EDGE_CURVE ( 'NONE', #40102, #35268, #36157, .T. ) ;
#49821 = ORIENTED_EDGE ( 'NONE', *, *, #31749, .T. ) ;
#49823 = DIRECTION ( 'NONE',  ( 0.6427681459581294776, -0.7660444431189769032, 0.005002170337467562802 ) ) ;
#49824 = PLANE ( 'NONE',  #35064 ) ;
#49825 = DIRECTION ( 'NONE',  ( -0.000000000000000000, -0.000000000000000000, -1.000000000000000000 ) ) ;
#49826 = VERTEX_POINT ( 'NONE', #28163 ) ;
#49827 = DIRECTION ( 'NONE',  ( -0.5364919789714478471, 0.6444004775717705469, -0.5449076811759709926 ) ) ;
#49828 = DIRECTION ( 'NONE',  ( -0.005961354470445682716, -0.6427876096865404731, 0.7660212471507180654 ) ) ;
#49829 = PLANE ( 'NONE',  #46546 ) ;
#49830 = ORIENTED_EDGE ( 'NONE', *, *, #2687, .F. ) ;
#49831 = DIRECTION ( 'NONE',  ( 0.9999697198139515519, 0.000000000000000000, 0.007781995580013368816 ) ) ;
#49832 = ORIENTED_EDGE ( 'NONE', *, *, #35393, .T. ) ;
#49833 = EDGE_CURVE ( 'NONE', #9862, #21743, #45474, .T. ) ;
#49834 = ORIENTED_EDGE ( 'NONE', *, *, #40012, .T. ) ;
#49835 = EDGE_LOOP ( 'NONE', ( #41794, #48991, #46271 ) ) ;
#49836 = LINE ( 'NONE', #36797, #19367 ) ;
#49837 = EDGE_LOOP ( 'NONE', ( #47823, #41258, #8215, #46696 ) ) ;
#49838 = EDGE_CURVE ( 'NONE', #22139, #54019, #53202, .T. ) ;
#49839 = ORIENTED_EDGE ( 'NONE', *, *, #1905, .T. ) ;
#49840 = LINE ( 'NONE', #46134, #6666 ) ;
#49841 = EDGE_LOOP ( 'NONE', ( #10394, #33088, #38624 ) ) ;
#49842 = PRODUCT_DEFINITION_FORMATION_WITH_SPECIFIED_SOURCE ( 'ANY', '', #22810, .NOT_KNOWN. ) ;
#49843 = EDGE_CURVE ( 'NONE', #25320, #6407, #31614, .T. ) ;
#49844 = ORIENTED_EDGE ( 'NONE', *, *, #3159, .F. ) ;
#49845 = CARTESIAN_POINT ( 'NONE',  ( -26.54131626755147977, 17.33463975416308500, 4.634068379122165737 ) ) ;
#49846 = VERTEX_POINT ( 'NONE', #5763 ) ;
#49847 = ORIENTED_EDGE ( 'NONE', *, *, #42302, .T. ) ;
#49848 = EDGE_CURVE ( 'NONE', #44182, #22811, #53457, .T. ) ;
#49849 = VERTEX_POINT ( 'NONE', #20768 ) ;
#49850 = DIRECTION ( 'NONE',  ( -0.5449076811759708816, 0.6444004775717707689, 0.5364919789714475140 ) ) ;
#49851 = CARTESIAN_POINT ( 'NONE',  ( -20.54204810873173415, 0.000000000000000000, 4.860550213503115558 ) ) ;
#49852 = DIRECTION ( 'NONE',  ( 0.007781995580012663651, -3.146120232559066537E-19, -0.9999697198139514409 ) ) ;
#49853 = LINE ( 'NONE', #7251, #3328 ) ;
#49854 = ORIENTED_EDGE ( 'NONE', *, *, #18491, .T. ) ;
#49855 = CARTESIAN_POINT ( 'NONE',  ( 2.072287782118878319, 0.000000000000000000, -2.950529333540147015 ) ) ;
#49856 = EDGE_LOOP ( 'NONE', ( #45863, #24923, #51312, #53193, #385 ) ) ;
#49857 = VERTEX_POINT ( 'NONE', #47157 ) ;
#49858 = CARTESIAN_POINT ( 'NONE',  ( -6.110905869600904872, 1.712176620043476140E-14, 2.600000000000000089 ) ) ;
#49859 = CARTESIAN_POINT ( 'NONE',  ( -46.52156441860571334, 5.799038105676371124, -5.000000000000000000 ) ) ;
#49860 = CARTESIAN_POINT ( 'NONE',  ( -12.30091215004045679, 2.229229656569005957, 5.317958784709427178 ) ) ;
#49861 = CARTESIAN_POINT ( 'NONE',  ( -17.57617378642196115, 4.657758921906512306, 3.360507623857465820 ) ) ;
#49862 = DIRECTION ( 'NONE',  ( 0.6427681459581294776, -0.7660444431189769032, 0.005002170337467562802 ) ) ;
#49863 = ORIENTED_EDGE ( 'NONE', *, *, #43017, .F. ) ;
#49864 = LINE ( 'NONE', #10962, #19280 ) ;
#49865 = ORIENTED_EDGE ( 'NONE', *, *, #29946, .T. ) ;
#49866 = DIRECTION ( 'NONE',  ( 0.007781995580012662783, 0.000000000000000000, -0.9999697198139514409 ) ) ;
#49867 = DIRECTION ( 'NONE',  ( 0.9999697198139515519, 0.000000000000000000, 0.007781995580013368816 ) ) ;
#49868 = LINE ( 'NONE', #37103, #26320 ) ;
#49869 = DIRECTION ( 'NONE',  ( -0.005961354470445682716, -0.6427876096865404731, 0.7660212471507180654 ) ) ;
#49870 = DIRECTION ( 'NONE',  ( 0.000000000000000000, -0.000000000000000000, -1.000000000000000000 ) ) ;
#49871 = VECTOR ( 'NONE', #23220, 999.9999999999998863 ) ;
#49872 = EDGE_LOOP ( 'NONE', ( #53410, #39211, #6157, #14498 ) ) ;
#49873 = CARTESIAN_POINT ( 'NONE',  ( -19.60990026154428278, 0.000000000000000000, 4.498472333781370125 ) ) ;
#49874 = CARTESIAN_POINT ( 'NONE',  ( -15.55420528410555292, 3.362543313726509719, 2.616430550317521586 ) ) ;
#49875 = LINE ( 'NONE', #27191, #24564 ) ;
#49876 = EDGE_CURVE ( 'NONE', #37328, #2943, #11949, .T. ) ;
#49877 = DIRECTION ( 'NONE',  ( -0.7660212471507179544, -0.6427876096865405842, -0.005961354470445141482 ) ) ;
#49878 = DIRECTION ( 'NONE',  ( 0.000000000000000000, -1.000000000000000000, 0.000000000000000000 ) ) ;
#49879 = EDGE_CURVE ( 'NONE', #55101, #38023, #34130, .T. ) ;
#49880 = DIRECTION ( 'NONE',  ( -0.5449076811759708816, 0.6444004775717707689, 0.5364919789714475140 ) ) ;
#49881 = ADVANCED_FACE ( 'NONE', ( #25045 ), #20495, .F. ) ;
#49882 = CARTESIAN_POINT ( 'NONE',  ( 1.086233639165236964, 0.000000000000000000, 2.796443541562362078 ) ) ;
#49883 = LINE ( 'NONE', #54414, #25135 ) ;
#49884 = CARTESIAN_POINT ( 'NONE',  ( -11.90068819181640691, 0.1245042932765045296, 1.708285316316361158 ) ) ;
#49885 = ORIENTED_EDGE ( 'NONE', *, *, #2857, .T. ) ;
#49886 = ORIENTED_EDGE ( 'NONE', *, *, #19365, .F. ) ;
#49887 = ORIENTED_EDGE ( 'NONE', *, *, #34330, .F. ) ;
#49888 = VERTEX_POINT ( 'NONE', #2601 ) ;
#49889 = ORIENTED_EDGE ( 'NONE', *, *, #36334, .F. ) ;
#49890 = CARTESIAN_POINT ( 'NONE',  ( -13.27065584551087163, 0.000000000000000000, 12.04557950825129176 ) ) ;
#49891 = DIRECTION ( 'NONE',  ( -0.000000000000000000, -0.000000000000000000, -1.000000000000000000 ) ) ;
#49892 = ORIENTED_EDGE ( 'NONE', *, *, #17125, .F. ) ;
#49893 = CARTESIAN_POINT ( 'NONE',  ( -14.39473050296726697, 0.000000000000000000, 3.061729711506068874 ) ) ;
#49894 = EDGE_LOOP ( 'NONE', ( #34841, #51311, #17990, #33017 ) ) ;
#49895 = VERTEX_POINT ( 'NONE', #29008 ) ;
#49896 = ADVANCED_FACE ( 'NONE', ( #42056 ), #50853, .F. ) ;
#49897 = AXIS2_PLACEMENT_3D ( 'NONE', #7857, #24039, #45900 ) ;
#49898 = CARTESIAN_POINT ( 'NONE',  ( -65.19693841791328737, -9.171005842923255713, -1.901374313760128665 ) ) ;
#49899 = EDGE_CURVE ( 'NONE', #27583, #37134, #11690, .T. ) ;
#49900 = DIRECTION ( 'NONE',  ( 0.005002170337468016433, -0.7660444431189770143, -0.6427681459581293666 ) ) ;
#49901 = DIRECTION ( 'NONE',  ( 0.007781995580012662783, 0.000000000000000000, -0.9999697198139514409 ) ) ;
#49902 = ORIENTED_EDGE ( 'NONE', *, *, #11109, .F. ) ;
#49903 = CARTESIAN_POINT ( 'NONE',  ( -18.86354292863559579, 0.000000000000000000, 14.21804678658176080 ) ) ;
#49904 = LINE ( 'NONE', #28329, #33673 ) ;
#49905 = EDGE_CURVE ( 'NONE', #21119, #23033, #3715, .T. ) ;
#49906 = DIRECTION ( 'NONE',  ( 0.5364919789714477361, 0.6444004775717706579, 0.5449076811759711036 ) ) ;
#49907 = PLANE ( 'NONE',  #25502 ) ;
#49908 = DIRECTION ( 'NONE',  ( 0.9999697198139515519, 0.000000000000000000, 0.007781995580013368816 ) ) ;
#49909 = DIRECTION ( 'NONE',  ( -0.9999697198139514409, -0.000000000000000000, -0.007781995580013368816 ) ) ;
#49910 = CARTESIAN_POINT ( 'NONE',  ( -16.81267852042391198, -0.1191753592594197858, 3.312241722634738039 ) ) ;
#49911 = DIRECTION ( 'NONE',  ( 0.5364919789714477361, 0.6444004775717706579, 0.5449076811759711036 ) ) ;
#49912 = LINE ( 'NONE', #41425, #49242 ) ;
#49913 = EDGE_LOOP ( 'NONE', ( #55134, #17453, #44579, #50103 ) ) ;
#49914 = CARTESIAN_POINT ( 'NONE',  ( -15.09804169372909399, 0.000000000000000000, 8.026899302267967329 ) ) ;
#49915 = ORIENTED_EDGE ( 'NONE', *, *, #26987, .F. ) ;
#49916 = DIRECTION ( 'NONE',  ( 0.9321478471874541372, 0.000000000000000000, -0.3620778797217453771 ) ) ;
#49917 = CARTESIAN_POINT ( 'NONE',  ( -17.36532418587302473, -0.1191753592594177458, 13.67570816655714516 ) ) ;
#49918 = CARTESIAN_POINT ( 'NONE',  ( 2.072287782118878319, 0.000000000000000000, -2.950529333540147015 ) ) ;
#49919 = DIRECTION ( 'NONE',  ( 0.007781995580012662783, 0.000000000000000000, -0.9999697198139514409 ) ) ;
#49920 = LINE ( 'NONE', #19005, #10548 ) ;
#49921 = CARTESIAN_POINT ( 'NONE',  ( -18.67775241435682432, 0.000000000000000000, 4.136394454059623804 ) ) ;
#49922 = EDGE_CURVE ( 'NONE', #20261, #52731, #29592, .T. ) ;
#49923 = DIRECTION ( 'NONE',  ( 0.000000000000000000, 0.000000000000000000, 1.000000000000000000 ) ) ;
#49924 = PRESENTATION_STYLE_ASSIGNMENT (( #11865 ) ) ;
#49925 = CARTESIAN_POINT ( 'NONE',  ( -20.08683635851538796, -0.1191753592594195638, 5.133421818297142281 ) ) ;
#49926 = PLANE ( 'NONE',  #9403 ) ;
#49927 = LINE ( 'NONE', #23554, #31265 ) ;
#49928 = ADVANCED_FACE ( 'NONE', ( #33544 ), #8006, .F. ) ;
#49929 = LINE ( 'NONE', #31796, #40907 ) ;
#49930 = CARTESIAN_POINT ( 'NONE',  ( -21.47263955680318404, 0.000000000000000000, 5.022634149262071190 ) ) ;
#49931 = VECTOR ( 'NONE', #35275, 1000.000000000000227 ) ;
#49932 = EDGE_CURVE ( 'NONE', #16959, #35406, #50300, .T. ) ;
#49933 = CARTESIAN_POINT ( 'NONE',  ( -12.13851405436063047, 0.000000000000000000, 11.68505802764555135 ) ) ;
#49934 = DIRECTION ( 'NONE',  ( 0.5449076811759707706, 0.6444004775717708799, -0.5364919789714476250 ) ) ;
#49935 = DIRECTION ( 'NONE',  ( -0.005002170337468016433, -0.7660444431189770143, 0.6427681459581293666 ) ) ;
#49936 = EDGE_CURVE ( 'NONE', #50536, #44267, #46305, .T. ) ;
#49937 = CARTESIAN_POINT ( 'NONE',  ( -23.33693525117809386, 0.000000000000000000, 5.746789908705562944 ) ) ;
#49938 = VERTEX_POINT ( 'NONE', #2861 ) ;
#49939 = VECTOR ( 'NONE', #28936, 1000.000000000000227 ) ;
#49940 = FACE_OUTER_BOUND ( 'NONE', #450, .T. ) ;
#49941 = EDGE_LOOP ( 'NONE', ( #45551, #28696, #38728, #35920 ) ) ;
#49942 = CARTESIAN_POINT ( 'NONE',  ( -16.27758817276315284, 0.000000000000000000, 6.171059449791123086 ) ) ;
#49943 = DIRECTION ( 'NONE',  ( 0.6427681459581294776, -0.7660444431189769032, 0.005002170337467562802 ) ) ;
#49944 = ORIENTED_EDGE ( 'NONE', *, *, #20936, .T. ) ;
#49945 = CARTESIAN_POINT ( 'NONE',  ( -11.67244013076689946, 0.000000000000000000, 11.50401908778467863 ) ) ;
#49946 = ORIENTED_EDGE ( 'NONE', *, *, #5419, .T. ) ;
#49947 = PLANE ( 'NONE',  #2078 ) ;
#49948 = EDGE_CURVE ( 'NONE', #38604, #187, #16224, .T. ) ;
#49949 = VERTEX_POINT ( 'NONE', #7160 ) ;
#49950 = VERTEX_POINT ( 'NONE', #8263 ) ;
#49951 = ORIENTED_EDGE ( 'NONE', *, *, #37584, .T. ) ;
#49952 = CARTESIAN_POINT ( 'NONE',  ( -19.29729739867497074, 0.6102101463440047224, 4.158188481645193058 ) ) ;
#49953 = CARTESIAN_POINT ( 'NONE',  ( -22.40556560354864146, -0.1191753592594197858, 5.484709000965211523 ) ) ;
#49954 = CARTESIAN_POINT ( 'NONE',  ( 2.072287782118878319, 0.000000000000000000, -2.950529333540147015 ) ) ;
#49955 = VECTOR ( 'NONE', #55906, 1000.000000000000114 ) ;
#49956 = VECTOR ( 'NONE', #6830, 999.9999999999998863 ) ;
#49957 = ORIENTED_EDGE ( 'NONE', *, *, #39830, .F. ) ;
#49958 = ORIENTED_EDGE ( 'NONE', *, *, #5235, .T. ) ;
#49959 = LINE ( 'NONE', #28389, #9157 ) ;
#49960 = ORIENTED_EDGE ( 'NONE', *, *, #32084, .T. ) ;
#49961 = CARTESIAN_POINT ( 'NONE',  ( -26.13415699229845757, -0.1191753592594197858, 6.933020519852192365 ) ) ;
#49962 = ORIENTED_EDGE ( 'NONE', *, *, #40608, .T. ) ;
#49963 = DIRECTION ( 'NONE',  ( 0.000000000000000000, -0.000000000000000000, -1.000000000000000000 ) ) ;
#49964 = DIRECTION ( 'NONE',  ( -0.5364919789714478471, 0.6444004775717705469, -0.5449076811759709926 ) ) ;
#49965 = ORIENTED_EDGE ( 'NONE', *, *, #26007, .F. ) ;
#49966 = VECTOR ( 'NONE', #40293, 999.9999999999998863 ) ;
#49967 = LINE ( 'NONE', #20145, #18266 ) ;
#49968 = ADVANCED_FACE ( 'NONE', ( #21033 ), #55687, .F. ) ;
#49969 = AXIS2_PLACEMENT_3D ( 'NONE', #9063, #43681, #35204 ) ;
#49970 = CARTESIAN_POINT ( 'NONE',  ( -12.80458192191714595, 0.000000000000000000, 11.86454056839041726 ) ) ;
#49971 = ORIENTED_EDGE ( 'NONE', *, *, #35542, .T. ) ;
#49972 = LINE ( 'NONE', #11079, #51358 ) ;
#49973 = DIRECTION ( 'NONE',  ( 0.5364919789714477361, 0.6444004775717706579, 0.5449076811759711036 ) ) ;
#49974 = CARTESIAN_POINT ( 'NONE',  ( -20.54049170961573267, 0.000000000000000000, 4.660556269540326646 ) ) ;
#49975 = VERTEX_POINT ( 'NONE', #3452 ) ;
#49976 = ADVANCED_FACE ( 'NONE', ( #54843 ), #41519, .F. ) ;
#49977 = CARTESIAN_POINT ( 'NONE',  ( -13.36481033154660913, 0.000000000000000000, 8.409719779305810050 ) ) ;
#49978 = FACE_OUTER_BOUND ( 'NONE', #44811, .T. ) ;
#49979 = DIRECTION ( 'NONE',  ( -0.5449076811759708816, 0.6444004775717707689, 0.5364919789714475140 ) ) ;
#49980 = CARTESIAN_POINT ( 'NONE',  ( -9.037643660258000367, 0.000000000000000000, 5.488738232447742504 ) ) ;
#49981 = EDGE_CURVE ( 'NONE', #26517, #7643, #16495, .T. ) ;
#49982 = CARTESIAN_POINT ( 'NONE',  ( -23.52058642966956370, 18.95428049856751329, 4.498258486333376993 ) ) ;
#49984 = ADVANCED_FACE ( 'NONE', ( #15952 ), #33291, .F. ) ;
#49983 = DIRECTION ( 'NONE',  ( -0.9999697198139514409, -0.000000000000000000, -0.007781995580013368816 ) ) ;
#49985 = CARTESIAN_POINT ( 'NONE',  ( -66.03455808990733544, -11.28016643516713202, 6.196202711025575738 ) ) ;
#49986 = EDGE_LOOP ( 'NONE', ( #9566, #44979, #1324, #49556 ) ) ;
#49987 = DIRECTION ( 'NONE',  ( 0.000000000000000000, -0.000000000000000000, -1.000000000000000000 ) ) ;
#49988 = LINE ( 'NONE', #50580, #16833 ) ;
#49989 = CARTESIAN_POINT ( 'NONE',  ( -66.93407535620586657, 2.602085213965210642E-15, -5.905017180572246005 ) ) ;
#49990 = ORIENTED_EDGE ( 'NONE', *, *, #33239, .T. ) ;
#49991 = CARTESIAN_POINT ( 'NONE',  ( -12.37340416382502539, 4.495856970884011261, 9.066038720008986473 ) ) ;
#49992 = EDGE_CURVE ( 'NONE', #47218, #45990, #21336, .T. ) ;
#49993 = LINE ( 'NONE', #2590, #39056 ) ;
#49994 = AXIS2_PLACEMENT_3D ( 'NONE', #27395, #1269, #31941 ) ;
#49995 = AXIS2_PLACEMENT_3D ( 'NONE', #5378, #48820, #9921 ) ;
#49996 = EDGE_CURVE ( 'NONE', #30649, #54306, #13396, .T. ) ;
#49997 = CARTESIAN_POINT ( 'NONE',  ( -15.88053067323646417, -0.1191753592594197858, 2.950163842912994383 ) ) ;
#49998 = CARTESIAN_POINT ( 'NONE',  ( -16.47913851584194234, 0.000000000000000000, 6.369496994637906973 ) ) ;
#49999 = ADVANCED_FACE ( 'NONE', ( #26706 ), #18177, .T. ) ;
#50000 = CARTESIAN_POINT ( 'NONE',  ( -18.72338561947129065, 5.467268677019013090, 3.780296059854713953 ) ) ;
#50001 = ORIENTED_EDGE ( 'NONE', *, *, #20483, .F. ) ;
#50002 = AXIS2_PLACEMENT_3D ( 'NONE', #47034, #51574, #51832 ) ;
#50003 = ORIENTED_EDGE ( 'NONE', *, *, #53680, .T. ) ;
#50004 = LINE ( 'NONE', #38078, #40444 ) ;
#50005 = LINE ( 'NONE', #41516, #7560 ) ;
#50006 = EDGE_CURVE ( 'NONE', #25279, #3929, #43735, .T. ) ;
#50007 = ORIENTED_EDGE ( 'NONE', *, *, #35845, .F. ) ;
#50008 = CARTESIAN_POINT ( 'NONE',  ( -13.08330893211609869, 0.000000000000000000, 1.763933231766363630 ) ) ;
#50009 = ORIENTED_EDGE ( 'NONE', *, *, #35347, .F. ) ;
#50010 = CARTESIAN_POINT ( 'NONE',  ( -20.54204810873173415, 0.000000000000000000, 4.860550213503115558 ) ) ;
#50011 = VECTOR ( 'NONE', #8435, 999.9999999999998863 ) ;
#50012 = ADVANCED_FACE ( 'NONE', ( #17082 ), #4314, .F. ) ;
#50013 = ORIENTED_EDGE ( 'NONE', *, *, #38039, .T. ) ;
#50014 = ORIENTED_EDGE ( 'NONE', *, *, #54831, .T. ) ;
#50015 = PLANE ( 'NONE',  #39325 ) ;
#50016 = CARTESIAN_POINT ( 'NONE',  ( -18.67619601524082285, 0.000000000000000000, 3.936400510096834893 ) ) ;
#50017 = CARTESIAN_POINT ( 'NONE',  ( -19.32961685222932147, 0.000000000000000000, 14.39908572644263351 ) ) ;
#50018 = EDGE_LOOP ( 'NONE', ( #21195, #25061, #29002, #31278 ) ) ;
#50019 = FACE_OUTER_BOUND ( 'NONE', #52292, .T. ) ;
#50020 = ORIENTED_EDGE ( 'NONE', *, *, #38894, .F. ) ;
#50021 = ORIENTED_EDGE ( 'NONE', *, *, #30945, .T. ) ;
#50022 = EDGE_LOOP ( 'NONE', ( #12040, #44993, #54368, #50026, #17714, #30375, #31209 ) ) ;
#50023 = CARTESIAN_POINT ( 'NONE',  ( -17.62763697264768226, -0.5179957512181538881, 4.379223844503182583 ) ) ;
#50024 = ORIENTED_EDGE ( 'NONE', *, *, #47743, .T. ) ;
#50025 = DIRECTION ( 'NONE',  ( 0.000000000000000000, -1.000000000000000000, 0.000000000000000000 ) ) ;
#50026 = ORIENTED_EDGE ( 'NONE', *, *, #21805, .F. ) ;
#50027 = LINE ( 'NONE', #36428, #3179 ) ;
#50028 = CARTESIAN_POINT ( 'NONE',  ( -16.96808549511456832, 0.000000000000000000, 9.489674468226988679 ) ) ;
#50029 = VECTOR ( 'NONE', #6661, 999.9999999999998863 ) ;
#50030 = VECTOR ( 'NONE', #3750, 999.9999999999998863 ) ;
#50031 = ORIENTED_EDGE ( 'NONE', *, *, #21630, .F. ) ;
#50032 = DIRECTION ( 'NONE',  ( 0.7660212471507180654, -0.6427876096865404731, 0.005961354470445141482 ) ) ;
#50033 = EDGE_CURVE ( 'NONE', #18681, #16694, #38665, .T. ) ;
#50034 = EDGE_LOOP ( 'NONE', ( #10674, #50021, #48764, #8146 ) ) ;
#50035 = DIRECTION ( 'NONE',  ( -0.5449076811759708816, 0.6444004775717707689, 0.5364919789714475140 ) ) ;
#50036 = DIRECTION ( 'NONE',  ( 0.9999697198139515519, 0.000000000000000000, 0.007781995580013368816 ) ) ;
#50037 = VECTOR ( 'NONE', #40374, 1000.000000000000227 ) ;
#50038 = CARTESIAN_POINT ( 'NONE',  ( -18.59083284206345610, 0.000000000000000000, 4.875735021882804610 ) ) ;
#50039 =( NAMED_UNIT ( * ) SI_UNIT ( $, .STERADIAN. ) SOLID_ANGLE_UNIT ( ) );
#50040 = CARTESIAN_POINT ( 'NONE',  ( -12.33850799832341849, 0.000000000000000000, 11.68350162852954632 ) ) ;
#50041 = DIRECTION ( 'NONE',  ( 0.5364919789714477361, 0.6444004775717706579, 0.5449076811759711036 ) ) ;
#50042 = DIRECTION ( 'NONE',  ( 0.005002170337468016433, -0.7660444431189770143, -0.6427681459581293666 ) ) ;
#50043 = ORIENTED_EDGE ( 'NONE', *, *, #32256, .F. ) ;
#50044 = EDGE_CURVE ( 'NONE', #19093, #19489, #5152, .T. ) ;
#50045 = ADVANCED_FACE ( 'NONE', ( #47751 ), #35502, .F. ) ;
#50046 = ORIENTED_EDGE ( 'NONE', *, *, #49936, .T. ) ;
#50047 = CARTESIAN_POINT ( 'NONE',  ( -18.36355258475382612, 0.000000000000000000, 9.678820676885749208 ) ) ;
#50048 = CARTESIAN_POINT ( 'NONE',  ( -13.36006324802803569, 3.524445264749011208, 1.758985750240432022 ) ) ;
#50049 = AXIS2_PLACEMENT_3D ( 'NONE', #39390, #35153, #52448 ) ;
#50050 = CARTESIAN_POINT ( 'NONE',  ( -24.53375310857961367, 18.49370688441070953, -4.657437592157546824 ) ) ;
#50052 = ADVANCED_FACE ( 'NONE', ( #39506 ), #34658, .F. ) ;
#50051 = DIRECTION ( 'NONE',  ( 0.007781995580012662783, 0.000000000000000000, -0.9999697198139514409 ) ) ;
#50053 = CARTESIAN_POINT ( 'NONE',  ( -10.68470108963842868, 0.000000000000000000, 3.998592171460650047 ) ) ;
#50054 = ORIENTED_EDGE ( 'NONE', *, *, #12364, .T. ) ;
#50055 = DIRECTION ( 'NONE',  ( 0.005961354470445682716, -0.6427876096865404731, -0.7660212471507180654 ) ) ;
#50056 = LINE ( 'NONE', #41286, #22335 ) ;
#50057 = ORIENTED_EDGE ( 'NONE', *, *, #14260, .F. ) ;
#50058 = DIRECTION ( 'NONE',  ( 0.007781995580012663651, -3.146120232559066537E-19, -0.9999697198139514409 ) ) ;
#50059 = LINE ( 'NONE', #11738, #19559 ) ;
#50060 = EDGE_LOOP ( 'NONE', ( #55952, #14099, #12758, #34223 ) ) ;
#50061 = LINE ( 'NONE', #14893, #18902 ) ;
#50062 = PLANE ( 'NONE',  #51438 ) ;
#50063 = EDGE_CURVE ( 'NONE', #33161, #29115, #22171, .T. ) ;
#50064 = DIRECTION ( 'NONE',  ( 0.9999697198139515519, 0.000000000000000000, 0.007781995580013368816 ) ) ;
#50065 = VECTOR ( 'NONE', #31605, 1000.000000000000114 ) ;
#50066 = CARTESIAN_POINT ( 'NONE',  ( 2.072287782118878319, 0.000000000000000000, -2.950529333540147015 ) ) ;
#50067 = ADVANCED_FACE ( 'NONE', ( #4848 ), #25888, .F. ) ;
#50068 = CARTESIAN_POINT ( 'NONE',  ( -15.40103151951671734, 0.000000000000000000, 12.95233060667165681 ) ) ;
#50069 = ORIENTED_EDGE ( 'NONE', *, *, #42118, .F. ) ;
#50070 = EDGE_LOOP ( 'NONE', ( #20736, #14455, #11883, #34992 ) ) ;
#50071 = ADVANCED_FACE ( 'NONE', ( #17632 ), #42902, .F. ) ;
#50072 = LINE ( 'NONE', #36772, #26667 ) ;
#50073 = DIRECTION ( 'NONE',  ( 0.007781995580012662783, 0.000000000000000000, -0.9999697198139514409 ) ) ;
#50074 = AXIS2_PLACEMENT_3D ( 'NONE', #52055, #30508, #4638 ) ;
#50075 = DIRECTION ( 'NONE',  ( 0.9999697198139515519, 0.000000000000000000, 0.007781995580013368816 ) ) ;
#50076 = VECTOR ( 'NONE', #11626, 1000.000000000000227 ) ;
#50077 = DIRECTION ( 'NONE',  ( 0.5449076811759707706, 0.6444004775717708799, -0.5364919789714476250 ) ) ;
#50078 = EDGE_CURVE ( 'NONE', #33009, #35551, #47444, .T. ) ;
#50079 = VECTOR ( 'NONE', #29557, 1000.000000000000227 ) ;
#50080 = DIRECTION ( 'NONE',  ( -0.005002170337468016433, -0.7660444431189770143, 0.6427681459581293666 ) ) ;
#50081 = DIRECTION ( 'NONE',  ( -0.9999697198139514409, -0.000000000000000000, -0.007781995580013368816 ) ) ;
#50082 = EDGE_LOOP ( 'NONE', ( #33429, #20455, #39296, #55346 ) ) ;
#50083 = FACE_OUTER_BOUND ( 'NONE', #52917, .T. ) ;
#50084 = FACE_OUTER_BOUND ( 'NONE', #8622, .T. ) ;
#50085 = AXIS2_PLACEMENT_3D ( 'NONE', #12743, #11632, #33223 ) ;
#50086 = LINE ( 'NONE', #24529, #12408 ) ;
#50087 = VECTOR ( 'NONE', #1626, 1000.000000000000227 ) ;
#50088 = VERTEX_POINT ( 'NONE', #38940 ) ;
#50089 = DIRECTION ( 'NONE',  ( 0.9335804264972044075, -0.3583679495452936070, 0.000000000000000000 ) ) ;
#50090 = DIRECTION ( 'NONE',  ( 0.000000000000000000, -0.000000000000000000, -1.000000000000000000 ) ) ;
#50091 = CARTESIAN_POINT ( 'NONE',  ( -18.19747506107908563, 0.000000000000000000, 14.03856424583689311 ) ) ;
#50092 = ORIENTED_EDGE ( 'NONE', *, *, #36228, .T. ) ;
#50093 = CARTESIAN_POINT ( 'NONE',  ( -17.42410023143980879, 0.000000000000000000, 8.378129446685687043 ) ) ;
#50094 = VECTOR ( 'NONE', #52388, 999.9999999999998863 ) ;
#50095 = ORIENTED_EDGE ( 'NONE', *, *, #1682, .T. ) ;
#50096 = ORIENTED_EDGE ( 'NONE', *, *, #51024, .F. ) ;
#50097 = ORIENTED_EDGE ( 'NONE', *, *, #42760, .F. ) ;
#50098 = EDGE_LOOP ( 'NONE', ( #45483, #34661, #17148, #30215 ) ) ;
#50099 = EDGE_LOOP ( 'NONE', ( #17612, #47837, #9400, #48364 ) ) ;
#50100 = LINE ( 'NONE', #28538, #51072 ) ;
#50102 = ADVANCED_FACE ( 'NONE', ( #7 ), #13095, .F. ) ;
#50101 = ORIENTED_EDGE ( 'NONE', *, *, #41489, .F. ) ;
#50103 = ORIENTED_EDGE ( 'NONE', *, *, #46994, .F. ) ;
#50104 = PLANE ( 'NONE',  #32263 ) ;
#50105 = ORIENTED_EDGE ( 'NONE', *, *, #6944, .F. ) ;
#50106 = EDGE_CURVE ( 'NONE', #49029, #51817, #599, .T. ) ;
#50107 = VECTOR ( 'NONE', #52539, 999.9999999999998863 ) ;
#50108 = ORIENTED_EDGE ( 'NONE', *, *, #4124, .T. ) ;
#50109 = EDGE_LOOP ( 'NONE', ( #45352, #54487, #10790, #26503 ) ) ;
#50110 = LINE ( 'NONE', #6994, #17620 ) ;
#50111 = CARTESIAN_POINT ( 'NONE',  ( -15.07217521218155021, 0.000000000000000000, 4.703111972948089914 ) ) ;
#50112 = CARTESIAN_POINT ( 'NONE',  ( 5.223256457478859360, -6.243920421220471972, -1.967953638240999670 ) ) ;
#50113 = CARTESIAN_POINT ( 'NONE',  ( -23.33771345073609638, -0.1191753592594197858, 5.846786880686956955 ) ) ;
#50114 = VECTOR ( 'NONE', #5155, 1000.000000000000000 ) ;
#50115 = CARTESIAN_POINT ( 'NONE',  ( -18.19747506107908563, 0.000000000000000000, 14.03856424583689311 ) ) ;
#50116 = EDGE_LOOP ( 'NONE', ( #6465, #30647, #49147, #51730 ) ) ;
#50117 = ADVANCED_FACE ( 'NONE', ( #21882 ), #52545, .F. ) ;
#50118 = EDGE_CURVE ( 'NONE', #48023, #40238, #41265, .T. ) ;
#50119 = EDGE_CURVE ( 'NONE', #16052, #4269, #6524, .T. ) ;
#50120 = AXIS2_PLACEMENT_3D ( 'NONE', #22026, #34522, #26860 ) ;
#50121 = AXIS2_PLACEMENT_3D ( 'NONE', #29777, #52463, #13295 ) ;
#50122 = ORIENTED_EDGE ( 'NONE', *, *, #22297, .T. ) ;
#50123 = DIRECTION ( 'NONE',  ( 0.007781995580012663651, -3.146120232559066537E-19, -0.9999697198139514409 ) ) ;
#50124 = DIRECTION ( 'NONE',  ( 0.7660212471507180654, -0.6427876096865404731, 0.005961354470445141482 ) ) ;
#50125 = PRODUCT_DEFINITION_CONTEXT ( 'detailed design', #24239, 'design' ) ;
#50126 = EDGE_CURVE ( 'NONE', #6083, #25619, #36346, .T. ) ;
#50127 = CARTESIAN_POINT ( 'NONE',  ( -35.40880390783866716, 12.21499337800758234, -4.897373001089857958 ) ) ;
#50128 = VECTOR ( 'NONE', #31686, 1000.000000000000114 ) ;
#50129 = AXIS2_PLACEMENT_3D ( 'NONE', #11103, #41752, #23887 ) ;
#50130 = LINE ( 'NONE', #45595, #37606 ) ;
#50131 = CARTESIAN_POINT ( 'NONE',  ( -16.53317331066696383, 0.000000000000000000, 13.31285208727739899 ) ) ;
#50132 = DIRECTION ( 'NONE',  ( -0.6246952433987893460, -0.7422098413412802076, 0.2426528472758542054 ) ) ;
#50133 = VERTEX_POINT ( 'NONE', #40629 ) ;
#50134 = LINE ( 'NONE', #41366, #18390 ) ;
#50135 = ORIENTED_EDGE ( 'NONE', *, *, #12209, .T. ) ;
#50136 = FACE_OUTER_BOUND ( 'NONE', #18881, .T. ) ;
#50137 = CARTESIAN_POINT ( 'NONE',  ( -10.07321481412883912, -0.2242460341567873994, 1.060529934425493259 ) ) ;
#50138 = CARTESIAN_POINT ( 'NONE',  ( -23.95238608277258407, 18.82935929325833513, -4.517660165671053996 ) ) ;
#50139 = AXIS2_PLACEMENT_3D ( 'NONE', #5647, #18145, #5950 ) ;
#50140 = CARTESIAN_POINT ( 'NONE',  ( -69.11692417668358246, -9.015782624321049710, -7.493102809087829108 ) ) ;
#50141 = VECTOR ( 'NONE', #160, 1000.000000000000000 ) ;
#50142 = ADVANCED_FACE ( 'NONE', ( #14237 ), #1126, .F. ) ;
#50143 = CARTESIAN_POINT ( 'NONE',  ( -18.67697421479882181, -0.1191753592594197858, 4.036397482078229793 ) ) ;
#50144 = ADVANCED_FACE ( 'NONE', ( #35803 ), #14495, .F. ) ;
#50145 = ORIENTED_EDGE ( 'NONE', *, *, #21847, .F. ) ;
#50146 = ADVANCED_FACE ( 'NONE', ( #10227 ), #45411, .F. ) ;
#50147 = CARTESIAN_POINT ( 'NONE',  ( -16.38920120867433639, -3.432230869623160263, 8.680929647428692775 ) ) ;
#50148 = DIRECTION ( 'NONE',  ( 0.000000000000000000, -1.000000000000000000, 0.000000000000000000 ) ) ;
#50149 = DIRECTION ( 'NONE',  ( -0.5364919789714478471, 0.6444004775717705469, -0.5449076811759709926 ) ) ;
#50150 = VECTOR ( 'NONE', #25151, 1000.000000000000227 ) ;
#50151 = EDGE_CURVE ( 'NONE', #29873, #9919, #19026, .T. ) ;
#50152 = CARTESIAN_POINT ( 'NONE',  ( -25.20200914511100265, -0.1191753592594197858, 6.570942640130446932 ) ) ;
#50153 = LINE ( 'NONE', #33971, #23074 ) ;
#50154 = AXIS2_PLACEMENT_3D ( 'NONE', #23901, #44635, #14303 ) ;
#50155 = DIRECTION ( 'NONE',  ( 0.000000000000000000, -0.000000000000000000, -1.000000000000000000 ) ) ;
#50156 = DIRECTION ( 'NONE',  ( 0.007781995580012663651, 0.000000000000000000, -0.9999697198139515519 ) ) ;
#50157 = EDGE_CURVE ( 'NONE', #6183, #30608, #44868, .T. ) ;
#50158 = CARTESIAN_POINT ( 'NONE',  ( -69.67957132394272435, -8.678494591075715192, -7.555920072494596518 ) ) ;
#50159 = VECTOR ( 'NONE', #50237, 1000.000000000000227 ) ;
#50160 = DIRECTION ( 'NONE',  ( 0.6246952433987894571, -0.7422098413412800966, -0.2426528472758541777 ) ) ;
#50161 = EDGE_LOOP ( 'NONE', ( #28249, #19856, #11515, #1722 ) ) ;
#50162 = VECTOR ( 'NONE', #9137, 999.9999999999998863 ) ;
#50163 = B_SPLINE_CURVE_WITH_KNOTS ( 'NONE', 3,
 ( #2848, #20178, #41221, #19352, #6579, #37515, #54006, #14829, #32979, #28156, #24195, #37227, #41511, #36691 ),
 .UNSPECIFIED., .F., .F.,
 ( 4, 2, 2, 2, 2, 2, 4 ),
 ( 2.976959356410394185E-17, 0.0005795730796964416141, 0.001159146159392853304, 0.001448932699241052427, 0.001738719239089251550, 0.002028505778937450890, 0.002318292318785650230 ),
 .UNSPECIFIED. ) ;
#50164 = VECTOR ( 'NONE', #2079, 1000.000000000000227 ) ;
#50165 = ORIENTED_EDGE ( 'NONE', *, *, #45596, .T. ) ;
#50166 = AXIS2_PLACEMENT_3D ( 'NONE', #46533, #28113, #40890 ) ;
#50167 = ORIENTED_EDGE ( 'NONE', *, *, #18726, .F. ) ;
#50168 = ORIENTED_EDGE ( 'NONE', *, *, #35887, .T. ) ;
#50169 = VECTOR ( 'NONE', #51360, 1000.000000000000227 ) ;
#50170 = ORIENTED_EDGE ( 'NONE', *, *, #1654, .F. ) ;
#50171 = ORIENTED_EDGE ( 'NONE', *, *, #9856, .F. ) ;
#50172 = CARTESIAN_POINT ( 'NONE',  ( 2.072287782118878319, 0.000000000000000000, -2.950529333540147015 ) ) ;
#50173 = DIRECTION ( 'NONE',  ( 0.5449076811759707706, 0.6444004775717708799, -0.5364919789714476250 ) ) ;
#50174 = FACE_OUTER_BOUND ( 'NONE', #30067, .T. ) ;
#50175 = ORIENTED_EDGE ( 'NONE', *, *, #22529, .T. ) ;
#50176 = DIRECTION ( 'NONE',  ( -0.5364919789714478471, 0.6444004775717705469, -0.5449076811759709926 ) ) ;
#50177 = ORIENTED_EDGE ( 'NONE', *, *, #27090, .T. ) ;
#50178 = ORIENTED_EDGE ( 'NONE', *, *, #34890, .F. ) ;
#50179 = CARTESIAN_POINT ( 'NONE',  ( -66.57362299655956406, -8.724013652710414846, 0.6802539881128697452 ) ) ;
#50180 = VECTOR ( 'NONE', #12279, 1000.000000000000227 ) ;
#50181 = CARTESIAN_POINT ( 'NONE',  ( -10.00813838035478298, 0.000000000000000000, 10.77830692922518452 ) ) ;
#50182 = CARTESIAN_POINT ( 'NONE',  ( -16.79925329029790149, 0.000000000000000000, 13.49544742625427496 ) ) ;
#50183 = ORIENTED_EDGE ( 'NONE', *, *, #24102, .F. ) ;
#50184 = LINE ( 'NONE', #23788, #7413 ) ;
#50185 = AXIS2_PLACEMENT_3D ( 'NONE', #26318, #34557, #13551 ) ;
#50186 = ORIENTED_EDGE ( 'NONE', *, *, #32299, .T. ) ;
#50187 = EDGE_CURVE ( 'NONE', #45704, #21256, #27261, .T. ) ;
#50188 = CARTESIAN_POINT ( 'NONE',  ( -10.23599085943975595, 0.000000000000000000, 6.048750543480270636 ) ) ;
#50190 = VECTOR ( 'NONE', #50805, 1000.000000000000227 ) ;
#50189 = FACE_OUTER_BOUND ( 'NONE', #30722, .T. ) ;
#50191 = EDGE_CURVE ( 'NONE', #32397, #37255, #45165, .T. ) ;
#50192 = ADVANCED_FACE ( 'NONE', ( #23308 ), #6266, .F. ) ;
#50193 = LINE ( 'NONE', #6487, #29033 ) ;
#50194 = FACE_OUTER_BOUND ( 'NONE', #28157, .T. ) ;
#50195 = DIRECTION ( 'NONE',  ( 0.5364919789714477361, 0.6444004775717706579, 0.5449076811759711036 ) ) ;
#50196 = LINE ( 'NONE', #1667, #24721 ) ;
#50197 = DIRECTION ( 'NONE',  ( 0.5449076811759707706, 0.6444004775717708799, -0.5364919789714476250 ) ) ;
#50198 = CARTESIAN_POINT ( 'NONE',  ( -19.52429834364018646, 0.000000000000000000, 5.407128660899526373 ) ) ;
#50199 = VECTOR ( 'NONE', #11764, 1000.000000000000227 ) ;
#50200 = FACE_OUTER_BOUND ( 'NONE', #11203, .T. ) ;
#50201 = ORIENTED_EDGE ( 'NONE', *, *, #20362, .T. ) ;
#50202 = DIRECTION ( 'NONE',  ( -0.2588190451025212946, -0.9659258262890680902, 0.000000000000000000 ) ) ;
#50203 = EDGE_LOOP ( 'NONE', ( #40066, #3935, #25559, #52544 ) ) ;
#50204 = AXIS2_PLACEMENT_3D ( 'NONE', #34697, #52016, #39545 ) ;
#50205 = LINE ( 'NONE', #11314, #11097 ) ;
#50206 = DIRECTION ( 'NONE',  ( -0.9999697198139514409, -0.000000000000000000, -0.007781995580013368816 ) ) ;
#50207 = LINE ( 'NONE', #50511, #3271 ) ;
#50208 = PLANE ( 'NONE',  #44092 ) ;
#50209 = DIRECTION ( 'NONE',  ( 0.007781995580012663651, -3.146120232559066537E-19, -0.9999697198139514409 ) ) ;
#50210 = AXIS2_PLACEMENT_3D ( 'NONE', #31698, #40201, #1596 ) ;
#50211 = DIRECTION ( 'NONE',  ( 0.000000000000000000, 1.000000000000000000, 0.000000000000000000 ) ) ;
#50212 = VECTOR ( 'NONE', #12938, 1000.000000000000227 ) ;
#50213 = ORIENTED_EDGE ( 'NONE', *, *, #38620, .T. ) ;
#50214 = CARTESIAN_POINT ( 'NONE',  ( -25.20123094555300369, 0.000000000000000000, 6.470945668149052032 ) ) ;
#50215 = CARTESIAN_POINT ( 'NONE',  ( -21.80678505063549011, 3.038739411681508518, 5.055475909915189803 ) ) ;
#50216 = DIRECTION ( 'NONE',  ( 0.005002170337468016433, -0.7660444431189770143, -0.6427681459581293666 ) ) ;
#50217 = DIRECTION ( 'NONE',  ( -0.5449076811759708816, 0.6444004775717707689, 0.5364919789714475140 ) ) ;
#50218 = DIRECTION ( 'NONE',  ( -0.005961354470445682716, -0.6427876096865404731, 0.7660212471507180654 ) ) ;
#50219 = LINE ( 'NONE', #7935, #36394 ) ;
#50220 = DIRECTION ( 'NONE',  ( 0.005002170337468016433, -0.7660444431189770143, -0.6427681459581293666 ) ) ;
#50221 = ADVANCED_FACE ( 'NONE', ( #9691 ), #19294, .F. ) ;
#50222 = DIRECTION ( 'NONE',  ( 0.007781995580012662783, 0.000000000000000000, -0.9999697198139514409 ) ) ;
#50223 = CARTESIAN_POINT ( 'NONE',  ( -9.075990533167328067, 0.000000000000000000, 10.41622904950343909 ) ) ;
#50224 = VERTEX_POINT ( 'NONE', #36633 ) ;
#50225 = CARTESIAN_POINT ( 'NONE',  ( -11.37232435848456191, 0.000000000000000000, 6.947897486638751730 ) ) ;
#50226 = EDGE_LOOP ( 'NONE', ( #3969, #28761, #25413, #27576, #20865 ) ) ;
#50227 = VECTOR ( 'NONE', #30140, 1000.000000000000227 ) ;
#50228 = ADVANCED_FACE ( 'NONE', ( #53946 ), #15062, .F. ) ;
#50229 = DIRECTION ( 'NONE',  ( -0.3620778797217455991, 0.000000000000000000, -0.9321478471874540261 ) ) ;
#50230 = LINE ( 'NONE', #52890, #40076 ) ;
#50231 = EDGE_CURVE ( 'NONE', #21366, #26301, #49699, .T. ) ;
#50232 = VECTOR ( 'NONE', #11160, 1000.000000000000000 ) ;
#50233 = ORIENTED_EDGE ( 'NONE', *, *, #46552, .F. ) ;
#50234 = ADVANCED_FACE ( 'NONE', ( #54228 ), #27006, .F. ) ;
#50235 = VECTOR ( 'NONE', #47924, 1000.000000000000114 ) ;
#50236 = ORIENTED_EDGE ( 'NONE', *, *, #56053, .F. ) ;
#50237 = DIRECTION ( 'NONE',  ( 0.007781995580012662783, 0.000000000000000000, -0.9999697198139514409 ) ) ;
#50238 = ORIENTED_EDGE ( 'NONE', *, *, #3418, .F. ) ;
#50239 = ORIENTED_EDGE ( 'NONE', *, *, #29371, .F. ) ;
#50240 = VERTEX_POINT ( 'NONE', #36096 ) ;
#50241 = PLANE ( 'NONE',  #51062 ) ;
#50242 = VECTOR ( 'NONE', #33552, 999.9999999999998863 ) ;
#50243 = CARTESIAN_POINT ( 'NONE',  ( -66.59956646452421580, -9.331851097499329839, -6.325180979151075356 ) ) ;
#50244 = DIRECTION ( 'NONE',  ( -0.7660212471507179544, -0.6427876096865405842, -0.005961354470445141482 ) ) ;
#50245 = AXIS2_PLACEMENT_3D ( 'NONE', #35764, #22974, #14199 ) ;
#50246 = ORIENTED_EDGE ( 'NONE', *, *, #10194, .F. ) ;
#50247 = EDGE_LOOP ( 'NONE', ( #32103, #30713, #24202, #28752 ) ) ;
#50248 = VECTOR ( 'NONE', #18381, 1000.000000000000227 ) ;
#50249 = VECTOR ( 'NONE', #55829, 1000.000000000000000 ) ;
#50250 = LINE ( 'NONE', #42006, #50190 ) ;
#50251 = CARTESIAN_POINT ( 'NONE',  ( -13.46921766719642122, -1.651309408375655874, 4.623913353405106008 ) ) ;
#50252 = ORIENTED_EDGE ( 'NONE', *, *, #26319, .F. ) ;
#50253 = CARTESIAN_POINT ( 'NONE',  ( -17.36532418587302473, -0.1191753592594177458, 13.67570816655714516 ) ) ;
#50254 = EDGE_CURVE ( 'NONE', #29163, #441, #51303, .T. ) ;
#50255 = EDGE_LOOP ( 'NONE', ( #32916, #41624, #13034, #1063 ) ) ;
#50256 = CARTESIAN_POINT ( 'NONE',  ( 5.421104749901517472, -1.072937963535797179, 2.456654125669141209 ) ) ;
#50257 = LINE ( 'NONE', #36659, #24904 ) ;
#50259 = EDGE_LOOP ( 'NONE', ( #34850, #45870, #1012, #12798 ) ) ;
#50258 = EDGE_CURVE ( 'NONE', #14573, #21242, #46448, .T. ) ;
#50260 = DIRECTION ( 'NONE',  ( -0.005002170337468016433, -0.7660444431189770143, 0.6427681459581293666 ) ) ;
#50261 = EDGE_CURVE ( 'NONE', #33384, #18589, #21761, .T. ) ;
#50262 = EDGE_CURVE ( 'NONE', #51823, #11765, #21328, .T. ) ;
#50263 = VECTOR ( 'NONE', #44757, 1000.000000000000000 ) ;
#50264 = DIRECTION ( 'NONE',  ( 0.000000000000000000, 1.000000000000000000, 0.000000000000000000 ) ) ;
#50265 = VERTEX_POINT ( 'NONE', #47603 ) ;
#50266 = CARTESIAN_POINT ( 'NONE',  ( -16.41880516715173144, -0.1941918491731536578, 3.378255151246715826 ) ) ;
#50267 = VECTOR ( 'NONE', #46859, 1000.000000000000227 ) ;
#50268 = CARTESIAN_POINT ( 'NONE',  ( -17.39248564288169874, 0.000000000000000000, 4.315722710850279142 ) ) ;
#50269 = EDGE_LOOP ( 'NONE', ( #23628, #24808, #34065, #51198 ) ) ;
#50270 = VECTOR ( 'NONE', #38404, 1000.000000000000000 ) ;
#50271 = DIRECTION ( 'NONE',  ( 0.000000000000000000, -1.000000000000000000, 0.000000000000000000 ) ) ;
#50272 = LINE ( 'NONE', #55656, #10621 ) ;
#50273 = FACE_OUTER_BOUND ( 'NONE', #15827, .T. ) ;
#50274 = LINE ( 'NONE', #15106, #17754 ) ;
#50275 = LINE ( 'NONE', #11388, #10432 ) ;
#50276 = CARTESIAN_POINT ( 'NONE',  ( -27.06708303904391144, 0.000000000000000000, 7.395095371555332697 ) ) ;
#50277 = EDGE_CURVE ( 'NONE', #34543, #43670, #50992, .T. ) ;
#50278 = CARTESIAN_POINT ( 'NONE',  ( -16.49129718093630004, -2.460819163488158878, 7.126335086546274233 ) ) ;
#50279 = VECTOR ( 'NONE', #13494, 1000.000000000000227 ) ;
#50280 = ORIENTED_EDGE ( 'NONE', *, *, #28036, .T. ) ;
#50281 =( NAMED_UNIT ( * ) PLANE_ANGLE_UNIT ( ) SI_UNIT ( $, .RADIAN. ) );
#50282 = DIRECTION ( 'NONE',  ( 0.007781995580012662783, 0.000000000000000000, -0.9999697198139514409 ) ) ;
#50283 = CARTESIAN_POINT ( 'NONE',  ( -67.69264396058785849, 5.362719954027564582E-12, -5.540714948658928662 ) ) ;
#50284 = ORIENTED_EDGE ( 'NONE', *, *, #36546, .F. ) ;
#50285 = VECTOR ( 'NONE', #13039, 1000.000000000000227 ) ;
#50286 = DIRECTION ( 'NONE',  ( 0.007781995580012663651, -3.146120232559066537E-19, -0.9999697198139514409 ) ) ;
#50287 = FACE_OUTER_BOUND ( 'NONE', #40828, .T. ) ;
#50288 = VECTOR ( 'NONE', #20544, 1000.000000000000000 ) ;
#50289 = LINE ( 'NONE', #45748, #44910 ) ;
#50290 = DIRECTION ( 'NONE',  ( -0.5449076811759708816, 0.6444004775717707689, 0.5364919789714475140 ) ) ;
#50291 = DIRECTION ( 'NONE',  ( 0.9999697198139515519, 0.000000000000000000, 0.007781995580013368816 ) ) ;
#50292 = ORIENTED_EDGE ( 'NONE', *, *, #12982, .T. ) ;
#50293 = VECTOR ( 'NONE', #3785, 1000.000000000000114 ) ;
#50294 = VECTOR ( 'NONE', #47095, 999.9999999999998863 ) ;
#50295 = VERTEX_POINT ( 'NONE', #3862 ) ;
#50296 = DIRECTION ( 'NONE',  ( 0.000000000000000000, -0.000000000000000000, -1.000000000000000000 ) ) ;
#50297 = CARTESIAN_POINT ( 'NONE',  ( -15.13495153988577968, 0.000000000000000000, 12.76973526769478084 ) ) ;
#50298 = CARTESIAN_POINT ( 'NONE',  ( -15.47473988553288038, -0.1159828484229817602, 9.229288071583351183 ) ) ;
#50299 = VERTEX_POINT ( 'NONE', #12955 ) ;
#50300 = LINE ( 'NONE', #38363, #40379 ) ;
#50301 = EDGE_CURVE ( 'NONE', #44396, #1167, #34531, .T. ) ;
#50302 = ORIENTED_EDGE ( 'NONE', *, *, #825, .F. ) ;
#50303 = DIRECTION ( 'NONE',  ( 0.000000000000000000, 0.000000000000000000, 1.000000000000000000 ) ) ;
#50304 = VECTOR ( 'NONE', #35488, 1000.000000000000227 ) ;
#50305 = EDGE_LOOP ( 'NONE', ( #3389, #56148, #37798, #12622 ) ) ;
#50306 = ORIENTED_EDGE ( 'NONE', *, *, #15636, .F. ) ;
#50307 = VECTOR ( 'NONE', #10699, 1000.000000000000227 ) ;
#50308 = LINE ( 'NONE', #11957, #32073 ) ;
#50309 = CARTESIAN_POINT ( 'NONE',  ( -23.66772770479517618, 18.99370688441070953, -4.503111145262439052 ) ) ;
#50310 = VECTOR ( 'NONE', #419, 1000.000000000000227 ) ;
#50311 = LINE ( 'NONE', #28755, #35749 ) ;
#50312 = ADVANCED_FACE ( 'NONE', ( #20648 ), #51841, .F. ) ;
#50313 = ORIENTED_EDGE ( 'NONE', *, *, #15953, .T. ) ;
#50314 = CARTESIAN_POINT ( 'NONE',  ( -58.00000000000000711, -9.250000000000000000, 7.102951435054649637E-15 ) ) ;
#50315 = AXIS2_PLACEMENT_3D ( 'NONE', #17593, #4808, #48232 ) ;
#50316 = ORIENTED_EDGE ( 'NONE', *, *, #1072, .T. ) ;
#50317 = EDGE_CURVE ( 'NONE', #8089, #54118, #42758, .T. ) ;
#50318 = EDGE_CURVE ( 'NONE', #39727, #38353, #38814, .T. ) ;
#50319 = ORIENTED_EDGE ( 'NONE', *, *, #30721, .T. ) ;
#50320 = ORIENTED_EDGE ( 'NONE', *, *, #7502, .F. ) ;
#50321 = AXIS2_PLACEMENT_3D ( 'NONE', #4226, #25237, #30330 ) ;
#50322 = FACE_OUTER_BOUND ( 'NONE', #2120, .T. ) ;
#50323 = AXIS2_PLACEMENT_3D ( 'NONE', #41817, #15699, #11731 ) ;
#50324 = PLANE ( 'NONE',  #24031 ) ;
#50325 = ORIENTED_EDGE ( 'NONE', *, *, #21286, .F. ) ;
#50326 = VECTOR ( 'NONE', #17746, 999.9999999999998863 ) ;
#50327 = DIRECTION ( 'NONE',  ( 0.9999697198139515519, 0.000000000000000000, 0.007781995580013368816 ) ) ;
#50328 = EDGE_CURVE ( 'NONE', #4025, #42332, #8722, .T. ) ;
#50329 = ORIENTED_EDGE ( 'NONE', *, *, #32481, .T. ) ;
#50330 = LINE ( 'NONE', #32720, #53936 ) ;
#50331 = CARTESIAN_POINT ( 'NONE',  ( -12.91584975057942941, -1.003701604285655469, 3.346131726335665579 ) ) ;
#50332 = AXIS2_PLACEMENT_3D ( 'NONE', #13967, #18504, #14531 ) ;
#50333 = ORIENTED_EDGE ( 'NONE', *, *, #38781, .F. ) ;
#50334 = ADVANCED_FACE ( 'NONE', ( #4450 ), #11822, .F. ) ;
#50335 = DIRECTION ( 'NONE',  ( -0.6427681459581293666, -0.7660444431189770143, -0.005002170337467561935 ) ) ;
#50336 = EDGE_LOOP ( 'NONE', ( #49711, #17163, #28367, #32436 ) ) ;
#50337 = EDGE_CURVE ( 'NONE', #38002, #47502, #12682, .T. ) ;
#50338 = AXIS2_PLACEMENT_3D ( 'NONE', #31809, #48861, #10797 ) ;
#50339 = CARTESIAN_POINT ( 'NONE',  ( -15.65072360821981334, 2.876837460659007473, 7.681974050944107013 ) ) ;
#50340 = VECTOR ( 'NONE', #33118, 999.9999999999998863 ) ;
#50341 = CARTESIAN_POINT ( 'NONE',  ( -27.22333567087903461, 16.65220053346459750, -4.657437592157546824 ) ) ;
#50342 = LINE ( 'NONE', #50627, #35038 ) ;
#50343 = PRESENTATION_STYLE_ASSIGNMENT (( #53239 ) ) ;
#50344 = DIRECTION ( 'NONE',  ( -0.005002170337468016433, -0.7660444431189770143, 0.6427681459581293666 ) ) ;
#50345 = DIRECTION ( 'NONE',  ( 0.9999697198139515519, 0.000000000000000000, 0.007781995580013368816 ) ) ;
#50346 = ORIENTED_EDGE ( 'NONE', *, *, #135, .T. ) ;
#50347 = EDGE_CURVE ( 'NONE', #4182, #43916, #55267, .T. ) ;
#50348 = ORIENTED_EDGE ( 'NONE', *, *, #1798, .F. ) ;
#50349 = CARTESIAN_POINT ( 'NONE',  ( 2.072287782118878319, 0.000000000000000000, -2.950529333540147015 ) ) ;
#50350 = LINE ( 'NONE', #6931, #25764 ) ;
#50351 = CARTESIAN_POINT ( 'NONE',  ( -22.40556560354864146, -0.1191753592594197858, 5.484709000965211523 ) ) ;
#50352 = DIRECTION ( 'NONE',  ( -0.005002170337468016433, -0.7660444431189770143, 0.6427681459581293666 ) ) ;
#50353 = LINE ( 'NONE', #49798, #10686 ) ;
#50354 = VECTOR ( 'NONE', #42489, 999.9999999999998863 ) ;
#50355 = EDGE_CURVE ( 'NONE', #44511, #39352, #29438, .T. ) ;
#50356 = DIRECTION ( 'NONE',  ( 0.6427681459581294776, -0.7660444431189769032, 0.005002170337467562802 ) ) ;
#50357 = ORIENTED_EDGE ( 'NONE', *, *, #30669, .F. ) ;
#50358 = AXIS2_PLACEMENT_3D ( 'NONE', #29273, #51135, #38357 ) ;
#50359 = DIRECTION ( 'NONE',  ( 0.000000000000000000, -0.000000000000000000, -1.000000000000000000 ) ) ;
#50360 = CARTESIAN_POINT ( 'NONE',  ( -15.13495153988577968, 0.000000000000000000, 12.76973526769478084 ) ) ;
#50361 = ORIENTED_EDGE ( 'NONE', *, *, #46294, .F. ) ;
#50362 = DIRECTION ( 'NONE',  ( -0.5364919789714478471, 0.6444004775717705469, -0.5449076811759709926 ) ) ;
#50363 = DIRECTION ( 'NONE',  ( 0.007781995580012662783, 0.000000000000000000, -0.9999697198139514409 ) ) ;
#50364 = VECTOR ( 'NONE', #41064, 1000.000000000000227 ) ;
#50365 = EDGE_LOOP ( 'NONE', ( #23919, #33106, #52434, #15810 ) ) ;
#50366 = CARTESIAN_POINT ( 'NONE',  ( -25.20278734466900517, 0.000000000000000000, 6.670939612111840944 ) ) ;
#50367 = LINE ( 'NONE', #19716, #45087 ) ;
#50368 = VECTOR ( 'NONE', #21530, 999.9999999999998863 ) ;
#50369 = FACE_OUTER_BOUND ( 'NONE', #23421, .T. ) ;
#50370 = CARTESIAN_POINT ( 'NONE',  ( -13.50659957395150812, -1.165603555308157846, 2.090554221737622953 ) ) ;
#50371 = LINE ( 'NONE', #23430, #51900 ) ;
#50372 = B_SPLINE_CURVE_WITH_KNOTS ( 'NONE', 3,
 ( #8905, #26208, #39254, #51496 ),
 .UNSPECIFIED., .F., .F.,
 ( 4, 4 ),
 ( 3.934737272476643706E-05, 0.0004522109935135529301 ),
 .UNSPECIFIED. ) ;
#50373 = ORIENTED_EDGE ( 'NONE', *, *, #3144, .T. ) ;
#50374 = VECTOR ( 'NONE', #35000, 999.9999999999998863 ) ;
#50375 = VECTOR ( 'NONE', #48944, 1000.000000000000227 ) ;
#50376 = ORIENTED_EDGE ( 'NONE', *, *, #25043, .F. ) ;
#50377 = DIRECTION ( 'NONE',  ( -0.5449076811759708816, 0.6444004775717707689, 0.5364919789714475140 ) ) ;
#50378 = DIRECTION ( 'NONE',  ( -0.005002170337468016433, -0.7660444431189770143, 0.6427681459581293666 ) ) ;
#50379 = CARTESIAN_POINT ( 'NONE',  ( -14.40622671698839774, 0.000000000000000000, 4.538968524537128069 ) ) ;
#50380 = VECTOR ( 'NONE', #55592, 1000.000000000000227 ) ;
#50381 = CARTESIAN_POINT ( 'NONE',  ( -27.06630483948590893, -0.1191753592594197858, 7.295098399573937797 ) ) ;
#50383 = DIRECTION ( 'NONE',  ( 0.9999697198139515519, 0.000000000000000000, 0.007781995580013368816 ) ) ;
#50382 = VECTOR ( 'NONE', #53738, 1000.000000000000227 ) ;
#50384 = DIRECTION ( 'NONE',  ( 0.5364919789714477361, 0.6444004775717706579, 0.5449076811759711036 ) ) ;
#50385 = EDGE_CURVE ( 'NONE', #31029, #47959, #38222, .T. ) ;
#50386 = VERTEX_POINT ( 'NONE', #55843 ) ;
#50387 = CARTESIAN_POINT ( 'NONE',  ( -27.06630483948590893, -0.1191753592594197858, 7.295098399573937797 ) ) ;
#50388 = VECTOR ( 'NONE', #41023, 999.9999999999998863 ) ;
#50389 = LINE ( 'NONE', #27590, #36005 ) ;
#50390 = VECTOR ( 'NONE', #52590, 999.9999999999998863 ) ;
#50391 = CARTESIAN_POINT ( 'NONE',  ( -13.07066190154808361, 0.000000000000000000, 12.04713590736729678 ) ) ;
#50392 = ORIENTED_EDGE ( 'NONE', *, *, #45431, .T. ) ;
#50393 = CARTESIAN_POINT ( 'NONE',  ( -69.24055593166185929, -10.33124374485395514, 7.498947595741733529 ) ) ;
#50394 = CARTESIAN_POINT ( 'NONE',  ( -22.03895444026947104, 19.66185708466576187, 4.421688969255889390 ) ) ;
#50395 = LINE ( 'NONE', #10928, #41129 ) ;
#50396 = ORIENTED_EDGE ( 'NONE', *, *, #13920, .F. ) ;
#50397 = DIRECTION ( 'NONE',  ( -0.005961354470445682716, -0.6427876096865404731, 0.7660212471507180654 ) ) ;
#50398 = ORIENTED_EDGE ( 'NONE', *, *, #27490, .F. ) ;
#50399 = ADVANCED_FACE ( 'NONE', ( #42499 ), #29993, .F. ) ;
#50400 = VECTOR ( 'NONE', #21028, 1000.000000000000227 ) ;
#50401 = ORIENTED_EDGE ( 'NONE', *, *, #50277, .T. ) ;
#50402 = ORIENTED_EDGE ( 'NONE', *, *, #51759, .T. ) ;
#50403 = ORIENTED_EDGE ( 'NONE', *, *, #26730, .T. ) ;
#50404 = AXIS2_PLACEMENT_3D ( 'NONE', #45688, #41160, #2254 ) ;
#50405 = ORIENTED_EDGE ( 'NONE', *, *, #17536, .F. ) ;
#50406 = DIRECTION ( 'NONE',  ( 0.6427681459581294776, -0.7660444431189769032, 0.005002170337467562802 ) ) ;
#50407 = AXIS2_PLACEMENT_3D ( 'NONE', #12653, #30254, #3294 ) ;
#50408 = EDGE_LOOP ( 'NONE', ( #1756, #21744, #28282, #5469 ) ) ;
#50409 = VERTEX_POINT ( 'NONE', #56126 ) ;
#50410 = ADVANCED_FACE ( 'NONE', ( #16952 ), #34277, .F. ) ;
#50411 = EDGE_LOOP ( 'NONE', ( #12824, #43569, #56128, #8161 ) ) ;
#50412 = AXIS2_PLACEMENT_3D ( 'NONE', #30993, #52856, #23346 ) ;
#50413 = ORIENTED_EDGE ( 'NONE', *, *, #47261, .F. ) ;
#50414 = EDGE_CURVE ( 'NONE', #13801, #17105, #9835, .T. ) ;
#50415 = AXIS2_PLACEMENT_3D ( 'NONE', #40303, #27826, #40856 ) ;
#50416 = VECTOR ( 'NONE', #27659, 999.9999999999998863 ) ;
#50417 = DIRECTION ( 'NONE',  ( 0.7660212471507180654, -0.6427876096865404731, 0.005961354470445141482 ) ) ;
#50418 = CARTESIAN_POINT ( 'NONE',  ( -8.653915872335209869, -10.43490457594507781, 6.579848388698870565 ) ) ;
#50419 = CARTESIAN_POINT ( 'NONE',  ( -25.20278734466900517, 0.000000000000000000, 6.670939612111840944 ) ) ;
#50420 = DIRECTION ( 'NONE',  ( -0.5449076811759708816, 0.6444004775717707689, 0.5364919789714475140 ) ) ;
#50421 = ORIENTED_EDGE ( 'NONE', *, *, #20271, .F. ) ;
#50422 = DIRECTION ( 'NONE',  ( 0.5449076811759707706, 0.6444004775717708799, -0.5364919789714476250 ) ) ;
#50423 = ORIENTED_EDGE ( 'NONE', *, *, #44605, .T. ) ;
#50424 = VECTOR ( 'NONE', #24874, 999.9999999999998863 ) ;
#50425 = EDGE_CURVE ( 'NONE', #27945, #51378, #54625, .T. ) ;
#50426 = EDGE_LOOP ( 'NONE', ( #26186, #6535, #31567, #49965, #6832 ) ) ;
#50427 = VECTOR ( 'NONE', #1020, 1000.000000000000114 ) ;
#50428 = CARTESIAN_POINT ( 'NONE',  ( -10.94028622754223967, 0.000000000000000000, 11.14038480894692995 ) ) ;
#50429 = FACE_OUTER_BOUND ( 'NONE', #45107, .T. ) ;
#50430 = AXIS2_PLACEMENT_3D ( 'NONE', #19926, #40418, #19088 ) ;
#50431 = CARTESIAN_POINT ( 'NONE',  ( -19.63691669459172928, -5.051250379848162275, 12.59953947454578760 ) ) ;
#50432 = EDGE_CURVE ( 'NONE', #16632, #46605, #14091, .T. ) ;
#50433 = VECTOR ( 'NONE', #54404, 999.9999999999998863 ) ;
#50434 = FACE_OUTER_BOUND ( 'NONE', #2675, .T. ) ;
#50435 = LINE ( 'NONE', #28567, #32196 ) ;
#50436 = DIRECTION ( 'NONE',  ( -0.6427681459581293666, -0.7660444431189770143, -0.005002170337467561935 ) ) ;
#50437 = EDGE_LOOP ( 'NONE', ( #4695, #33929, #30706, #21597 ) ) ;
#50438 = FACE_OUTER_BOUND ( 'NONE', #45856, .T. ) ;
#50439 = ORIENTED_EDGE ( 'NONE', *, *, #27529, .F. ) ;
#50440 = CARTESIAN_POINT ( 'NONE',  ( -13.53673582514181106, 0.000000000000000000, 12.22817484722816772 ) ) ;
#50441 = DIRECTION ( 'NONE',  ( -0.005002170337468016433, -0.7660444431189770143, 0.6427681459581293666 ) ) ;
#50442 = LINE ( 'NONE', #11802, #34470 ) ;
#50443 = LINE ( 'NONE', #15784, #44015 ) ;
#50444 = DIRECTION ( 'NONE',  ( -0.9999697198139514409, -0.000000000000000000, -0.007781995580013368816 ) ) ;
#50445 = VECTOR ( 'NONE', #13518, 1000.000000000000000 ) ;
#50446 = ORIENTED_EDGE ( 'NONE', *, *, #31707, .F. ) ;
#50447 = ORIENTED_EDGE ( 'NONE', *, *, #9836, .F. ) ;
#50448 = DIRECTION ( 'NONE',  ( 0.007781995580012663651, -3.146120232559066537E-19, -0.9999697198139514409 ) ) ;
#50449 = CARTESIAN_POINT ( 'NONE',  ( -28.92982233430281980, 0.000000000000000000, 7.919257187036034651 ) ) ;
#50450 = CARTESIAN_POINT ( 'NONE',  ( -18.33193799619571962, 0.000000000000000000, 5.616413941050340419 ) ) ;
#50451 = VECTOR ( 'NONE', #30755, 1000.000000000000000 ) ;
#50452 = ADVANCED_FACE ( 'NONE', ( #26292 ), #5005, .F. ) ;
#50453 = PLANE ( 'NONE',  #8301 ) ;
#50454 = VECTOR ( 'NONE', #29511, 999.9999999999998863 ) ;
#50455 = FACE_OUTER_BOUND ( 'NONE', #34150, .T. ) ;
#50456 = ADVANCED_FACE ( 'NONE', ( #5846 ), #22870, .F. ) ;
#50457 = CARTESIAN_POINT ( 'NONE',  ( -8.409922665610809034, 0.000000000000000000, 10.23674650875856962 ) ) ;
#50458 = CARTESIAN_POINT ( 'NONE',  ( 2.072287782118878319, 0.000000000000000000, -2.950529333540147015 ) ) ;
#50459 = AXIS2_PLACEMENT_3D ( 'NONE', #20322, #33404, #3300 ) ;
#50460 = CARTESIAN_POINT ( 'NONE',  ( -14.66887761629205222, 0.000000000000000000, 12.58869632783390990 ) ) ;
#50461 = EDGE_CURVE ( 'NONE', #43270, #30420, #52680, .T. ) ;
#50462 = LINE ( 'NONE', #52678, #20163 ) ;
#50463 = ADVANCED_FACE ( 'NONE', ( #22606 ), #17793, .F. ) ;
#50464 = VECTOR ( 'NONE', #5874, 1000.000000000000227 ) ;
#50465 = EDGE_CURVE ( 'NONE', #43561, #12378, #53285, .T. ) ;
#50466 = ADVANCED_FACE ( 'NONE', ( #52428 ), #14376, .F. ) ;
#50467 = ORIENTED_EDGE ( 'NONE', *, *, #27030, .T. ) ;
#50468 = AXIS2_PLACEMENT_3D ( 'NONE', #50951, #29395, #7835 ) ;
#50469 = VECTOR ( 'NONE', #13267, 1000.000000000000227 ) ;
#50470 = ORIENTED_EDGE ( 'NONE', *, *, #40726, .T. ) ;
#50471 = VECTOR ( 'NONE', #34446, 999.9999999999998863 ) ;
#50472 = VERTEX_POINT ( 'NONE', #40498 ) ;
#50473 = EDGE_LOOP ( 'NONE', ( #43250, #19045, #624, #31821 ) ) ;
#50474 = ORIENTED_EDGE ( 'NONE', *, *, #34325, .F. ) ;
#50475 = CARTESIAN_POINT ( 'NONE',  ( -17.70023939833923521, 0.000000000000000000, 9.853308747064737361 ) ) ;
#50476 = CARTESIAN_POINT ( 'NONE',  ( -12.65839411606857823, -0.1191753592594179401, 5.929895813100822366 ) ) ;
#50477 = LINE ( 'NONE', #30599, #37608 ) ;
#50478 = VERTEX_POINT ( 'NONE', #35659 ) ;
#50479 = LINE ( 'NONE', #33437, #9559 ) ;
#50480 = EDGE_CURVE ( 'NONE', #9219, #40728, #22033, .T. ) ;
#50481 = ORIENTED_EDGE ( 'NONE', *, *, #21447, .T. ) ;
#50482 = CARTESIAN_POINT ( 'NONE',  ( -19.86442598447069585, 1.771796430571655145, 6.503047446853179814 ) ) ;
#50483 = EDGE_LOOP ( 'NONE', ( #52819, #6801, #52820, #26412 ) ) ;
#50484 = VECTOR ( 'NONE', #18435, 1000.000000000000000 ) ;
#50485 = EDGE_CURVE ( 'NONE', #12432, #43913, #1586, .T. ) ;
#50486 = CARTESIAN_POINT ( 'NONE',  ( -67.12594105347433526, -9.392212684426485936, 7.224227263220592832 ) ) ;
#50487 = EDGE_CURVE ( 'NONE', #36594, #22669, #48994, .T. ) ;
#50488 = LINE ( 'NONE', #20071, #8280 ) ;
#50489 = LINE ( 'NONE', #28903, #42280 ) ;
#50490 = ORIENTED_EDGE ( 'NONE', *, *, #42608, .T. ) ;
#50491 = DIRECTION ( 'NONE',  ( -0.7660212471507179544, -0.6427876096865405842, -0.005961354470445141482 ) ) ;
#50492 = ORIENTED_EDGE ( 'NONE', *, *, #46179, .T. ) ;
#50493 = EDGE_CURVE ( 'NONE', #45245, #46200, #9248, .T. ) ;
#50494 = FACE_OUTER_BOUND ( 'NONE', #36650, .T. ) ;
#50495 = VECTOR ( 'NONE', #54357, 999.9999999999998863 ) ;
#50496 = CARTESIAN_POINT ( 'NONE',  ( -18.67775241435682432, 0.000000000000000000, 4.136394454059623804 ) ) ;
#50497 = EDGE_CURVE ( 'NONE', #27027, #8286, #52136, .T. ) ;
#50498 = CARTESIAN_POINT ( 'NONE',  ( -27.99845268667336384, -0.1191753592594197858, 7.657176279295684118 ) ) ;
#50499 = VECTOR ( 'NONE', #12007, 999.9999999999998863 ) ;
#50500 = LINE ( 'NONE', #55295, #6841 ) ;
#50501 = PLANE ( 'NONE',  #29266 ) ;
#50502 = CARTESIAN_POINT ( 'NONE',  ( -14.97381569168726756, 0.4483081953215047322, 3.433409769016318780 ) ) ;
#50503 = LINE ( 'NONE', #37724, #26652 ) ;
#50504 = PLANE ( 'NONE',  #41970 ) ;
#50505 = ORIENTED_EDGE ( 'NONE', *, *, #26454, .F. ) ;
#50506 = DIRECTION ( 'NONE',  ( 0.7660212471507180654, -0.6427876096865404731, 0.005961354470445141482 ) ) ;
#50507 = ORIENTED_EDGE ( 'NONE', *, *, #30371, .T. ) ;
#50508 = VECTOR ( 'NONE', #15294, 1000.000000000000000 ) ;
#50509 = LINE ( 'NONE', #1933, #4784 ) ;
#50510 = CARTESIAN_POINT ( 'NONE',  ( -13.53673582514181106, 0.000000000000000000, 12.22817484722816772 ) ) ;
#50511 = CARTESIAN_POINT ( 'NONE',  ( -14.64608374724779161, 0.6102101463440037232, 3.571816235922804950 ) ) ;
#50512 = LINE ( 'NONE', #10504, #15075 ) ;
#50513 = LINE ( 'NONE', #24642, #37657 ) ;
#50514 = VECTOR ( 'NONE', #39832, 1000.000000000000114 ) ;
#50515 = CARTESIAN_POINT ( 'NONE',  ( -24.27063949748155380, 0.000000000000000000, 6.308861732390097288 ) ) ;
#50516 = DIRECTION ( 'NONE',  ( -1.021680238921689289E-15, 3.490776269985572895E-16, 0.9999999999999998890 ) ) ;
#50517 = VERTEX_POINT ( 'NONE', #13253 ) ;
#50518 = DIRECTION ( 'NONE',  ( 0.007781995580012663651, -3.146120232559066537E-19, -0.9999697198139514409 ) ) ;
#50519 = PLANE ( 'NONE',  #42924 ) ;
#50520 = DIRECTION ( 'NONE',  ( 0.007781995580012663651, -3.146120232559066537E-19, -0.9999697198139514409 ) ) ;
#50521 = DIRECTION ( 'NONE',  ( -0.005961354470445682716, -0.6427876096865404731, 0.7660212471507180654 ) ) ;
#50522 = LINE ( 'NONE', #24651, #27781 ) ;
#50523 = FACE_OUTER_BOUND ( 'NONE', #46930, .T. ) ;
#50524 = PLANE ( 'NONE',  #33894 ) ;
#50525 = PLANE ( 'NONE',  #47681 ) ;
#50526 = CARTESIAN_POINT ( 'NONE',  ( -12.60458797795435615, 0.000000000000000000, 11.86609696750642229 ) ) ;
#50527 = ORIENTED_EDGE ( 'NONE', *, *, #7570, .F. ) ;
#50528 = LINE ( 'NONE', #41156, #6774 ) ;
#50529 = PLANE ( 'NONE',  #45040 ) ;
#50530 = ORIENTED_EDGE ( 'NONE', *, *, #5579, .F. ) ;
#50531 = DIRECTION ( 'NONE',  ( 0.007781995580012663651, -3.146120232559066537E-19, -0.9999697198139514409 ) ) ;
#50532 = PLANE ( 'NONE',  #5623 ) ;
#50533 = ADVANCED_FACE ( 'NONE', ( #47889 ), #43891, .F. ) ;
#50534 = EDGE_CURVE ( 'NONE', #25308, #41647, #740, .T. ) ;
#50535 = ORIENTED_EDGE ( 'NONE', *, *, #27181, .F. ) ;
#50536 = VERTEX_POINT ( 'NONE', #31109 ) ;
#50537 = DIRECTION ( 'NONE',  ( 0.007781995580012662783, 0.000000000000000000, -0.9999697198139514409 ) ) ;
#50538 = ADVANCED_FACE ( 'NONE', ( #48433 ), #7230, .F. ) ;
#50539 = VECTOR ( 'NONE', #48721, 999.9999999999998863 ) ;
#50540 = EDGE_LOOP ( 'NONE', ( #28644, #30002 ) ) ;
#50541 = ORIENTED_EDGE ( 'NONE', *, *, #42354, .T. ) ;
#50542 = ORIENTED_EDGE ( 'NONE', *, *, #15678, .F. ) ;
#50543 = FACE_OUTER_BOUND ( 'NONE', #31065, .T. ) ;
#50544 = DIRECTION ( 'NONE',  ( -0.9335804264972041855, 0.3583679495452941621, 0.000000000000000000 ) ) ;
#50545 = DIRECTION ( 'NONE',  ( 0.7660212471507180654, -0.6427876096865404731, 0.005961354470445141482 ) ) ;
#50546 = VECTOR ( 'NONE', #55237, 999.9999999999998863 ) ;
#50547 = EDGE_LOOP ( 'NONE', ( #28045, #27836, #9498, #48432 ) ) ;
#50548 = EDGE_LOOP ( 'NONE', ( #52305, #34830, #18104, #23781 ) ) ;
#50549 = ADVANCED_FACE ( 'NONE', ( #6399 ), #11200, .F. ) ;
#50550 = DIRECTION ( 'NONE',  ( 0.005961354470445682716, -0.6427876096865404731, -0.7660212471507180654 ) ) ;
#50551 = DIRECTION ( 'NONE',  ( 0.9999697198139515519, 0.000000000000000000, 0.007781995580013368816 ) ) ;
#50552 = VERTEX_POINT ( 'NONE', #24280 ) ;
#50553 = CARTESIAN_POINT ( 'NONE',  ( -10.66170866159616715, 0.000000000000000000, 1.044114545398534766 ) ) ;
#50554 = VERTEX_POINT ( 'NONE', #23698 ) ;
#50555 = DIRECTION ( 'NONE',  ( 0.000000000000000000, -1.000000000000000000, 0.000000000000000000 ) ) ;
#50556 = CARTESIAN_POINT ( 'NONE',  ( -10.43730245779182475, 0.000000000000000000, 6.216509903659242831 ) ) ;
#50557 = ORIENTED_EDGE ( 'NONE', *, *, #21277, .F. ) ;
#50558 = ADVANCED_FACE ( 'NONE', ( #33072 ), #54102, .F. ) ;
#50559 = LINE ( 'NONE', #7123, #14114 ) ;
#50560 = ADVANCED_FACE ( 'NONE', ( #10927 ), #1831, .F. ) ;
#50561 = LINE ( 'NONE', #28127, #29104 ) ;
#50563 = EDGE_CURVE ( 'NONE', #54555, #30542, #56073, .T. ) ;
#50562 = ORIENTED_EDGE ( 'NONE', *, *, #24261, .F. ) ;
#50564 = LINE ( 'NONE', #6290, #16764 ) ;
#50565 = LINE ( 'NONE', #2826, #46595 ) ;
#50566 = DIRECTION ( 'NONE',  ( -0.005961354470445682716, -0.6427876096865404731, 0.7660212471507180654 ) ) ;
#50567 = ADVANCED_FACE ( 'NONE', ( #45297 ), #37313, .F. ) ;
#50568 = ORIENTED_EDGE ( 'NONE', *, *, #52466, .F. ) ;
#50569 = FACE_OUTER_BOUND ( 'NONE', #1620, .T. ) ;
#50570 = FACE_OUTER_BOUND ( 'NONE', #23174, .T. ) ;
#50571 = EDGE_CURVE ( 'NONE', #18631, #37343, #11504, .T. ) ;
#50572 = DIRECTION ( 'NONE',  ( 0.9999697198139515519, 0.000000000000000000, 0.007781995580013368816 ) ) ;
#50573 = DIRECTION ( 'NONE',  ( -0.7660212471507179544, -0.6427876096865405842, -0.005961354470445141482 ) ) ;
#50574 = LINE ( 'NONE', #37496, #8644 ) ;
#50575 = CARTESIAN_POINT ( 'NONE',  ( -12.18800911221693006, -0.1191753592594174960, 5.194892318353301341 ) ) ;
#50576 = VECTOR ( 'NONE', #12018, 1000.000000000000000 ) ;
#50577 = DIRECTION ( 'NONE',  ( -0.005961354470445682716, -0.6427876096865404731, 0.7660212471507180654 ) ) ;
#50578 = ORIENTED_EDGE ( 'NONE', *, *, #2007, .F. ) ;
#50579 = CARTESIAN_POINT ( 'NONE',  ( -19.84110863911566014, -3.108426967578157729, 9.490350352780952292 ) ) ;
#50580 = CARTESIAN_POINT ( 'NONE',  ( -14.44988390315699434, 4.819660872929013351, 2.140984944058630823 ) ) ;
#50581 = CARTESIAN_POINT ( 'NONE',  ( -15.40103151951671734, 0.000000000000000000, 12.95233060667165681 ) ) ;
#50582 = ORIENTED_EDGE ( 'NONE', *, *, #9910, .F. ) ;
#50583 = CARTESIAN_POINT ( 'NONE',  ( -11.15508609349007507, 0.000000000000000000, 4.733595666208168851 ) ) ;
#50584 = PLANE ( 'NONE',  #18172 ) ;
#50585 = AXIS2_PLACEMENT_3D ( 'NONE', #34708, #31296, #53171 ) ;
#50586 = LINE ( 'NONE', #34386, #4094 ) ;
#50587 = DIRECTION ( 'NONE',  ( -0.005002170337468016433, -0.7660444431189770143, 0.6427681459581293666 ) ) ;
#50588 = CARTESIAN_POINT ( 'NONE',  ( -18.63389729487044377, -0.006848592768176286170, 9.670969966159701059 ) ) ;
#50589 = ORIENTED_EDGE ( 'NONE', *, *, #35668, .T. ) ;
#50590 = ORIENTED_EDGE ( 'NONE', *, *, #24813, .F. ) ;
#50591 = DIRECTION ( 'NONE',  ( 0.000000000000000000, -1.000000000000000000, 0.000000000000000000 ) ) ;
#50592 = DIRECTION ( 'NONE',  ( 0.000000000000000000, -1.000000000000000000, 0.000000000000000000 ) ) ;
#50593 = ADVANCED_FACE ( 'NONE', ( #49271 ), #45553, .F. ) ;
#50594 = ORIENTED_EDGE ( 'NONE', *, *, #39394, .F. ) ;
#50595 = CARTESIAN_POINT ( 'NONE',  ( 2.072287782118878319, 0.000000000000000000, -2.950529333540147015 ) ) ;
#50596 = VERTEX_POINT ( 'NONE', #28825 ) ;
#50597 = LINE ( 'NONE', #29010, #28391 ) ;
#50598 = EDGE_CURVE ( 'NONE', #8140, #38515, #14919, .T. ) ;
#50599 = EDGE_CURVE ( 'NONE', #25448, #54376, #18913, .T. ) ;
#50600 = ORIENTED_EDGE ( 'NONE', *, *, #9337, .T. ) ;
#50601 = ORIENTED_EDGE ( 'NONE', *, *, #4263, .F. ) ;
#50602 = EDGE_LOOP ( 'NONE', ( #49720, #43823, #31328, #53884 ) ) ;
#50603 = DIRECTION ( 'NONE',  ( 0.9321478471874540261, 0.000000000000000000, -0.3620778797217457101 ) ) ;
#50604 = CARTESIAN_POINT ( 'NONE',  ( -12.54767912962405774, 0.000000000000000000, 4.553432171609165913 ) ) ;
#50605 = DIRECTION ( 'NONE',  ( -0.005961354470445682716, -0.6427876096865404731, 0.7660212471507180654 ) ) ;
#50606 = VERTEX_POINT ( 'NONE', #15456 ) ;
#50607 = FACE_OUTER_BOUND ( 'NONE', #24686, .T. ) ;
#50608 = ORIENTED_EDGE ( 'NONE', *, *, #10807, .F. ) ;
#50609 = ADVANCED_FACE ( 'NONE', ( #32525 ), #6973, .T. ) ;
#50610 = ORIENTED_EDGE ( 'NONE', *, *, #32424, .F. ) ;
#50611 = ORIENTED_EDGE ( 'NONE', *, *, #50933, .F. ) ;
#50612 = PLANE ( 'NONE',  #23203 ) ;
#50613 = DIRECTION ( 'NONE',  ( -0.6427681459581293666, -0.7660444431189770143, -0.005002170337467561935 ) ) ;
#50614 = ORIENTED_EDGE ( 'NONE', *, *, #36355, .T. ) ;
#50615 = CARTESIAN_POINT ( 'NONE',  ( 2.072287782118878319, -1.000000000000000000, -2.950529333540147015 ) ) ;
#50616 = VERTEX_POINT ( 'NONE', #32778 ) ;
#50617 = CARTESIAN_POINT ( 'NONE',  ( -15.80013740751165230, 0.000000000000000000, 4.528120789233099686 ) ) ;
#50618 = LINE ( 'NONE', #37851, #40415 ) ;
#50619 = VECTOR ( 'NONE', #56222, 999.9999999999998863 ) ;
#50620 = VERTEX_POINT ( 'NONE', #36227 ) ;
#50621 = CARTESIAN_POINT ( 'NONE',  ( -27.99767448711536133, 0.000000000000000000, 7.557179307314289218 ) ) ;
#50622 = ORIENTED_EDGE ( 'NONE', *, *, #23882, .F. ) ;
#50623 = ADVANCED_FACE ( 'NONE', ( #27711 ), #10682, .F. ) ;
#50624 = LINE ( 'NONE', #28473, #24643 ) ;
#50625 = DIRECTION ( 'NONE',  ( 0.007781995580012663651, -3.146120232559066537E-19, -0.9999697198139514409 ) ) ;
#50626 = ADVANCED_FACE ( 'NONE', ( #6145 ), #14632, .F. ) ;
#50627 = CARTESIAN_POINT ( 'NONE',  ( -14.94760462649100496, 0.000000000000000000, 2.488088991209854051 ) ) ;
#50628 = LINE ( 'NONE', #45505, #3015 ) ;
#50629 = LINE ( 'NONE', #46937, #38682 ) ;
#50630 = CARTESIAN_POINT ( 'NONE',  ( -61.70068505767309830, 8.059153983834628221, -3.000000000000000000 ) ) ;
#50631 = ORIENTED_EDGE ( 'NONE', *, *, #23618, .F. ) ;
#50632 = ORIENTED_EDGE ( 'NONE', *, *, #29748, .F. ) ;
#50633 = FACE_BOUND ( 'NONE', #46964, .T. ) ;
#50634 = EDGE_CURVE ( 'NONE', #21969, #25655, #40765, .T. ) ;
#50635 = CARTESIAN_POINT ( 'NONE',  ( -68.54116703456952564, -9.287124719764433323, 7.481505251583916660 ) ) ;
#50636 = CARTESIAN_POINT ( 'NONE',  ( -9.808144436391993182, 0.000000000000000000, 10.77986332834118777 ) ) ;
#50637 = DIRECTION ( 'NONE',  ( 0.007781995580012662783, 0.000000000000000000, -0.9999697198139514409 ) ) ;
#50638 = DIRECTION ( 'NONE',  ( 0.5364919789714477361, 0.6444004775717706579, 0.5449076811759711036 ) ) ;
#50639 = CARTESIAN_POINT ( 'NONE',  ( -19.94320461137762024, -2.137015261443157232, 7.935755791898535527 ) ) ;
#50640 = EDGE_LOOP ( 'NONE', ( #25316, #11989, #41406, #4521 ) ) ;
#50641 = CARTESIAN_POINT ( 'NONE',  ( -15.79283290138508455, 0.000000000000000000, 3.589507438754780289 ) ) ;
#50642 = CARTESIAN_POINT ( 'NONE',  ( -14.66887761629205222, 0.000000000000000000, 12.58869632783390990 ) ) ;
#50643 = VERTEX_POINT ( 'NONE', #3793 ) ;
#50644 = CARTESIAN_POINT ( 'NONE',  ( -17.46532115785441519, 0.000000000000000000, 13.67492996699914265 ) ) ;
#50645 = LINE ( 'NONE', #49805, #2323 ) ;
#50646 = ORIENTED_EDGE ( 'NONE', *, *, #16421, .T. ) ;
#50647 = EDGE_CURVE ( 'NONE', #28808, #12905, #25664, .T. ) ;
#50648 = DIRECTION ( 'NONE',  ( -0.005961354470445682716, -0.6427876096865404731, 0.7660212471507180654 ) ) ;
#50649 = DIRECTION ( 'NONE',  ( -0.6427681459581293666, -0.7660444431189770143, -0.005002170337467561935 ) ) ;
#50650 = DIRECTION ( 'NONE',  ( 0.3583679495452925523, 0.9335804264972047406, 0.000000000000000000 ) ) ;
#50651 = EDGE_CURVE ( 'NONE', #53756, #33683, #8341, .T. ) ;
#50652 = CARTESIAN_POINT ( 'NONE',  ( -18.67775241435682432, 0.000000000000000000, 4.136394454059623804 ) ) ;
#50653 = DIRECTION ( 'NONE',  ( 0.9999697198139515519, 0.000000000000000000, 0.007781995580013368816 ) ) ;
#50654 = ORIENTED_EDGE ( 'NONE', *, *, #13361, .F. ) ;
#50655 = ORIENTED_EDGE ( 'NONE', *, *, #18760, .F. ) ;
#50656 = DIRECTION ( 'NONE',  ( -0.7660212471507179544, -0.6427876096865405842, -0.005961354470445141482 ) ) ;
#50657 = CARTESIAN_POINT ( 'NONE',  ( -14.66887761629205222, 0.000000000000000000, 12.58869632783390990 ) ) ;
#50658 = CARTESIAN_POINT ( 'NONE',  ( -50.02554558092695913, 3.776013638374817294, 5.000000000000000000 ) ) ;
#50659 = EDGE_CURVE ( 'NONE', #48678, #47622, #25973, .T. ) ;
#50660 = FACE_OUTER_BOUND ( 'NONE', #53472, .T. ) ;
#50661 = VECTOR ( 'NONE', #45203, 1000.000000000000114 ) ;
#50662 = DIRECTION ( 'NONE',  ( -0.005002170337468016433, -0.7660444431189770143, 0.6427681459581293666 ) ) ;
#50663 = EDGE_CURVE ( 'NONE', #14307, #29351, #3252, .T. ) ;
#50664 = CARTESIAN_POINT ( 'NONE',  ( -17.19404809803491574, 0.000000000000000000, 4.517273053929070414 ) ) ;
#50665 = VERTEX_POINT ( 'NONE', #16884 ) ;
#50666 = CARTESIAN_POINT ( 'NONE',  ( -20.89679648621866193, -4.889348428825661230, 12.82321088736104642 ) ) ;
#50667 = EDGE_CURVE ( 'NONE', #14388, #31826, #38749, .T. ) ;
#50668 = CARTESIAN_POINT ( 'NONE',  ( -8.910664554068135956, -10.68360705318012194, 6.679578295905873375 ) ) ;
#50669 = PLANE ( 'NONE',  #22420 ) ;
#50670 = ORIENTED_EDGE ( 'NONE', *, *, #36917, .T. ) ;
#50671 = CARTESIAN_POINT ( 'NONE',  ( -27.06552663992790997, 0.000000000000000000, 7.195101427592543786 ) ) ;
#50672 = DIRECTION ( 'NONE',  ( 0.6427681459581294776, -0.7660444431189769032, 0.005002170337467562802 ) ) ;
#50673 = DIRECTION ( 'NONE',  ( 0.9321478471874540261, 0.000000000000000000, -0.3620778797217457101 ) ) ;
#50674 = ADVANCED_FACE ( 'NONE', ( #38159 ), #3529, .T. ) ;
#50675 = ORIENTED_EDGE ( 'NONE', *, *, #30073, .T. ) ;
#50676 = ADVANCED_FACE ( 'NONE', ( #37900 ), #29368, .F. ) ;
#50677 = DIRECTION ( 'NONE',  ( 0.005961354470445682716, -0.6427876096865404731, -0.7660212471507180654 ) ) ;
#50678 = ORIENTED_EDGE ( 'NONE', *, *, #51305, .T. ) ;
#50679 = EDGE_CURVE ( 'NONE', #46842, #19985, #46978, .T. ) ;
#50680 = ORIENTED_EDGE ( 'NONE', *, *, #24056, .T. ) ;
#50681 = VERTEX_POINT ( 'NONE', #47233 ) ;
#50682 = ORIENTED_EDGE ( 'NONE', *, *, #12182, .T. ) ;
#50683 = DIRECTION ( 'NONE',  ( -0.9999697198139514409, -0.000000000000000000, -0.007781995580013368816 ) ) ;
#50684 = ORIENTED_EDGE ( 'NONE', *, *, #13298, .T. ) ;
#50685 = EDGE_LOOP ( 'NONE', ( #18838, #55784, #45942, #33998 ) ) ;
#50686 = DIRECTION ( 'NONE',  ( 0.9999697198139515519, 0.000000000000000000, 0.007781995580013368816 ) ) ;
#50687 = VERTEX_POINT ( 'NONE', #4097 ) ;
#50688 = EDGE_LOOP ( 'NONE', ( #48136, #50009, #22693, #13528 ) ) ;
#50689 = DIRECTION ( 'NONE',  ( 0.007781995580012663651, -3.146120232559066537E-19, -0.9999697198139514409 ) ) ;
#50690 = DIRECTION ( 'NONE',  ( 0.6427681459581294776, -0.7660444431189769032, 0.005002170337467562802 ) ) ;
#50691 = DIRECTION ( 'NONE',  ( -0.7660212471507179544, -0.6427876096865405842, -0.005961354470445141482 ) ) ;
#50692 = DIRECTION ( 'NONE',  ( 0.000000000000000000, -0.000000000000000000, -1.000000000000000000 ) ) ;
#50693 = FACE_OUTER_BOUND ( 'NONE', #47707, .T. ) ;
#50694 = ORIENTED_EDGE ( 'NONE', *, *, #24580, .F. ) ;
#50695 = ORIENTED_EDGE ( 'NONE', *, *, #37962, .F. ) ;
#50696 = LINE ( 'NONE', #37344, #52088 ) ;
#50697 = EDGE_CURVE ( 'NONE', #19093, #27972, #21426, .T. ) ;
#50698 = DIRECTION ( 'NONE',  ( -0.6246952433987894571, 0.7422098413412802076, 0.2426528472758539834 ) ) ;
#50699 = PRODUCT_DEFINITION_CONTEXT ( 'detailed design', #46339, 'design' ) ;
#50700 = CARTESIAN_POINT ( 'NONE',  ( -28.92982233430281980, 0.000000000000000000, 7.919257187036034651 ) ) ;
#50701 = LINE ( 'NONE', #11791, #38629 ) ;
#50702 = DIRECTION ( 'NONE',  ( 0.9321478471874540261, 0.000000000000000000, -0.3620778797217456546 ) ) ;
#50703 = CARTESIAN_POINT ( 'NONE',  ( -10.23730851382903495, 0.000000000000000000, 6.218066302775246079 ) ) ;
#50704 = ORIENTED_EDGE ( 'NONE', *, *, #25179, .F. ) ;
#50705 = DIRECTION ( 'NONE',  ( 0.6427681459581294776, -0.7660444431189769032, 0.005002170337467562802 ) ) ;
#50706 = VERTEX_POINT ( 'NONE', #12033 ) ;
#50707 = ADVANCED_FACE ( 'NONE', ( #34465 ), #2945, .F. ) ;
#50708 = DIRECTION ( 'NONE',  ( 0.5364919789714477361, 0.6444004775717706579, 0.5449076811759711036 ) ) ;
#50709 = CARTESIAN_POINT ( 'NONE',  ( -18.39746900504187010, 0.000000000000000000, 14.03700784672088808 ) ) ;
#50710 = CARTESIAN_POINT ( 'NONE',  ( -21.47419595591918906, 0.000000000000000000, 5.222628093224860102 ) ) ;
#50711 = DIRECTION ( 'NONE',  ( 0.000000000000000000, -0.000000000000000000, -1.000000000000000000 ) ) ;
#50712 = CARTESIAN_POINT ( 'NONE',  ( -23.33849165029409889, 0.000000000000000000, 5.946783852668351855 ) ) ;
#50713 = EDGE_CURVE ( 'NONE', #50620, #6417, #20840, .T. ) ;
#50714 = ADVANCED_FACE ( 'NONE', ( #34215 ), #16042, .F. ) ;
#50715 = CARTESIAN_POINT ( 'NONE',  ( -10.94028622754223967, 0.000000000000000000, 11.14038480894692995 ) ) ;
#50716 = ORIENTED_EDGE ( 'NONE', *, *, #13468, .F. ) ;
#50717 = VERTEX_POINT ( 'NONE', #42147 ) ;
#50718 = CARTESIAN_POINT ( 'NONE',  ( -15.83306965045904668, 0.000000000000000000, 8.759843284363483917 ) ) ;
#50719 = DIRECTION ( 'NONE',  ( -0.6427681459581293666, -0.7660444431189770143, -0.005002170337467561935 ) ) ;
#50720 = CARTESIAN_POINT ( 'NONE',  ( -13.49264084522192064, 0.000000000000000000, 6.562064623656943319 ) ) ;
#50721 = CARTESIAN_POINT ( 'NONE',  ( -21.47263955680318404, 0.000000000000000000, 5.022634149262071190 ) ) ;
#50722 = EDGE_CURVE ( 'NONE', #51840, #14307, #11763, .T. ) ;
#50723 = PLANE ( 'NONE',  #25790 ) ;
#50724 = CARTESIAN_POINT ( 'NONE',  ( -12.16389985764536519, 25.63544498867374344, -3.297528153982450583 ) ) ;
#50725 = CARTESIAN_POINT ( 'NONE',  ( -12.07243185130034213, -2.784623065533160524, 1.481819574845134602 ) ) ;
#50726 = EDGE_CURVE ( 'NONE', #33095, #23836, #55473, .T. ) ;
#50727 = PLANE ( 'NONE',  #21484 ) ;
#50728 = LINE ( 'NONE', #38220, #31949 ) ;
#50729 = ORIENTED_EDGE ( 'NONE', *, *, #47749, .F. ) ;
#50730 = ADVANCED_FACE ( 'NONE', ( #46686 ), #7811, .F. ) ;
#50731 = VERTEX_POINT ( 'NONE', #12617 ) ;
#50732 = EDGE_CURVE ( 'NONE', #36692, #37781, #676, .T. ) ;
#50733 = ORIENTED_EDGE ( 'NONE', *, *, #14983, .T. ) ;
#50734 = ORIENTED_EDGE ( 'NONE', *, *, #17133, .F. ) ;
#50735 = ORIENTED_EDGE ( 'NONE', *, *, #18893, .F. ) ;
#50736 = ORIENTED_EDGE ( 'NONE', *, *, #10796, .F. ) ;
#50737 = DIRECTION ( 'NONE',  ( 0.5364919789714477361, 0.6444004775717706579, 0.5449076811759711036 ) ) ;
#50738 = DIRECTION ( 'NONE',  ( 0.9999697198139515519, 0.000000000000000000, 0.007781995580013368816 ) ) ;
#50739 = DIRECTION ( 'NONE',  ( -0.9999697198139514409, -0.000000000000000000, -0.007781995580013368816 ) ) ;
#50740 = ORIENTED_EDGE ( 'NONE', *, *, #55448, .F. ) ;
#50741 = CARTESIAN_POINT ( 'NONE',  ( -21.47263955680318404, 0.000000000000000000, 5.022634149262071190 ) ) ;
#50742 = EDGE_LOOP ( 'NONE', ( #46299, #48809, #17140, #9932 ) ) ;
#50743 = LINE ( 'NONE', #46779, #18649 ) ;
#50744 = ORIENTED_EDGE ( 'NONE', *, *, #46527, .T. ) ;
#50745 = CARTESIAN_POINT ( 'NONE',  ( -67.74416038478570101, -8.858064234063045106, 5.268187007955521750 ) ) ;
#50746 = DIRECTION ( 'NONE',  ( 0.9999697198139515519, 0.000000000000000000, 0.007781995580013368816 ) ) ;
#50747 = LINE ( 'NONE', #33172, #37747 ) ;
#50748 = ORIENTED_EDGE ( 'NONE', *, *, #52495, .F. ) ;
#50749 = LINE ( 'NONE', #38244, #30129 ) ;
#50750 = EDGE_LOOP ( 'NONE', ( #855, #29803, #21967, #15895 ) ) ;
#50751 = CARTESIAN_POINT ( 'NONE',  ( -13.10951999731236128, 0.4483081953215036219, 2.709254009572826138 ) ) ;
#50752 = ADVANCED_FACE ( 'NONE', ( #35889 ), #48356, .F. ) ;
#50753 = DIRECTION ( 'NONE',  ( 0.007781995580012663651, -3.146120232559066537E-19, -0.9999697198139514409 ) ) ;
#50754 = DIRECTION ( 'NONE',  ( -0.5364919789714478471, 0.6444004775717705469, -0.5449076811759709926 ) ) ;
#50755 = EDGE_CURVE ( 'NONE', #55136, #4507, #52362, .T. ) ;
#50756 = CARTESIAN_POINT ( 'NONE',  ( -27.99923088623136636, 0.000000000000000000, 7.757173251277078130 ) ) ;
#50757 = DIRECTION ( 'NONE',  ( 0.9999697198139515519, 0.000000000000000000, 0.007781995580013368816 ) ) ;
#50758 = LINE ( 'NONE', #12142, #40286 ) ;
#50759 = EDGE_CURVE ( 'NONE', #49826, #22994, #4930, .T. ) ;
#50760 = CARTESIAN_POINT ( 'NONE',  ( -16.42972749701432278, 4.333955019861509328, 10.37594377198947804 ) ) ;
#50761 = CARTESIAN_POINT ( 'NONE',  ( -22.20772426397657995, -4.241740624735659715, 12.26958501973509463 ) ) ;
#50762 = VERTEX_POINT ( 'NONE', #9767 ) ;
#50763 = CARTESIAN_POINT ( 'NONE',  ( -6.110905869600904872, 1.712176620043476140E-14, 2.600000000000000089 ) ) ;
#50764 = ORIENTED_EDGE ( 'NONE', *, *, #35250, .T. ) ;
#50765 = ADVANCED_FACE ( 'NONE', ( #30780 ), #27075, .F. ) ;
#50766 = EDGE_CURVE ( 'NONE', #13246, #43824, #5482, .T. ) ;
#50767 = ADVANCED_FACE ( 'NONE', ( #39012 ), #43816, .F. ) ;
#50768 = CARTESIAN_POINT ( 'NONE',  ( -20.95581447963227717, 20.46320434849166148, -4.352198852488014857 ) ) ;
#50769 = PLANE ( 'NONE',  #29644 ) ;
#50770 = DIRECTION ( 'NONE',  ( 0.007781995580012663651, 0.000000000000000000, -0.9999697198139515519 ) ) ;
#50771 = CARTESIAN_POINT ( 'NONE',  ( -14.76859376284157044, -1.003701604285655025, 2.585921142092966640 ) ) ;
#50772 = PLANE ( 'NONE',  #13180 ) ;
#50773 = FACE_OUTER_BOUND ( 'NONE', #29445, .T. ) ;
#50774 = ORIENTED_EDGE ( 'NONE', *, *, #5607, .T. ) ;
#50775 = CARTESIAN_POINT ( 'NONE',  ( -18.45768884757317352, -1.489407457353155717, 6.295896285107346557 ) ) ;
#50776 = CARTESIAN_POINT ( 'NONE',  ( -9.342070512798265725, 0.000000000000000000, 10.59882438848031505 ) ) ;
#50777 = CARTESIAN_POINT ( 'NONE',  ( -20.01713377844408726, -3.917936722690662066, 4.531652967349151240 ) ) ;
#50778 = FACE_OUTER_BOUND ( 'NONE', #40748, .T. ) ;
#50779 = FACE_OUTER_BOUND ( 'NONE', #22263, .T. ) ;
#50780 = EDGE_CURVE ( 'NONE', #28121, #19288, #79, .T. ) ;
#50781 = PLANE ( 'NONE',  #43009 ) ;
#50782 = DIRECTION ( 'NONE',  ( 0.005961354470445682716, -0.6427876096865404731, -0.7660212471507180654 ) ) ;
#50783 = CARTESIAN_POINT ( 'NONE',  ( -14.97008238625287646, -0.1191753592594189115, 4.434577441229718531 ) ) ;
#50784 = ORIENTED_EDGE ( 'NONE', *, *, #46003, .F. ) ;
#50785 = ADVANCED_FACE ( 'NONE', ( #26230 ), #26496, .F. ) ;
#50786 = LINE ( 'NONE', #32911, #37573 ) ;
#50787 = FACE_OUTER_BOUND ( 'NONE', #23766, .T. ) ;
#50788 = EDGE_LOOP ( 'NONE', ( #24065, #7963, #30063 ) ) ;
#50789 = EDGE_CURVE ( 'NONE', #6267, #2187, #34744, .T. ) ;
#50790 = ORIENTED_EDGE ( 'NONE', *, *, #18991, .F. ) ;
#50791 = CARTESIAN_POINT ( 'NONE',  ( -23.33693525117809386, 0.000000000000000000, 5.746789908705562944 ) ) ;
#50792 = EDGE_CURVE ( 'NONE', #16631, #36118, #13462, .T. ) ;
#50793 = ORIENTED_EDGE ( 'NONE', *, *, #10297, .F. ) ;
#50794 = ORIENTED_EDGE ( 'NONE', *, *, #54169, .F. ) ;
#50795 = CARTESIAN_POINT ( 'NONE',  ( -20.99889245848062558, -3.917936722690661178, 11.26861632647862876 ) ) ;
#50796 = AXIS2_PLACEMENT_3D ( 'NONE', #41070, #14139, #31466 ) ;
#50797 = ORIENTED_EDGE ( 'NONE', *, *, #24550, .F. ) ;
#50798 = ORIENTED_EDGE ( 'NONE', *, *, #25835, .T. ) ;
#50799 = ORIENTED_EDGE ( 'NONE', *, *, #17379, .T. ) ;
#50800 = LINE ( 'NONE', #49952, #55609 ) ;
#50801 = CARTESIAN_POINT ( 'NONE',  ( -65.07102203629978021, -9.156566482107063365, 0.3363546178749044491 ) ) ;
#50802 = LINE ( 'NONE', #3663, #386 ) ;
#50803 = ORIENTED_EDGE ( 'NONE', *, *, #40211, .F. ) ;
#50804 = VERTEX_POINT ( 'NONE', #30514 ) ;
#50805 = DIRECTION ( 'NONE',  ( 0.007781995580012662783, 0.000000000000000000, -0.9999697198139514409 ) ) ;
#50806 = DIRECTION ( 'NONE',  ( -0.005002170337468016433, -0.7660444431189770143, 0.6427681459581293666 ) ) ;
#50807 = ORIENTED_EDGE ( 'NONE', *, *, #35694, .F. ) ;
#50808 = DIRECTION ( 'NONE',  ( -0.6427681459581293666, -0.7660444431189770143, -0.005002170337467561935 ) ) ;
#50809 = ORIENTED_EDGE ( 'NONE', *, *, #20186, .T. ) ;
#50810 = DIRECTION ( 'NONE',  ( 0.005002170337468016433, -0.7660444431189770143, -0.6427681459581293666 ) ) ;
#50811 = LINE ( 'NONE', #47397, #35779 ) ;
#50812 = EDGE_LOOP ( 'NONE', ( #9135, #41821, #47443, #5017 ) ) ;
#50813 = DIRECTION ( 'NONE',  ( -0.005002170337468016433, -0.7660444431189770143, 0.6427681459581293666 ) ) ;
#50814 = EDGE_CURVE ( 'NONE', #42842, #10997, #44115, .T. ) ;
#50815 = DIRECTION ( 'NONE',  ( 0.000000000000000000, 0.000000000000000000, 1.000000000000000000 ) ) ;
#50816 = ORIENTED_EDGE ( 'NONE', *, *, #52869, .F. ) ;
#50817 = DIRECTION ( 'NONE',  ( 0.6427681459581294776, -0.7660444431189769032, 0.005002170337467562802 ) ) ;
#50818 = FACE_OUTER_BOUND ( 'NONE', #16487, .T. ) ;
#50819 = DIRECTION ( 'NONE',  ( -0.6427681459581293666, -0.7660444431189770143, -0.005002170337467561935 ) ) ;
#50820 = ORIENTED_EDGE ( 'NONE', *, *, #17947, .T. ) ;
#50821 = EDGE_CURVE ( 'NONE', #16969, #21242, #43541, .T. ) ;
#50822 = ADVANCED_FACE ( 'NONE', ( #1208 ), #21956, .F. ) ;
#50823 = EDGE_CURVE ( 'NONE', #54087, #9690, #21700, .T. ) ;
#50824 = AXIS2_PLACEMENT_3D ( 'NONE', #34295, #25473, #12128 ) ;
#50825 = CARTESIAN_POINT ( 'NONE',  ( -19.73447084723482448, 0.000000000000000000, 6.713495315519605100 ) ) ;
#50826 = FACE_OUTER_BOUND ( 'NONE', #41037, .T. ) ;
#50827 = CARTESIAN_POINT ( 'NONE',  ( -12.20237937974333953, -0.1191753592594185784, 7.041440834642125779 ) ) ;
#50828 = CARTESIAN_POINT ( 'NONE',  ( -16.72785480207782527, 0.000000000000000000, 4.320895021734290964 ) ) ;
#50829 = ADVANCED_FACE ( 'NONE', ( #31032 ), #17995, .F. ) ;
#50830 = CARTESIAN_POINT ( 'NONE',  ( -16.81345671998191449, 0.000000000000000000, 3.412238694616132495 ) ) ;
#50831 = LINE ( 'NONE', #8241, #7994 ) ;
#50832 = AXIS2_PLACEMENT_3D ( 'NONE', #5460, #44623, #48634 ) ;
#50833 = CARTESIAN_POINT ( 'NONE',  ( -67.62965612898899792, -11.46308303289930386, -8.694190345973900946 ) ) ;
#50834 = VERTEX_POINT ( 'NONE', #18251 ) ;
#50835 = LINE ( 'NONE', #2837, #30772 ) ;
#50836 = DIRECTION ( 'NONE',  ( 0.000000000000000000, -1.000000000000000000, 0.000000000000000000 ) ) ;
#50837 = FACE_OUTER_BOUND ( 'NONE', #55220, .T. ) ;
#50838 = ORIENTED_EDGE ( 'NONE', *, *, #30971, .F. ) ;
#50839 = CARTESIAN_POINT ( 'NONE',  ( -18.21825225188358743, -0.1191753592594171213, 3.858214293418511076 ) ) ;
#50840 = CARTESIAN_POINT ( 'NONE',  ( -20.29238058347068829, -4.727446477803161073, 12.32272654073281259 ) ) ;
#50841 = DIRECTION ( 'NONE',  ( 0.007781995580012663651, 0.000000000000000000, -0.9999697198139515519 ) ) ;
#50842 = CARTESIAN_POINT ( 'NONE',  ( -11.47218654453707032, 0.000000000000000000, 1.237813275329368690 ) ) ;
#50843 = ADVANCED_FACE ( 'NONE', ( #52899 ), #41527, .F. ) ;
#50844 = LINE ( 'NONE', #33283, #34722 ) ;
#50845 = ORIENTED_EDGE ( 'NONE', *, *, #32348, .F. ) ;
#50846 = EDGE_LOOP ( 'NONE', ( #34818, #8963, #54722, #2186 ) ) ;
#50847 = ADVANCED_FACE ( 'NONE', ( #15391 ), #14846, .F. ) ;
#50848 = FACE_OUTER_BOUND ( 'NONE', #26578, .T. ) ;
#50849 = CARTESIAN_POINT ( 'NONE',  ( -16.92497469253532927, 0.000000000000000000, 3.950028919360522917 ) ) ;
#50850 = EDGE_CURVE ( 'NONE', #13341, #49579, #32705, .T. ) ;
#50851 = VECTOR ( 'NONE', #2475, 1000.000000000000000 ) ;
#50852 = ORIENTED_EDGE ( 'NONE', *, *, #45043, .F. ) ;
#50853 = PLANE ( 'NONE',  #32244 ) ;
#50854 = ORIENTED_EDGE ( 'NONE', *, *, #15787, .F. ) ;
#50855 = DIRECTION ( 'NONE',  ( 0.9321478471874541372, 0.000000000000000000, -0.3620778797217453771 ) ) ;
#50856 = EDGE_CURVE ( 'NONE', #32088, #32467, #6075, .T. ) ;
#50857 = EDGE_LOOP ( 'NONE', ( #39447, #40770, #11484, #51639 ) ) ;
#50858 = VERTEX_POINT ( 'NONE', #50309 ) ;
#50859 = ORIENTED_EDGE ( 'NONE', *, *, #37762, .T. ) ;
#50860 = CARTESIAN_POINT ( 'NONE',  ( -18.67619601524082285, 0.000000000000000000, 3.936400510096834893 ) ) ;
#50861 = CARTESIAN_POINT ( 'NONE',  ( -14.56888064431065821, -0.1191753592594197858, 12.58947452739191064 ) ) ;
#50862 = DIRECTION ( 'NONE',  ( 0.007781995580012663651, -3.146120232559066537E-19, -0.9999697198139514409 ) ) ;
#50864 = DIRECTION ( 'NONE',  ( -0.6427681459581293666, -0.7660444431189770143, -0.005002170337467561935 ) ) ;
#50863 = AXIS2_PLACEMENT_3D ( 'NONE', #51175, #12837, #56018 ) ;
#50865 = ORIENTED_EDGE ( 'NONE', *, *, #29936, .F. ) ;
#50866 = AXIS2_PLACEMENT_3D ( 'NONE', #19576, #19014, #9945 ) ;
#50867 = ORIENTED_EDGE ( 'NONE', *, *, #32047, .F. ) ;
#50868 = ORIENTED_EDGE ( 'NONE', *, *, #10738, .T. ) ;
#50869 = LINE ( 'NONE', #47174, #18660 ) ;
#50870 = CARTESIAN_POINT ( 'NONE',  ( -25.92429756520238016, 17.40220053346460105, -4.657437592157546824 ) ) ;
#50871 = VERTEX_POINT ( 'NONE', #15657 ) ;
#50872 = DIRECTION ( 'NONE',  ( -0.5449076811759708816, 0.6444004775717707689, 0.5364919789714475140 ) ) ;
#50873 = ORIENTED_EDGE ( 'NONE', *, *, #15449, .T. ) ;
#50874 = PLANE ( 'NONE',  #31489 ) ;
#50875 = PLANE ( 'NONE',  #36705 ) ;
#50876 = ORIENTED_EDGE ( 'NONE', *, *, #25658, .F. ) ;
#50877 = FACE_OUTER_BOUND ( 'NONE', #28832, .T. ) ;
#50878 = ORIENTED_EDGE ( 'NONE', *, *, #40090, .F. ) ;
#50879 = CARTESIAN_POINT ( 'NONE',  ( -9.841832199969237749, -0.1191753592594186895, 2.258494251131236030 ) ) ;
#50880 = CARTESIAN_POINT ( 'NONE',  ( -11.82414738691523581, 0.000000000000000000, 5.297727002544709407 ) ) ;
#50881 = ORIENTED_EDGE ( 'NONE', *, *, #8580, .T. ) ;
#50882 = DIRECTION ( 'NONE',  ( 0.005961354470445682716, -0.6427876096865404731, -0.7660212471507180654 ) ) ;
#50883 = PLANE ( 'NONE',  #16648 ) ;
#50884 = LINE ( 'NONE', #33863, #26891 ) ;
#50885 = DIRECTION ( 'NONE',  ( 0.6427681459581294776, -0.7660444431189769032, 0.005002170337467562802 ) ) ;
#50886 = VERTEX_POINT ( 'NONE', #49192 ) ;
#50887 = ADVANCED_FACE ( 'NONE', ( #6594 ), #37246, .F. ) ;
#50888 = VECTOR ( 'NONE', #53114, 1000.000000000000000 ) ;
#50889 = ORIENTED_EDGE ( 'NONE', *, *, #6082, .F. ) ;
#50890 = AXIS2_PLACEMENT_3D ( 'NONE', #40289, #26662, #27810 ) ;
#50891 = DIRECTION ( 'NONE',  ( -0.005002170337468016433, -0.7660444431189770143, 0.6427681459581293666 ) ) ;
#50892 = DIRECTION ( 'NONE',  ( 0.9999697198139515519, 0.000000000000000000, 0.007781995580013368816 ) ) ;
#50893 = CARTESIAN_POINT ( 'NONE',  ( -67.33410474092524112, 0.1329883344697675163, 0.6700356180039969134 ) ) ;
#50894 = EDGE_CURVE ( 'NONE', #37968, #37323, #28448, .T. ) ;
#50895 = EDGE_CURVE ( 'NONE', #52748, #35993, #24210, .T. ) ;
#50896 = LINE ( 'NONE', #33872, #35800 ) ;
#50897 = CARTESIAN_POINT ( 'NONE',  ( -21.77789634727513857, -5.375054281893161701, 13.96258604752399712 ) ) ;
#50898 = FACE_OUTER_BOUND ( 'NONE', #46268, .T. ) ;
#50899 = ORIENTED_EDGE ( 'NONE', *, *, #4292, .F. ) ;
#50900 = CARTESIAN_POINT ( 'NONE',  ( -15.34699672469169762, 0.000000000000000000, 6.008975514032165677 ) ) ;
#50901 = CARTESIAN_POINT ( 'NONE',  ( -16.79925329029790149, 0.000000000000000000, 13.49544742625427496 ) ) ;
#50902 = VERTEX_POINT ( 'NONE', #23914 ) ;
#50903 = CARTESIAN_POINT ( 'NONE',  ( -12.33850799832341849, 0.000000000000000000, 11.68350162852954632 ) ) ;
#50904 = ORIENTED_EDGE ( 'NONE', *, *, #40404, .F. ) ;
#50905 = CARTESIAN_POINT ( 'NONE',  ( -9.287916345609888324, 0.000000000000000000, 3.640130203506913631 ) ) ;
#50906 = LINE ( 'NONE', #29347, #4264 ) ;
#50907 = DIRECTION ( 'NONE',  ( -0.5449076811759708816, 0.6444004775717707689, 0.5364919789714475140 ) ) ;
#50908 = DIRECTION ( 'NONE',  ( -0.005961354470445682716, -0.6427876096865404731, 0.7660212471507180654 ) ) ;
#50909 = VECTOR ( 'NONE', #35267, 999.9999999999998863 ) ;
#50910 = CARTESIAN_POINT ( 'NONE',  ( -68.15691219544618207, 2.000000000026043612, -4.725549651835818210 ) ) ;
#50911 = ORIENTED_EDGE ( 'NONE', *, *, #51742, .T. ) ;
#50912 = VERTEX_POINT ( 'NONE', #31881 ) ;
#50913 = CARTESIAN_POINT ( 'NONE',  ( -68.81473095537231188, -0.6015118236491385773, -6.396357082918164849 ) ) ;
#50914 = CARTESIAN_POINT ( 'NONE',  ( 2.072287782118878319, 0.000000000000000000, -2.950529333540147015 ) ) ;
#50915 = CARTESIAN_POINT ( 'NONE',  ( -23.23471500290295921, 19.24370688441070953, 4.657440554554202805 ) ) ;
#50916 = DIRECTION ( 'NONE',  ( 0.9999697198139515519, 0.000000000000000000, 0.007781995580013368816 ) ) ;
#50917 = FACE_OUTER_BOUND ( 'NONE', #13486, .T. ) ;
#50918 = CARTESIAN_POINT ( 'NONE',  ( -18.19747506107908563, 0.000000000000000000, 14.03856424583689311 ) ) ;
#50919 = ORIENTED_EDGE ( 'NONE', *, *, #29746, .T. ) ;
#50920 = CARTESIAN_POINT ( 'NONE',  ( -12.63540168802631669, -0.1191753592594192307, 2.975418187038710194 ) ) ;
#50921 = ADVANCED_FACE ( 'NONE', ( #5771 ), #2607, .F. ) ;
#50922 = DIRECTION ( 'NONE',  ( -0.5364919789714478471, 0.6444004775717705469, -0.5449076811759709926 ) ) ;
#50923 = DIRECTION ( 'NONE',  ( -0.7660212471507179544, -0.6427876096865405842, -0.005961354470445141482 ) ) ;
#50924 = EDGE_LOOP ( 'NONE', ( #48575, #27001, #41287, #7284, #938 ) ) ;
#50925 = EDGE_CURVE ( 'NONE', #9595, #21126, #45228, .T. ) ;
#50926 = CARTESIAN_POINT ( 'NONE',  ( -68.13401945688795536, -11.18625196726625148, 7.477472888882759960 ) ) ;
#50927 = DIRECTION ( 'NONE',  ( 0.6427681459581294776, -0.7660444431189769032, 0.005002170337467562802 ) ) ;
#50928 = DIRECTION ( 'NONE',  ( 0.9999697198139515519, 0.000000000000000000, 0.007781995580013368816 ) ) ;
#50929 = VERTEX_POINT ( 'NONE', #23381 ) ;
#50930 = AXIS2_PLACEMENT_3D ( 'NONE', #20045, #45615, #37367 ) ;
#50931 = AXIS2_PLACEMENT_3D ( 'NONE', #34170, #52321, #17368 ) ;
#50932 = CARTESIAN_POINT ( 'NONE',  ( -10.74029228357944987, 0.000000000000000000, 11.14194120806293320 ) ) ;
#50933 = EDGE_CURVE ( 'NONE', #16128, #55340, #2334, .T. ) ;
#50934 = VERTEX_POINT ( 'NONE', #2033 ) ;
#50935 = ORIENTED_EDGE ( 'NONE', *, *, #22906, .F. ) ;
#50936 = ORIENTED_EDGE ( 'NONE', *, *, #52997, .F. ) ;
#50937 = VECTOR ( 'NONE', #46751, 1000.000000000000227 ) ;
#50938 = VERTEX_POINT ( 'NONE', #14565 ) ;
#50939 = LINE ( 'NONE', #20004, #16628 ) ;
#50940 = ORIENTED_EDGE ( 'NONE', *, *, #11548, .T. ) ;
#50941 = CARTESIAN_POINT ( 'NONE',  ( -15.35456184398319657, 22.06126462439962310, -3.957089338018470404 ) ) ;
#50942 = ORIENTED_EDGE ( 'NONE', *, *, #4977, .T. ) ;
#50943 = CARTESIAN_POINT ( 'NONE',  ( -12.17076479118523302, -0.1191753592594189115, 2.979034098806719211 ) ) ;
#50944 = ORIENTED_EDGE ( 'NONE', *, *, #40614, .F. ) ;
#50945 = VECTOR ( 'NONE', #55876, 999.9999999999998863 ) ;
#50946 = VERTEX_POINT ( 'NONE', #49495 ) ;
#50947 = VECTOR ( 'NONE', #55287, 999.9999999999998863 ) ;
#50948 = DIRECTION ( 'NONE',  ( -0.5364919789714478471, 0.6444004775717705469, -0.5449076811759709926 ) ) ;
#50949 = PLANE ( 'NONE',  #53872 ) ;
#50950 = PLANE ( 'NONE',  #41254 ) ;
#50951 = CARTESIAN_POINT ( 'NONE',  ( -19.60834386242827776, 0.000000000000000000, 4.298478389818581213 ) ) ;
#50952 = ADVANCED_FACE ( 'NONE', ( #54293 ), #49765, .F. ) ;
#50953 = CARTESIAN_POINT ( 'NONE',  ( -14.42280954203746646, -4.403642575758160760, 9.511368448867619563 ) ) ;
#50954 = ORIENTED_EDGE ( 'NONE', *, *, #47250, .F. ) ;
#50955 = ORIENTED_EDGE ( 'NONE', *, *, #28368, .T. ) ;
#50956 = DIRECTION ( 'NONE',  ( -0.2426528472758542054, 0.7422098413412800966, -0.6246952433987894571 ) ) ;
#50957 = LINE ( 'NONE', #10955, #7642 ) ;
#50958 = EDGE_CURVE ( 'NONE', #27743, #661, #36415, .T. ) ;
#50959 = CARTESIAN_POINT ( 'NONE',  ( -13.53673582514181106, 0.000000000000000000, 12.22817484722816772 ) ) ;
#50960 = FACE_BOUND ( 'NONE', #22431, .T. ) ;
#50961 = PLANE ( 'NONE',  #52131 ) ;
#50962 = CARTESIAN_POINT ( 'NONE',  ( -13.97153759768243297, -2.784623065533160524, 6.678992260915761037 ) ) ;
#50963 = VERTEX_POINT ( 'NONE', #6331 ) ;
#50965 = LINE ( 'NONE', #30556, #22981 ) ;
#50964 = VECTOR ( 'NONE', #2229, 999.9999999999998863 ) ;
#50966 = CARTESIAN_POINT ( 'NONE',  ( 5.558065690504402134, 8.867811663421879681E-06, -2.260478214935544017 ) ) ;
#50967 = VERTEX_POINT ( 'NONE', #23631 ) ;
#50968 = AXIS2_PLACEMENT_3D ( 'NONE', #54479, #18835, #15580 ) ;
#50969 = VECTOR ( 'NONE', #16757, 999.9999999999998863 ) ;
#50970 = LINE ( 'NONE', #29415, #1651 ) ;
#50971 = PLANE ( 'NONE',  #21449 ) ;
#50972 = PLANE ( 'NONE',  #7272 ) ;
#50973 = DIRECTION ( 'NONE',  ( -0.5449076811759708816, 0.6444004775717707689, 0.5364919789714475140 ) ) ;
#50974 = DIRECTION ( 'NONE',  ( -0.6427681459581293666, -0.7660444431189770143, -0.005002170337467561935 ) ) ;
#50975 = ADVANCED_FACE ( 'NONE', ( #36707 ), #54027, .F. ) ;
#50976 = ORIENTED_EDGE ( 'NONE', *, *, #38355, .T. ) ;
#50977 = AXIS2_PLACEMENT_3D ( 'NONE', #34894, #30890, #26349 ) ;
#50978 = AXIS2_PLACEMENT_3D ( 'NONE', #18213, #48308, #9423 ) ;
#50979 = ORIENTED_EDGE ( 'NONE', *, *, #44341, .T. ) ;
#50980 = DIRECTION ( 'NONE',  ( -0.005002170337468016433, -0.7660444431189770143, 0.6427681459581293666 ) ) ;
#50981 = CARTESIAN_POINT ( 'NONE',  ( -10.87475521869608919, 0.000000000000000000, 2.719790903276377403 ) ) ;
#50982 = DIRECTION ( 'NONE',  ( 0.5449076811759707706, 0.6444004775717708799, -0.5364919789714476250 ) ) ;
#50983 = DIRECTION ( 'NONE',  ( 0.005961354470445682716, -0.6427876096865404731, -0.7660212471507180654 ) ) ;
#50984 =( GEOMETRIC_REPRESENTATION_CONTEXT ( 3 ) GLOBAL_UNCERTAINTY_ASSIGNED_CONTEXT ( ( #37092 ) ) GLOBAL_UNIT_ASSIGNED_CONTEXT ( ( #3551, #3278, #29396 ) ) REPRESENTATION_CONTEXT ( 'NONE', 'WORKASPACE' ) );
#50985 = DIRECTION ( 'NONE',  ( -0.8531650599175527594, 0.4028455766673922356, 0.3313982828793700652 ) ) ;
#50986 = DIRECTION ( 'NONE',  ( 0.5449076811759707706, 0.6444004775717708799, -0.5364919789714476250 ) ) ;
#50987 = LINE ( 'NONE', #55836, #6598 ) ;
#50988 = LINE ( 'NONE', #51298, #31412 ) ;
#50989 = DIRECTION ( 'NONE',  ( -0.000000000000000000, 1.000000000000000000, -0.000000000000000000 ) ) ;
#50990 = DIRECTION ( 'NONE',  ( -0.005961354470445682716, -0.6427876096865404731, 0.7660212471507180654 ) ) ;
#50991 = ORIENTED_EDGE ( 'NONE', *, *, #49438, .T. ) ;
#50992 = LINE ( 'NONE', #20899, #30418 ) ;
#50993 = EDGE_LOOP ( 'NONE', ( #51074, #49254, #35793, #14991 ) ) ;
#50994 = EDGE_CURVE ( 'NONE', #52435, #40267, #32460, .T. ) ;
#50995 = AXIS2_PLACEMENT_3D ( 'NONE', #28087, #2232, #45144 ) ;
#50996 = ORIENTED_EDGE ( 'NONE', *, *, #45979, .F. ) ;
#50997 = ORIENTED_EDGE ( 'NONE', *, *, #2738, .F. ) ;
#50998 = ORIENTED_EDGE ( 'NONE', *, *, #37873, .T. ) ;
#50999 = ORIENTED_EDGE ( 'NONE', *, *, #54678, .T. ) ;
#51000 = ORIENTED_EDGE ( 'NONE', *, *, #21133, .F. ) ;
#51001 = VECTOR ( 'NONE', #16569, 1000.000000000000227 ) ;
#51002 = DIRECTION ( 'NONE',  ( 0.005961354470445682716, -0.6427876096865404731, -0.7660212471507180654 ) ) ;
#51003 = DIRECTION ( 'NONE',  ( -0.6427681459581293666, -0.7660444431189770143, -0.005002170337467561935 ) ) ;
#51004 = CARTESIAN_POINT ( 'NONE',  ( -25.20200914511100265, -0.1191753592594197858, 6.570942640130446932 ) ) ;
#51005 = ADVANCED_FACE ( 'NONE', ( #25588 ), #55997, .F. ) ;
#51006 = VECTOR ( 'NONE', #8786, 1000.000000000000000 ) ;
#51007 = VERTEX_POINT ( 'NONE', #37835 ) ;
#51008 = DIRECTION ( 'NONE',  ( 0.000000000000000000, -0.000000000000000000, -1.000000000000000000 ) ) ;
#51009 = ORIENTED_EDGE ( 'NONE', *, *, #7532, .F. ) ;
#51010 = CARTESIAN_POINT ( 'NONE',  ( -19.60834386242827776, 0.000000000000000000, 4.298478389818581213 ) ) ;
#51011 = EDGE_CURVE ( 'NONE', #46331, #34260, #17090, .T. ) ;
#51012 = EDGE_LOOP ( 'NONE', ( #227, #8449, #50589, #31632 ) ) ;
#51013 = EDGE_CURVE ( 'NONE', #37711, #55849, #38676, .T. ) ;
#51014 = AXIS2_PLACEMENT_3D ( 'NONE', #2670, #54627, #15733 ) ;
#51015 = VECTOR ( 'NONE', #43390, 999.9999999999998863 ) ;
#51016 = CARTESIAN_POINT ( 'NONE',  ( -66.20424668929096867, -9.286518117000532868, 2.845885083223566703 ) ) ;
#51017 = CARTESIAN_POINT ( 'NONE',  ( -9.342070512798265725, 0.000000000000000000, 10.59882438848031505 ) ) ;
#51018 = CARTESIAN_POINT ( 'NONE',  ( -68.96626428157883026, -10.65111260844145313, -7.493887922408438484 ) ) ;
#51019 = ADVANCED_FACE ( 'NONE', ( #16233 ), #15963, .F. ) ;
#51020 = EDGE_LOOP ( 'NONE', ( #54016, #17086, #28471, #19466 ) ) ;
#51021 = DIRECTION ( 'NONE',  ( -0.5449076811759708816, 0.6444004775717707689, 0.5364919789714475140 ) ) ;
#51022 = ORIENTED_EDGE ( 'NONE', *, *, #10810, .T. ) ;
#51023 = FACE_OUTER_BOUND ( 'NONE', #43683, .T. ) ;
#51024 = EDGE_CURVE ( 'NONE', #1477, #36530, #34406, .T. ) ;
#51025 = AXIS2_PLACEMENT_3D ( 'NONE', #41127, #2214, #19551 ) ;
#51026 = DIRECTION ( 'NONE',  ( -0.7660212471507179544, -0.6427876096865405842, -0.005961354470445141482 ) ) ;
#51027 = VECTOR ( 'NONE', #40775, 1000.000000000000227 ) ;
#51028 = EDGE_CURVE ( 'NONE', #7819, #26523, #51456, .T. ) ;
#51029 = DIRECTION ( 'NONE',  ( -0.9999697198139514409, -0.000000000000000000, -0.007781995580013368816 ) ) ;
#51030 = CARTESIAN_POINT ( 'NONE',  ( -14.52490551429942656, -3.432230869623160263, 7.956773887985201021 ) ) ;
#51031 = DIRECTION ( 'NONE',  ( 0.007781995580012663651, 0.000000000000000000, -0.9999697198139515519 ) ) ;
#51032 = CARTESIAN_POINT ( 'NONE',  ( -18.15625413466447569, 0.000000000000000000, 8.741763725523435724 ) ) ;
#51033 = CARTESIAN_POINT ( 'NONE',  ( -12.88624579210203436, -4.241740624735661491, 8.648806222517640308 ) ) ;
#51034 = CARTESIAN_POINT ( 'NONE',  ( -11.13652411806909903, 0.000000000000000000, 2.348421687366606392 ) ) ;
#51035 = VERTEX_POINT ( 'NONE', #55403 ) ;
#51036 = FACE_OUTER_BOUND ( 'NONE', #48063, .T. ) ;
#51037 = ORIENTED_EDGE ( 'NONE', *, *, #12524, .T. ) ;
#51038 = VECTOR ( 'NONE', #5031, 1000.000000000000227 ) ;
#51039 = EDGE_CURVE ( 'NONE', #32426, #31757, #46312, .T. ) ;
#51040 = LINE ( 'NONE', #3631, #31089 ) ;
#51041 = DIRECTION ( 'NONE',  ( 0.005961354470445682716, -0.6427876096865404731, -0.7660212471507180654 ) ) ;
#51042 = CARTESIAN_POINT ( 'NONE',  ( -20.18285418839233714, 0.000000000000000000, 4.621332403721110538 ) ) ;
#51043 = VECTOR ( 'NONE', #42611, 1000.000000000000227 ) ;
#51044 = CARTESIAN_POINT ( 'NONE',  ( -14.61041236884574879, 0.000000000000000000, 5.076037587973862841 ) ) ;
#51045 = PLANE ( 'NONE',  #30410 ) ;
#51046 = ADVANCED_FACE ( 'NONE', ( #16804 ), #46914, .F. ) ;
#51047 = LINE ( 'NONE', #33465, #48250 ) ;
#51048 = APPLICATION_PROTOCOL_DEFINITION ( 'draft international standard', 'automotive_design', 1998, #9746 ) ;
#51049 = ORIENTED_EDGE ( 'NONE', *, *, #39477, .T. ) ;
#51050 = CARTESIAN_POINT ( 'NONE',  ( -12.38502494873981163, 1.257817950434005683, 1.452565040780329886 ) ) ;
#51051 = VECTOR ( 'NONE', #14497, 1000.000000000000114 ) ;
#51052 = DIRECTION ( 'NONE',  ( 0.005002170337468016433, -0.7660444431189770143, -0.6427681459581293666 ) ) ;
#51053 = CARTESIAN_POINT ( 'NONE',  ( -11.20636620717317378, 0.000000000000000000, 11.32298014792380414 ) ) ;
#51054 = CARTESIAN_POINT ( 'NONE',  ( -21.47419595591918906, 0.000000000000000000, 5.222628093224860102 ) ) ;
#51055 = VECTOR ( 'NONE', #41638, 1000.000000000000227 ) ;
#51056 = VECTOR ( 'NONE', #17608, 1000.000000000000227 ) ;
#51057 = LINE ( 'NONE', #11622, #10976 ) ;
#51058 = DIRECTION ( 'NONE',  ( -0.7660212471507179544, -0.6427876096865405842, -0.005961354470445141482 ) ) ;
#51059 = DIRECTION ( 'NONE',  ( 0.5364919789714477361, 0.6444004775717706579, 0.5449076811759711036 ) ) ;
#51060 = CARTESIAN_POINT ( 'NONE',  ( -18.19747506107908563, 0.000000000000000000, 14.03856424583689311 ) ) ;
#51061 = ORIENTED_EDGE ( 'NONE', *, *, #50823, .T. ) ;
#51062 = AXIS2_PLACEMENT_3D ( 'NONE', #41997, #3098, #20431 ) ;
#51063 = DIRECTION ( 'NONE',  ( 0.7660212471507180654, -0.6427876096865404731, 0.005961354470445141482 ) ) ;
#51064 = AXIS2_PLACEMENT_3D ( 'NONE', #49472, #44086, #27050 ) ;
#51065 = LINE ( 'NONE', #46239, #18850 ) ;
#51066 = VERTEX_POINT ( 'NONE', #50604 ) ;
#51067 = ORIENTED_EDGE ( 'NONE', *, *, #10725, .T. ) ;
#51068 = FACE_OUTER_BOUND ( 'NONE', #51131, .T. ) ;
#51069 = ORIENTED_EDGE ( 'NONE', *, *, #49848, .F. ) ;
#51070 = ADVANCED_FACE ( 'NONE', ( #55696 ), #12554, .F. ) ;
#51071 = CARTESIAN_POINT ( 'NONE',  ( -14.00280974873554030, 0.000000000000000000, 12.40921378708904044 ) ) ;
#51072 = VECTOR ( 'NONE', #6986, 999.9999999999998863 ) ;
#51073 = ORIENTED_EDGE ( 'NONE', *, *, #38751, .T. ) ;
#51074 = ORIENTED_EDGE ( 'NONE', *, *, #16748, .F. ) ;
#51075 = ORIENTED_EDGE ( 'NONE', *, *, #18478, .T. ) ;
#51076 = SHAPE_REPRESENTATION ( 'BR-836', ( #23538, #9037, #53454, #42584, #33510, #55268 ), #27156 ) ;
#51077 = FACE_OUTER_BOUND ( 'NONE', #28783, .T. ) ;
#51078 = CARTESIAN_POINT ( 'NONE',  ( -14.01701317841955508, 0.000000000000000000, 2.326005055450897085 ) ) ;
#51079 = PLANE ( 'NONE',  #42093 ) ;
#51080 = EDGE_CURVE ( 'NONE', #9247, #19141, #7423, .T. ) ;
#51081 = VECTOR ( 'NONE', #99, 1000.000000000000227 ) ;
#51082 = EDGE_CURVE ( 'NONE', #48904, #51697, #33834, .T. ) ;
#51083 = VERTEX_POINT ( 'NONE', #21042 ) ;
#51084 = EDGE_LOOP ( 'NONE', ( #33758, #21205, #46918, #12146 ) ) ;
#51085 = AXIS2_PLACEMENT_3D ( 'NONE', #50297, #46049, #7156 ) ;
#51086 = ADVANCED_FACE ( 'NONE', ( #7723 ), #8013, .F. ) ;
#51087 = FACE_OUTER_BOUND ( 'NONE', #19745, .T. ) ;
#51088 = CARTESIAN_POINT ( 'NONE',  ( -20.54049170961573267, 0.000000000000000000, 4.660556269540326646 ) ) ;
#51089 = EDGE_LOOP ( 'NONE', ( #53704, #33487, #38315, #55159 ) ) ;
#51090 = AXIS2_PLACEMENT_3D ( 'NONE', #54484, #37456, #54775 ) ;
#51091 = DIRECTION ( 'NONE',  ( -0.7660212471507179544, -0.6427876096865405842, -0.005961354470445141482 ) ) ;
#51092 = CARTESIAN_POINT ( 'NONE',  ( -12.80458192191714595, 0.000000000000000000, 11.86454056839041726 ) ) ;
#51093 = ORIENTED_EDGE ( 'NONE', *, *, #22579, .T. ) ;
#51094 = DIRECTION ( 'NONE',  ( 0.000000000000000000, -1.000000000000000000, 0.000000000000000000 ) ) ;
#51095 = DIRECTION ( 'NONE',  ( -0.7660212471507179544, -0.6427876096865405842, -0.005961354470445141482 ) ) ;
#51096 = AXIS2_PLACEMENT_3D ( 'NONE', #19395, #36737, #17668 ) ;
#51097 = VECTOR ( 'NONE', #44241, 999.9999999999998863 ) ;
#51098 = ORIENTED_EDGE ( 'NONE', *, *, #48178, .F. ) ;
#51099 = FACE_OUTER_BOUND ( 'NONE', #44081, .T. ) ;
#51100 = ADVANCED_FACE ( 'NONE', ( #25056 ), #29603, .F. ) ;
#51101 = ADVANCED_FACE ( 'NONE', ( #7167 ), #8271, .F. ) ;
#51102 = VECTOR ( 'NONE', #8195, 1000.000000000000227 ) ;
#51103 = LINE ( 'NONE', #46865, #4634 ) ;
#51104 = VECTOR ( 'NONE', #44789, 1000.000000000000114 ) ;
#51105 = ORIENTED_EDGE ( 'NONE', *, *, #44876, .T. ) ;
#51106 = DIRECTION ( 'NONE',  ( 0.7660212471507180654, -0.6427876096865404731, 0.005961354470445141482 ) ) ;
#51107 = DIRECTION ( 'NONE',  ( -0.9999697198139514409, -0.000000000000000000, -0.007781995580013368816 ) ) ;
#51108 = CARTESIAN_POINT ( 'NONE',  ( -0.8462754142284378833, 3.710276453311750267, 3.547095686184165153 ) ) ;
#51109 = CARTESIAN_POINT ( 'NONE',  ( -18.91945046336710590, 0.000000000000000000, 8.935830411442143628 ) ) ;
#51110 = ORIENTED_EDGE ( 'NONE', *, *, #15465, .F. ) ;
#51111 = ADVANCED_FACE ( 'NONE', ( #54852 ), #24746, .F. ) ;
#51112 = DIRECTION ( 'NONE',  ( -0.005961354470445682716, -0.6427876096865404731, 0.7660212471507180654 ) ) ;
#51113 = CARTESIAN_POINT ( 'NONE',  ( -15.89273142772683300, -0.1134144341942070200, 2.954903030296413657 ) ) ;
#51114 = LINE ( 'NONE', #21600, #27633 ) ;
#51115 = DIRECTION ( 'NONE',  ( -0.6427681459581293666, -0.7660444431189770143, -0.005002170337467561935 ) ) ;
#51116 = DIRECTION ( 'NONE',  ( -0.005002170337468016433, -0.7660444431189770143, 0.6427681459581293666 ) ) ;
#51117 = DIRECTION ( 'NONE',  ( 0.5364919789714477361, 0.6444004775717706579, 0.5449076811759711036 ) ) ;
#51118 = CARTESIAN_POINT ( 'NONE',  ( -68.76211497692452213, -11.59294684971063916, -7.108028418031229201 ) ) ;
#51119 = AXIS2_PLACEMENT_3D ( 'NONE', #50615, #50025, #32473 ) ;
#51120 = ORIENTED_EDGE ( 'NONE', *, *, #22715, .T. ) ;
#51121 = SURFACE_SIDE_STYLE ('',( #16474 ) ) ;
#51122 = LINE ( 'NONE', #20754, #26918 ) ;
#51123 = ORIENTED_EDGE ( 'NONE', *, *, #47856, .T. ) ;
#51124 = DIRECTION ( 'NONE',  ( -0.005961354470445682716, -0.6427876096865404731, 0.7660212471507180654 ) ) ;
#51125 = FACE_OUTER_BOUND ( 'NONE', #35263, .T. ) ;
#51126 = VECTOR ( 'NONE', #9867, 1000.000000000000114 ) ;
#51127 = CARTESIAN_POINT ( 'NONE',  ( -19.30004991711850337, -4.727446477803165514, 4.227285643902905399 ) ) ;
#51128 = VECTOR ( 'NONE', #38847, 1000.000000000000227 ) ;
#51129 = LINE ( 'NONE', #12237, #40564 ) ;
#51130 = PLANE ( 'NONE',  #28387 ) ;
#51131 = EDGE_LOOP ( 'NONE', ( #55302, #36486, #34355, #51795 ) ) ;
#51132 = ORIENTED_EDGE ( 'NONE', *, *, #42151, .F. ) ;
#51133 = LINE ( 'NONE', #11410, #15017 ) ;
#51134 = VECTOR ( 'NONE', #55998, 1000.000000000000227 ) ;
#51135 = DIRECTION ( 'NONE',  ( 0.9321478471874540261, 0.000000000000000000, -0.3620778797217457101 ) ) ;
#51136 = ORIENTED_EDGE ( 'NONE', *, *, #53604, .F. ) ;
#51137 = ADVANCED_FACE ( 'NONE', ( #52552 ), #610, .F. ) ;
#51138 = VECTOR ( 'NONE', #55106, 999.9999999999998863 ) ;
#51139 = LINE ( 'NONE', #32695, #13004 ) ;
#51140 = ORIENTED_EDGE ( 'NONE', *, *, #23995, .F. ) ;
#51141 = CARTESIAN_POINT ( 'NONE',  ( -14.01701317841955508, 0.000000000000000000, 2.326005055450897085 ) ) ;
#51142 = EDGE_CURVE ( 'NONE', #6164, #34166, #22735, .T. ) ;
#51143 = EDGE_LOOP ( 'NONE', ( #30850, #32179, #30796, #44212 ) ) ;
#51144 = FACE_OUTER_BOUND ( 'NONE', #38042, .T. ) ;
#51145 = VECTOR ( 'NONE', #1889, 1000.000000000000227 ) ;
#51146 = ORIENTED_EDGE ( 'NONE', *, *, #36244, .T. ) ;
#51147 = VECTOR ( 'NONE', #24266, 1000.000000000000227 ) ;
#51148 = EDGE_LOOP ( 'NONE', ( #43890, #23779, #18256, #25301 ) ) ;
#51149 = ORIENTED_EDGE ( 'NONE', *, *, #13831, .T. ) ;
#51150 = ADVANCED_FACE ( 'NONE', ( #40049 ), #39790, .F. ) ;
#51151 = LINE ( 'NONE', #47760, #307 ) ;
#51152 = CARTESIAN_POINT ( 'NONE',  ( -26.13415699229845757, -0.1191753592594197858, 6.933020519852192365 ) ) ;
#51153 = CARTESIAN_POINT ( 'NONE',  ( -15.94144280372852762, 2.714935509636508204, 2.787508833130166952 ) ) ;
#51154 = ADVANCED_FACE ( 'NONE', ( #26715 ), #44323, .T. ) ;
#51155 = EDGE_CURVE ( 'NONE', #23097, #2132, #47455, .T. ) ;
#51156 = ADVANCED_FACE ( 'NONE', ( #13404 ), #35513, .F. ) ;
#51157 = DIRECTION ( 'NONE',  ( 0.9999697198139515519, 0.000000000000000000, 0.007781995580013368816 ) ) ;
#51158 = ORIENTED_EDGE ( 'NONE', *, *, #46593, .T. ) ;
#51159 = ORIENTED_EDGE ( 'NONE', *, *, #10565, .F. ) ;
#51160 = AXIS2_PLACEMENT_3D ( 'NONE', #13807, #23196, #40785 ) ;
#51161 = ORIENTED_EDGE ( 'NONE', *, *, #2385, .F. ) ;
#51162 = LINE ( 'NONE', #33558, #20462 ) ;
#51163 = LINE ( 'NONE', #21, #20368 ) ;
#51164 = ORIENTED_EDGE ( 'NONE', *, *, #46529, .F. ) ;
#51165 = CARTESIAN_POINT ( 'NONE',  ( -15.11879971925641009, 4.981562823951510843, 10.92956963961542982 ) ) ;
#51166 = VERTEX_POINT ( 'NONE', #30964 ) ;
#51167 = AXIS2_PLACEMENT_3D ( 'NONE', #22569, #22832, #23128 ) ;
#51168 = LINE ( 'NONE', #42931, #15149 ) ;
#51169 = FACE_OUTER_BOUND ( 'NONE', #12688, .T. ) ;
#51170 = ORIENTED_EDGE ( 'NONE', *, *, #18549, .F. ) ;
#51171 = CARTESIAN_POINT ( 'NONE',  ( -17.26532721389163072, 0.000000000000000000, 13.67648636611514590 ) ) ;
#51172 = ADVANCED_FACE ( 'NONE', ( #51707 ), #43744, .F. ) ;
#51173 = ORIENTED_EDGE ( 'NONE', *, *, #35397, .F. ) ;
#51174 = EDGE_CURVE ( 'NONE', #25200, #606, #48279, .T. ) ;
#51175 = CARTESIAN_POINT ( 'NONE',  ( -21.47419595591918906, 0.000000000000000000, 5.222628093224860102 ) ) ;
#51176 = LINE ( 'NONE', #13601, #31110 ) ;
#51177 = AXIS2_PLACEMENT_3D ( 'NONE', #4419, #26263, #39630 ) ;
#51178 = ORIENTED_EDGE ( 'NONE', *, *, #49239, .T. ) ;
#51179 = CARTESIAN_POINT ( 'NONE',  ( -19.45503627000849889, -1.000000000000000000, 7.556996783084074742 ) ) ;
#51180 = CARTESIAN_POINT ( 'NONE',  ( -8.570132709911630897, 0.000000000000000000, 5.123044440957987611 ) ) ;
#51181 = EDGE_CURVE ( 'NONE', #16744, #16632, #9395, .T. ) ;
#51182 = CARTESIAN_POINT ( 'NONE',  ( -16.54374430921337691, 2.876837460659007473, 3.016297672218315906 ) ) ;
#51183 = VECTOR ( 'NONE', #10806, 1000.000000000000227 ) ;
#51184 = LINE ( 'NONE', #11723, #30990 ) ;
#51185 = ORIENTED_EDGE ( 'NONE', *, *, #45857, .T. ) ;
#51186 = AXIS2_PLACEMENT_3D ( 'NONE', #2509, #41674, #54447 ) ;
#51188 = ORIENTED_EDGE ( 'NONE', *, *, #39402, .T. ) ;
#51187 = EDGE_CURVE ( 'NONE', #17041, #54371, #13931, .T. ) ;
#51189 = FACE_OUTER_BOUND ( 'NONE', #30852, .T. ) ;
#51190 = DIRECTION ( 'NONE',  ( 0.7660212471507180654, -0.6427876096865404731, 0.005961354470445141482 ) ) ;
#51191 = DIRECTION ( 'NONE',  ( 0.9999697198139515519, 0.000000000000000000, 0.007781995580013368816 ) ) ;
#51192 = DIRECTION ( 'NONE',  ( 0.005961354470445682716, -0.6427876096865404731, -0.7660212471507180654 ) ) ;
#51193 = ADVANCED_FACE ( 'NONE', ( #48585 ), #25898, .F. ) ;
#51194 = PLANE ( 'NONE',  #54189 ) ;
#51195 = AXIS2_PLACEMENT_3D ( 'NONE', #17147, #30202, #13168 ) ;
#51196 = AXIS2_PLACEMENT_3D ( 'NONE', #12065, #46413, #12382 ) ;
#51197 = LINE ( 'NONE', #11467, #48507 ) ;
#51198 = ORIENTED_EDGE ( 'NONE', *, *, #10071, .F. ) ;
#51199 = DIRECTION ( 'NONE',  ( -0.5364919789714478471, 0.6444004775717705469, -0.5449076811759709926 ) ) ;
#51200 = CARTESIAN_POINT ( 'NONE',  ( -9.908141408373387193, -0.1191753592594197858, 10.77908512878318703 ) ) ;
#51201 = ORIENTED_EDGE ( 'NONE', *, *, #25075, .T. ) ;
#51202 = CARTESIAN_POINT ( 'NONE',  ( -22.40478740399063895, 0.000000000000000000, 5.384712028983816623 ) ) ;
#51203 = EDGE_LOOP ( 'NONE', ( #52233, #9108, #1962, #40114 ) ) ;
#51204 = CARTESIAN_POINT ( 'NONE',  ( -16.53317331066696383, 0.000000000000000000, 13.31285208727739899 ) ) ;
#51205 = DIRECTION ( 'NONE',  ( 0.007781995580012663651, 0.000000000000000000, -0.9999697198139515519 ) ) ;
#51206 = LINE ( 'NONE', #29660, #24120 ) ;
#51207 = DIRECTION ( 'NONE',  ( -0.005961354470445682716, -0.6427876096865404731, 0.7660212471507180654 ) ) ;
#51208 = CARTESIAN_POINT ( 'NONE',  ( -69.53119166430043663, 1.999999999951586060, 7.127210919673932388 ) ) ;
#51209 = VECTOR ( 'NONE', #45091, 999.9999999999998863 ) ;
#51210 = VERTEX_POINT ( 'NONE', #38948 ) ;
#51211 = EDGE_LOOP ( 'NONE', ( #5420, #15970, #53292, #12632 ) ) ;
#51212 = AXIS2_PLACEMENT_3D ( 'NONE', #24394, #7100, #49410 ) ;
#51213 = CARTESIAN_POINT ( 'NONE',  ( -67.46601601628378830, -0.6012495896919525240, -3.320464512871842189 ) ) ;
#51214 = FACE_OUTER_BOUND ( 'NONE', #24977, .T. ) ;
#51215 = FACE_OUTER_BOUND ( 'NONE', #16198, .T. ) ;
#51216 = VECTOR ( 'NONE', #38123, 999.9999999999998863 ) ;
#51217 = DIRECTION ( 'NONE',  ( -0.7660212471507179544, -0.6427876096865405842, -0.005961354470445141482 ) ) ;
#51218 = CARTESIAN_POINT ( 'NONE',  ( -13.62138192979224272, -0.1941918491731554897, 2.166132706095718508 ) ) ;
#51219 = DIRECTION ( 'NONE',  ( 0.000000000000000000, -1.000000000000000000, 0.000000000000000000 ) ) ;
#51220 = AXIS2_PLACEMENT_3D ( 'NONE', #36123, #44907, #6026 ) ;
#51221 = ORIENTED_EDGE ( 'NONE', *, *, #7322, .F. ) ;
#51222 = PLANE ( 'NONE',  #52832 ) ;
#51223 = DIRECTION ( 'NONE',  ( -0.3620778797217457656, 0.000000000000000000, -0.9321478471874539151 ) ) ;
#51224 = CARTESIAN_POINT ( 'NONE',  ( -15.60102546347950536, 0.000000000000000000, 12.95077420755565356 ) ) ;
#51225 = VECTOR ( 'NONE', #51888, 1000.000000000000000 ) ;
#51227 = ORIENTED_EDGE ( 'NONE', *, *, #27144, .T. ) ;
#51226 = VECTOR ( 'NONE', #2835, 999.9999999999998863 ) ;
#51228 = AXIS2_PLACEMENT_3D ( 'NONE', #22046, #30849, #31123 ) ;
#51229 = FACE_OUTER_BOUND ( 'NONE', #8555, .T. ) ;
#51230 = DIRECTION ( 'NONE',  ( -0.7660212471507179544, -0.6427876096865405842, -0.005961354470445141482 ) ) ;
#51231 = CARTESIAN_POINT ( 'NONE',  ( -16.44024919480531821, -2.946525016555658016, 7.903632366987483060 ) ) ;
#51232 = AXIS2_PLACEMENT_3D ( 'NONE', #55371, #16470, #46879 ) ;
#51233 = ADVANCED_FACE ( 'NONE', ( #298 ), #17344, .F. ) ;
#51234 = ADVANCED_FACE ( 'NONE', ( #30436 ), #47761, .F. ) ;
#51235 = ORIENTED_EDGE ( 'NONE', *, *, #25260, .T. ) ;
#51236 = LINE ( 'NONE', #39016, #22299 ) ;
#51237 = EDGE_LOOP ( 'NONE', ( #20185, #44787, #49120, #38496 ) ) ;
#51238 = ADVANCED_FACE ( 'NONE', ( #39208 ), #34981, .F. ) ;
#51239 = VECTOR ( 'NONE', #53657, 1000.000000000000227 ) ;
#51240 = EDGE_LOOP ( 'NONE', ( #29750, #396 ) ) ;
#51241 = VECTOR ( 'NONE', #2701, 1000.000000000000114 ) ;
#51242 = VERTEX_POINT ( 'NONE', #9115 ) ;
#51243 = ORIENTED_EDGE ( 'NONE', *, *, #45901, .T. ) ;
#51244 = CARTESIAN_POINT ( 'NONE',  ( -23.33849165029409889, 0.000000000000000000, 5.946783852668351855 ) ) ;
#51245 = EDGE_LOOP ( 'NONE', ( #6956, #38379, #25052, #55388 ) ) ;
#51246 = CARTESIAN_POINT ( 'NONE',  ( -12.42987990997295711, 23.74983052629447045, -3.542935327883032226 ) ) ;
#51247 = EDGE_LOOP ( 'NONE', ( #54157, #25755, #3820, #42400 ) ) ;
#51248 = FACE_OUTER_BOUND ( 'NONE', #3464, .T. ) ;
#51249 = ORIENTED_EDGE ( 'NONE', *, *, #43315, .T. ) ;
#51250 = ORIENTED_EDGE ( 'NONE', *, *, #35532, .T. ) ;
#51251 = AXIS2_PLACEMENT_3D ( 'NONE', #35955, #10078, #44432 ) ;
#51252 = DIRECTION ( 'NONE',  ( 0.005002170337468016433, -0.7660444431189770143, -0.6427681459581293666 ) ) ;
#51253 = DIRECTION ( 'NONE',  ( 0.5364919789714477361, 0.6444004775717706579, 0.5449076811759711036 ) ) ;
#51254 = PLANE ( 'NONE',  #44008 ) ;
#51255 = CARTESIAN_POINT ( 'NONE',  ( 2.072287782118878319, 0.000000000000000000, -2.950529333540147015 ) ) ;
#51256 = CARTESIAN_POINT ( 'NONE',  ( -7.337759244690715832, 5.055610077911836697, -0.3681386936730630666 ) ) ;
#51257 = AXIS2_PLACEMENT_3D ( 'NONE', #47274, #13759, #52401 ) ;
#51258 = VERTEX_POINT ( 'NONE', #23843 ) ;
#51259 = ORIENTED_EDGE ( 'NONE', *, *, #14359, .T. ) ;
#51260 = DIRECTION ( 'NONE',  ( -0.7660212471507179544, -0.6427876096865405842, -0.005961354470445141482 ) ) ;
#51261 = FACE_OUTER_BOUND ( 'NONE', #22575, .T. ) ;
#51262 = VECTOR ( 'NONE', #45374, 1000.000000000000227 ) ;
#51263 = UNCERTAINTY_MEASURE_WITH_UNIT (LENGTH_MEASURE( 1.000000000000000082E-05 ), #26396, 'distance_accuracy_value', 'NONE');
#51264 = ADVANCED_FACE ( 'NONE', ( #45173 ), #6274, .F. ) ;
#51265 = DIRECTION ( 'NONE',  ( 0.9999697198139515519, 0.000000000000000000, 0.007781995580013368816 ) ) ;
#51266 = AXIS2_PLACEMENT_3D ( 'NONE', #38963, #29, #26187 ) ;
#51267 = VECTOR ( 'NONE', #24611, 1000.000000000000114 ) ;
#51268 = CARTESIAN_POINT ( 'NONE',  ( -13.53673582514181106, 0.000000000000000000, 12.22817484722816772 ) ) ;
#51269 = EDGE_CURVE ( 'NONE', #25448, #39671, #1440, .T. ) ;
#51270 = AXIS2_PLACEMENT_3D ( 'NONE', #24720, #11940, #46892 ) ;
#51271 = DIRECTION ( 'NONE',  ( -0.005961354470445682716, -0.6427876096865404731, 0.7660212471507180654 ) ) ;
#51272 = CARTESIAN_POINT ( 'NONE',  ( -12.70458494993575194, -0.1191753592594197858, 11.86531876794841978 ) ) ;
#51273 = ORIENTED_EDGE ( 'NONE', *, *, #29298, .T. ) ;
#51274 = DIRECTION ( 'NONE',  ( 0.5364919789714477361, 0.6444004775717706579, 0.5449076811759711036 ) ) ;
#51275 = EDGE_CURVE ( 'NONE', #36877, #16502, #1708, .T. ) ;
#51276 = CARTESIAN_POINT ( 'NONE',  ( -11.14071582596366383, 0.000000000000000000, 2.887047149919346634 ) ) ;
#51277 = ORIENTED_EDGE ( 'NONE', *, *, #34056, .F. ) ;
#51278 = VECTOR ( 'NONE', #37735, 999.9999999999998863 ) ;
#51279 = DIRECTION ( 'NONE',  ( -0.000000000000000000, -0.000000000000000000, -1.000000000000000000 ) ) ;
#51280 = CARTESIAN_POINT ( 'NONE',  ( -9.542064456761055524, 0.000000000000000000, 10.59726798936431180 ) ) ;
#51281 = AXIS2_PLACEMENT_3D ( 'NONE', #11440, #6607, #10319 ) ;
#51282 = DIRECTION ( 'NONE',  ( -0.9999697198139514409, -0.000000000000000000, -0.007781995580013368816 ) ) ;
#51283 = EDGE_CURVE ( 'NONE', #14403, #12863, #1969, .T. ) ;
#51284 = CARTESIAN_POINT ( 'NONE',  ( -12.35196013617144217, 1.743523803501505709, 4.540661504268221016 ) ) ;
#51285 = FACE_OUTER_BOUND ( 'NONE', #24979, .T. ) ;
#51286 = AXIS2_PLACEMENT_3D ( 'NONE', #27990, #31955, #45034 ) ;
#51287 = ORIENTED_EDGE ( 'NONE', *, *, #53423, .T. ) ;
#51288 = VECTOR ( 'NONE', #56034, 1000.000000000000227 ) ;
#51289 = EDGE_LOOP ( 'NONE', ( #17075, #9995, #44126, #41642 ) ) ;
#51290 = DIRECTION ( 'NONE',  ( -0.9999697198139514409, -0.000000000000000000, -0.007781995580013368816 ) ) ;
#51291 = CARTESIAN_POINT ( 'NONE',  ( -13.08330893211609869, 0.000000000000000000, 1.763933231766363630 ) ) ;
#51292 = FACE_OUTER_BOUND ( 'NONE', #2423, .T. ) ;
#51293 = PLANE ( 'NONE',  #9235 ) ;
#51294 = DIRECTION ( 'NONE',  ( -0.005961354470445682716, -0.6427876096865404731, 0.7660212471507180654 ) ) ;
#51295 = CARTESIAN_POINT ( 'NONE',  ( -57.29829478218162109, -10.27834239552269935, 3.000000000000005773 ) ) ;
#51296 = DIRECTION ( 'NONE',  ( 0.7660212471507180654, -0.6427876096865404731, 0.005961354470445141482 ) ) ;
#51297 = VECTOR ( 'NONE', #6879, 999.9999999999998863 ) ;
#51298 = CARTESIAN_POINT ( 'NONE',  ( -20.54204810873173415, 0.000000000000000000, 4.860550213503115558 ) ) ;
#51299 = DIRECTION ( 'NONE',  ( 0.005002170337468016433, -0.7660444431189770143, -0.6427681459581293666 ) ) ;
#51300 = AXIS2_PLACEMENT_3D ( 'NONE', #26513, #40135, #9483 ) ;
#51301 = CARTESIAN_POINT ( 'NONE',  ( -12.80458192191714595, 0.000000000000000000, 11.86454056839041726 ) ) ;
#51302 = ORIENTED_EDGE ( 'NONE', *, *, #31232, .T. ) ;
#51303 = LINE ( 'NONE', #26042, #24043 ) ;
#51304 = VECTOR ( 'NONE', #16691, 1000.000000000000000 ) ;
#51305 = EDGE_CURVE ( 'NONE', #32412, #24071, #36103, .T. ) ;
#51306 = VERTEX_POINT ( 'NONE', #18783 ) ;
#51307 = AXIS2_PLACEMENT_3D ( 'NONE', #27298, #44611, #39551 ) ;
#51308 = ORIENTED_EDGE ( 'NONE', *, *, #47590, .T. ) ;
#51309 = ADVANCED_FACE ( 'NONE', ( #14246 ), #45699, .F. ) ;
#51310 = EDGE_CURVE ( 'NONE', #33398, #21014, #53406, .T. ) ;
#51311 = ORIENTED_EDGE ( 'NONE', *, *, #11715, .T. ) ;
#51312 = ORIENTED_EDGE ( 'NONE', *, *, #15340, .T. ) ;
#51313 = VECTOR ( 'NONE', #20798, 999.9999999999998863 ) ;
#51314 = ORIENTED_EDGE ( 'NONE', *, *, #56000, .F. ) ;
#51315 = VERTEX_POINT ( 'NONE', #9965 ) ;
#51316 = CARTESIAN_POINT ( 'NONE',  ( -57.29829478218162109, -10.27834239552269580, -2.999999999999996891 ) ) ;
#51317 = CARTESIAN_POINT ( 'NONE',  ( -58.00000000000000711, -9.000000000000000000, 7.102951435054649637E-15 ) ) ;
#51318 = LINE ( 'NONE', #37697, #16729 ) ;
#51319 = VECTOR ( 'NONE', #27120, 1000.000000000000000 ) ;
#51320 = VECTOR ( 'NONE', #48162, 999.9999999999998863 ) ;
#51321 = ORIENTED_EDGE ( 'NONE', *, *, #6055, .F. ) ;
#51322 = DIRECTION ( 'NONE',  ( 0.005961354470445682716, -0.6427876096865404731, -0.7660212471507180654 ) ) ;
#51323 = VECTOR ( 'NONE', #38017, 999.9999999999998863 ) ;
#51324 = ORIENTED_EDGE ( 'NONE', *, *, #19630, .T. ) ;
#51325 = CARTESIAN_POINT ( 'NONE',  ( -66.08210154591968433, -11.28561844313478524, 6.312544413184012271 ) ) ;
#51326 = VERTEX_POINT ( 'NONE', #44584 ) ;
#51327 = EDGE_CURVE ( 'NONE', #29013, #55101, #32107, .T. ) ;
#51328 = AXIS2_PLACEMENT_3D ( 'NONE', #35971, #9549, #18624 ) ;
#51329 = AXIS2_PLACEMENT_3D ( 'NONE', #720, #43868, #48122 ) ;
#51330 = DIRECTION ( 'NONE',  ( 0.6427681459581294776, -0.7660444431189769032, 0.005002170337467562802 ) ) ;
#51331 = DIRECTION ( 'NONE',  ( 0.5364919789714477361, 0.6444004775717706579, 0.5449076811759711036 ) ) ;
#51332 = PLANE ( 'NONE',  #35945 ) ;
#51333 = ORIENTED_EDGE ( 'NONE', *, *, #12474, .F. ) ;
#51334 = LINE ( 'NONE', #16127, #2903 ) ;
#51335 = ORIENTED_EDGE ( 'NONE', *, *, #13612, .F. ) ;
#51336 = LINE ( 'NONE', #34855, #20076 ) ;
#51337 = DIRECTION ( 'NONE',  ( 0.005961354470445682716, -0.6427876096865404731, -0.7660212471507180654 ) ) ;
#51338 = VECTOR ( 'NONE', #26701, 999.9999999999998863 ) ;
#51339 = FACE_OUTER_BOUND ( 'NONE', #8267, .T. ) ;
#51340 = CARTESIAN_POINT ( 'NONE',  ( -10.19678563399013527, 0.000000000000000000, 0.7424042488757021108 ) ) ;
#51341 = LINE ( 'NONE', #25483, #49259 ) ;
#51342 = CARTESIAN_POINT ( 'NONE',  ( -23.33693525117809386, 0.000000000000000000, 5.746789908705562944 ) ) ;
#51343 = CARTESIAN_POINT ( 'NONE',  ( -26.13337879274045505, 0.000000000000000000, 6.833023547870798353 ) ) ;
#51344 = LINE ( 'NONE', #47073, #15904 ) ;
#51345 = ORIENTED_EDGE ( 'NONE', *, *, #15082, .T. ) ;
#51346 = CARTESIAN_POINT ( 'NONE',  ( -55.98099385706747455, 6.802457008950081097, -1.869625304823616219 ) ) ;
#51347 = EDGE_LOOP ( 'NONE', ( #46514, #54477, #31499, #53996 ) ) ;
#51348 = AXIS2_PLACEMENT_3D ( 'NONE', #20551, #43269, #25631 ) ;
#51349 = CARTESIAN_POINT ( 'NONE',  ( -20.84197899872282633, 20.43270222331197061, -4.347644189607536624 ) ) ;
#51350 = CARTESIAN_POINT ( 'NONE',  ( -16.53317331066696383, 0.000000000000000000, 13.31285208727739899 ) ) ;
#51351 = DIRECTION ( 'NONE',  ( -0.9999697198139514409, -0.000000000000000000, -0.007781995580013368816 ) ) ;
#51352 = EDGE_CURVE ( 'NONE', #32666, #54093, #2547, .T. ) ;
#51353 = AXIS2_PLACEMENT_3D ( 'NONE', #15306, #49385, #6240 ) ;
#51354 = DIRECTION ( 'NONE',  ( 0.9999697198139515519, 0.000000000000000000, 0.007781995580013368816 ) ) ;
#51355 = DIRECTION ( 'NONE',  ( 0.000000000000000000, -1.000000000000000000, 0.000000000000000000 ) ) ;
#51356 = VECTOR ( 'NONE', #26137, 999.9999999999998863 ) ;
#51358 = VECTOR ( 'NONE', #28408, 999.9999999999998863 ) ;
#51357 = DIRECTION ( 'NONE',  ( 0.005961354470445682716, -0.6427876096865404731, -0.7660212471507180654 ) ) ;
#51359 = ORIENTED_EDGE ( 'NONE', *, *, #37050, .T. ) ;
#51360 = DIRECTION ( 'NONE',  ( -0.9999697198139514409, -0.000000000000000000, -0.007781995580013368816 ) ) ;
#51361 = DIRECTION ( 'NONE',  ( 0.6427681459581294776, -0.7660444431189769032, 0.005002170337467562802 ) ) ;
#51362 = CARTESIAN_POINT ( 'NONE',  ( -15.77426360813536554, 4.657758921906511418, 10.65275670580245482 ) ) ;
#51363 = VECTOR ( 'NONE', #46230, 1000.000000000000114 ) ;
#51364 = EDGE_CURVE ( 'NONE', #35036, #26534, #49707, .T. ) ;
#51365 = AXIS2_PLACEMENT_3D ( 'NONE', #14336, #5508, #22563 ) ;
#51366 = DIRECTION ( 'NONE',  ( 0.000000000000000000, -1.000000000000000000, 0.000000000000000000 ) ) ;
#51367 = CYLINDRICAL_SURFACE ( 'NONE', #36608, 0.7500000000000006661 ) ;
#51368 = ADVANCED_FACE ( 'NONE', ( #28382 ), #32651, .F. ) ;
#51369 = PLANE ( 'NONE',  #36824 ) ;
#51370 = EDGE_CURVE ( 'NONE', #33398, #8596, #27270, .T. ) ;
#51371 = CARTESIAN_POINT ( 'NONE',  ( -11.30636317915456779, -0.1191753592594197858, 11.32220194836580340 ) ) ;
#51372 = ORIENTED_EDGE ( 'NONE', *, *, #31045, .F. ) ;
#51373 = VECTOR ( 'NONE', #5161, 1000.000000000000227 ) ;
#51375 = DIRECTION ( 'NONE',  ( 0.007781995580012663651, 0.000000000000000000, -0.9999697198139515519 ) ) ;
#51374 = AXIS2_PLACEMENT_3D ( 'NONE', #31395, #23680, #6124 ) ;
#51376 = DIRECTION ( 'NONE',  ( -0.6427681459581293666, -0.7660444431189770143, -0.005002170337467561935 ) ) ;
#51377 = ORIENTED_EDGE ( 'NONE', *, *, #48987, .T. ) ;
#51378 = VERTEX_POINT ( 'NONE', #45418 ) ;
#51379 = PLANE ( 'NONE',  #25609 ) ;
#51380 = EDGE_CURVE ( 'NONE', #31427, #10254, #35813, .T. ) ;
#51381 = ORIENTED_EDGE ( 'NONE', *, *, #17247, .F. ) ;
#51382 = EDGE_CURVE ( 'NONE', #15410, #43254, #5693, .T. ) ;
#51383 = ADVANCED_FACE ( 'NONE', ( #36353 ), #49422, .F. ) ;
#51384 = VECTOR ( 'NONE', #47982, 1000.000000000000227 ) ;
#51385 = ORIENTED_EDGE ( 'NONE', *, *, #49549, .F. ) ;
#51386 = ORIENTED_EDGE ( 'NONE', *, *, #4608, .T. ) ;
#51387 = EDGE_LOOP ( 'NONE', ( #47972, #9556, #44462, #52014 ) ) ;
#51388 = DIRECTION ( 'NONE',  ( 0.9999697198139515519, 0.000000000000000000, 0.007781995580013368816 ) ) ;
#51389 = CARTESIAN_POINT ( 'NONE',  ( -19.52961462879997967, -2.784623065533159636, 4.378442612619098284 ) ) ;
#51390 = AXIS2_PLACEMENT_3D ( 'NONE', #17970, #31597, #44620 ) ;
#51391 = FACE_OUTER_BOUND ( 'NONE', #38031, .T. ) ;
#51392 = EDGE_CURVE ( 'NONE', #23998, #33602, #14779, .T. ) ;
#51393 = AXIS2_PLACEMENT_3D ( 'NONE', #15515, #1892, #40565 ) ;
#51394 = VERTEX_POINT ( 'NONE', #10541 ) ;
#51395 = VERTEX_POINT ( 'NONE', #28114 ) ;
#51396 = ADVANCED_FACE ( 'NONE', ( #6533 ), #24982, .F. ) ;
#51397 = VECTOR ( 'NONE', #20689, 999.9999999999998863 ) ;
#51398 = DIRECTION ( 'NONE',  ( 0.005961354470445682716, -0.6427876096865404731, -0.7660212471507180654 ) ) ;
#51399 = DIRECTION ( 'NONE',  ( 0.6427681459581294776, -0.7660444431189769032, 0.005002170337467562802 ) ) ;
#51400 = VERTEX_POINT ( 'NONE', #7357 ) ;
#51401 = DIRECTION ( 'NONE',  ( 0.9999697198139515519, 0.000000000000000000, 0.007781995580013368816 ) ) ;
#51402 = CARTESIAN_POINT ( 'NONE',  ( -19.90235142260334911, -4.889348428825664783, 4.456074482991054353 ) ) ;
#51403 = ORIENTED_EDGE ( 'NONE', *, *, #53587, .T. ) ;
#51404 = DIRECTION ( 'NONE',  ( -0.2426528472758541499, 0.7422098413412800966, -0.6246952433987894571 ) ) ;
#51405 = ORIENTED_EDGE ( 'NONE', *, *, #52743, .F. ) ;
#51406 = AXIS2_PLACEMENT_3D ( 'NONE', #48230, #26969, #19256 ) ;
#51407 = CARTESIAN_POINT ( 'NONE',  ( -17.83749246818616996, -1.327505506330657781, 3.767654579712751861 ) ) ;
#51408 = VECTOR ( 'NONE', #14175, 999.9999999999998863 ) ;
#51409 = DIRECTION ( 'NONE',  ( -0.5449076811759708816, 0.6444004775717707689, 0.5364919789714475140 ) ) ;
#51410 = AXIS2_PLACEMENT_3D ( 'NONE', #37817, #42352, #37513 ) ;
#51411 = ORIENTED_EDGE ( 'NONE', *, *, #1036, .F. ) ;
#51412 = FACE_OUTER_BOUND ( 'NONE', #26712, .T. ) ;
#51413 = CARTESIAN_POINT ( 'NONE',  ( -9.808144436391993182, 0.000000000000000000, 10.77986332834118777 ) ) ;
#51414 = CARTESIAN_POINT ( 'NONE',  ( -15.15892537552479702, -0.3560938001956562293, 3.154583738431461892 ) ) ;
#51415 = DIRECTION ( 'NONE',  ( 0.5364919789714477361, 0.6444004775717706579, 0.5449076811759711036 ) ) ;
#51416 = VERTEX_POINT ( 'NONE', #33232 ) ;
#51417 = LINE ( 'NONE', #17599, #181 ) ;
#51418 = LINE ( 'NONE', #21850, #25126 ) ;
#51419 = CARTESIAN_POINT ( 'NONE',  ( -18.62175513582871034, 4.172053068839010059, 10.96169306452648229 ) ) ;
#51420 = EDGE_CURVE ( 'NONE', #7759, #13509, #20432, .T. ) ;
#51421 = DIRECTION ( 'NONE',  ( 0.6427681459581294776, -0.7660444431189769032, 0.005002170337467562802 ) ) ;
#51422 = DIRECTION ( 'NONE',  ( 0.007781995580012662783, 0.000000000000000000, -0.9999697198139514409 ) ) ;
#51423 = PLANE ( 'NONE',  #43378 ) ;
#51424 = VECTOR ( 'NONE', #53150, 999.9999999999998863 ) ;
#51425 = LINE ( 'NONE', #17061, #44007 ) ;
#51426 = ORIENTED_EDGE ( 'NONE', *, *, #8457, .T. ) ;
#51427 = CARTESIAN_POINT ( 'NONE',  ( -67.46615831890672155, 4.336808689942017736E-15, 6.899827505724789312 ) ) ;
#51428 = ORIENTED_EDGE ( 'NONE', *, *, #27649, .T. ) ;
#51429 = CARTESIAN_POINT ( 'NONE',  ( -11.20636620717317378, 0.000000000000000000, 11.32298014792380414 ) ) ;
#51430 = CARTESIAN_POINT ( 'NONE',  ( -21.04681073720913886, 1.581621852479007106, 4.806765756730587036 ) ) ;
#51431 = ADVANCED_FACE ( 'NONE', ( #42304 ), #11353, .F. ) ;
#51432 = VECTOR ( 'NONE', #22250, 1000.000000000000227 ) ;
#51433 = LINE ( 'NONE', #8251, #28566 ) ;
#51434 = CARTESIAN_POINT ( 'NONE',  ( -18.67697421479882181, -0.1191753592594197858, 4.036397482078229793 ) ) ;
#51435 = EDGE_CURVE ( 'NONE', #31757, #2279, #12493, .T. ) ;
#51436 = DIRECTION ( 'NONE',  ( 0.007781995580012663651, -3.146120232559066537E-19, -0.9999697198139514409 ) ) ;
#51437 = ORIENTED_EDGE ( 'NONE', *, *, #35015, .F. ) ;
#51438 = AXIS2_PLACEMENT_3D ( 'NONE', #33887, #2387, #50649 ) ;
#51439 = VERTEX_POINT ( 'NONE', #29530 ) ;
#51440 = PLANE ( 'NONE',  #30477 ) ;
#51441 = PLANE ( 'NONE',  #26817 ) ;
#51442 = VERTEX_POINT ( 'NONE', #15592 ) ;
#51443 = LINE ( 'NONE', #29859, #5749 ) ;
#51444 = VECTOR ( 'NONE', #32210, 1000.000000000000227 ) ;
#51445 = ORIENTED_EDGE ( 'NONE', *, *, #38865, .F. ) ;
#51446 = EDGE_CURVE ( 'NONE', #37283, #33305, #41713, .T. ) ;
#51447 = DIRECTION ( 'NONE',  ( -0.005961354470445682716, -0.6427876096865404731, 0.7660212471507180654 ) ) ;
#51448 = EDGE_LOOP ( 'NONE', ( #8747, #43361, #47835, #43977, #2612 ) ) ;
#51449 = LINE ( 'NONE', #46600, #53769 ) ;
#51450 = EDGE_CURVE ( 'NONE', #1435, #18921, #3100, .T. ) ;
#51451 = ORIENTED_EDGE ( 'NONE', *, *, #22422, .T. ) ;
#51452 = ORIENTED_EDGE ( 'NONE', *, *, #49905, .T. ) ;
#51454 = ORIENTED_EDGE ( 'NONE', *, *, #46205, .T. ) ;
#51453 = B_SPLINE_CURVE_WITH_KNOTS ( 'NONE', 3,
 ( #23459, #44457, #5560, #27719, #6154, #54114, #2121, #32535, #1840, #19168, #32261, #10936, #44738, #14385, #53539 ),
 .UNSPECIFIED., .F., .F.,
 ( 4, 1, 1, 1, 1, 1, 2, 2, 1, 1, 4 ),
 ( 0.000000000000000000, 0.2700693087945782445, 0.4051039631918675887, 0.4726212903905119833, 0.4895006221901730958, 0.4979402880900037909, 0.4989952463274826555, 0.5000502045649615201, 0.5021601210399194715, 0.5063799539898351521, 0.5401386175891612629 ),
 .UNSPECIFIED. ) ;
#51455 = FACE_OUTER_BOUND ( 'NONE', #36753, .T. ) ;
#51456 = LINE ( 'NONE', #28754, #5129 ) ;
#51457 = DIRECTION ( 'NONE',  ( 0.6427681459581294776, -0.7660444431189769032, 0.005002170337467562802 ) ) ;
#51458 = EDGE_CURVE ( 'NONE', #28952, #9163, #11892, .T. ) ;
#51459 = CARTESIAN_POINT ( 'NONE',  ( -17.93139508144814442, 0.000000000000000000, 13.85596890686001537 ) ) ;
#51460 = ORIENTED_EDGE ( 'NONE', *, *, #50254, .F. ) ;
#51461 = ORIENTED_EDGE ( 'NONE', *, *, #28877, .F. ) ;
#51462 = EDGE_CURVE ( 'NONE', #16114, #33400, #12188, .T. ) ;
#51463 = EDGE_LOOP ( 'NONE', ( #13358, #24240, #1000, #10940 ) ) ;
#51464 = DIRECTION ( 'NONE',  ( 0.9999697198139515519, 0.000000000000000000, 0.007781995580013368816 ) ) ;
#51465 = CARTESIAN_POINT ( 'NONE',  ( -9.381698774953246556, -0.1191753592594195360, 2.840796620997148914 ) ) ;
#51466 = ORIENTED_EDGE ( 'NONE', *, *, #17206, .F. ) ;
#51467 = CARTESIAN_POINT ( 'NONE',  ( -17.42984833845037684, 0.000000000000000000, 9.116748853201215752 ) ) ;
#51468 = VERTEX_POINT ( 'NONE', #33497 ) ;
#51469 = FACE_OUTER_BOUND ( 'NONE', #17636, .T. ) ;
#51470 = LINE ( 'NONE', #55157, #55754 ) ;
#51471 = ORIENTED_EDGE ( 'NONE', *, *, #681, .T. ) ;
#51472 = LINE ( 'NONE', #25606, #36768 ) ;
#51473 = VERTEX_POINT ( 'NONE', #7954 ) ;
#51474 = AXIS2_PLACEMENT_3D ( 'NONE', #5830, #23155, #32236 ) ;
#51475 = CARTESIAN_POINT ( 'NONE',  ( -15.50102849149811135, -0.1191753592594197858, 12.95155240711365430 ) ) ;
#51476 = CARTESIAN_POINT ( 'NONE',  ( -15.91947455447202664, -0.1191753592594193972, 7.012513540498049203 ) ) ;
#51477 = ORIENTED_EDGE ( 'NONE', *, *, #6621, .F. ) ;
#51478 = DIRECTION ( 'NONE',  ( 0.5364919789714477361, 0.6444004775717706579, 0.5449076811759711036 ) ) ;
#51479 = DIRECTION ( 'NONE',  ( -0.6427681459581293666, -0.7660444431189770143, -0.005002170337467561935 ) ) ;
#51480 = DIRECTION ( 'NONE',  ( 0.5449076811759707706, 0.6444004775717708799, -0.5364919789714476250 ) ) ;
#51481 = CARTESIAN_POINT ( 'NONE',  ( -15.03495456790438389, -0.1191753592594197858, 12.77051346725278158 ) ) ;
#51482 = ORIENTED_EDGE ( 'NONE', *, *, #32362, .T. ) ;
#51483 = EDGE_CURVE ( 'NONE', #40757, #4596, #28686, .T. ) ;
#51484 = VECTOR ( 'NONE', #29568, 1000.000000000000000 ) ;
#51485 = CARTESIAN_POINT ( 'NONE',  ( 2.072287782118878319, 0.000000000000000000, -2.950529333540147015 ) ) ;
#51486 = DIRECTION ( 'NONE',  ( 0.9999697198139515519, 0.000000000000000000, 0.007781995580013368816 ) ) ;
#51487 = ADVANCED_FACE ( 'NONE', ( #24677 ), #19868, .F. ) ;
#51488 = DIRECTION ( 'NONE',  ( 0.7660212471507180654, -0.6427876096865404731, 0.005961354470445141482 ) ) ;
#51489 = CARTESIAN_POINT ( 'NONE',  ( -27.06552663992790997, 0.000000000000000000, 7.195101427592543786 ) ) ;
#51490 = CARTESIAN_POINT ( 'NONE',  ( -18.19747506107908563, 0.000000000000000000, 14.03856424583689311 ) ) ;
#51491 = EDGE_CURVE ( 'NONE', #44205, #10708, #24759, .T. ) ;
#51492 = CARTESIAN_POINT ( 'NONE',  ( -7.020097852742797073, 1.644072297827783524, 8.920596959107028212 ) ) ;
#51493 = ORIENTED_EDGE ( 'NONE', *, *, #43113, .T. ) ;
#51494 = LINE ( 'NONE', #12589, #52485 ) ;
#51495 = ADVANCED_FACE ( 'NONE', ( #2802 ), #15892, .F. ) ;
#51496 = CARTESIAN_POINT ( 'NONE',  ( -25.85160216376510434, 17.67350346510513148, -4.606045122360801436 ) ) ;
#51497 = FACE_OUTER_BOUND ( 'NONE', #5104, .T. ) ;
#51498 = EDGE_LOOP ( 'NONE', ( #52085, #39920, #38591 ) ) ;
#51499 = CARTESIAN_POINT ( 'NONE',  ( -31.72782227498118601, 0.000000000000000000, 9.205484770164058972 ) ) ;
#51500 = ORIENTED_EDGE ( 'NONE', *, *, #37786, .F. ) ;
#51501 = ADVANCED_FACE ( 'NONE', ( #43966 ), #4788, .F. ) ;
#51502 = EDGE_CURVE ( 'NONE', #29764, #34537, #9054, .T. ) ;
#51503 = EDGE_CURVE ( 'NONE', #36269, #13086, #55929, .T. ) ;
#51504 = PLANE ( 'NONE',  #37088 ) ;
#51505 = PLANE ( 'NONE',  #49389 ) ;
#51506 = CARTESIAN_POINT ( 'NONE',  ( -31.72626587586518099, 0.000000000000000000, 9.005490826201270949 ) ) ;
#51507 = CARTESIAN_POINT ( 'NONE',  ( -68.57948186459397277, 0.1329774074821103713, 5.304050906517310260 ) ) ;
#51508 = EDGE_LOOP ( 'NONE', ( #30906, #35900, #17410, #38816 ) ) ;
#51509 = ORIENTED_EDGE ( 'NONE', *, *, #45761, .T. ) ;
#51510 = CARTESIAN_POINT ( 'NONE',  ( -69.39314964050831236, -0.6010558250688294857, 7.224037831218162786 ) ) ;
#51511 = PLANE ( 'NONE',  #27764 ) ;
#51512 = CARTESIAN_POINT ( 'NONE',  ( -20.26176469941677993, 0.000000000000000000, 14.76116360616437895 ) ) ;
#51513 = CARTESIAN_POINT ( 'NONE',  ( 5.284365508485809215, -1.088618427183434934, -2.393569053917001810 ) ) ;
#51514 = DIRECTION ( 'NONE',  ( 0.000000000000000000, -0.000000000000000000, -1.000000000000000000 ) ) ;
#51515 = EDGE_CURVE ( 'NONE', #27953, #49693, #51650, .T. ) ;
#51516 = CARTESIAN_POINT ( 'NONE',  ( -15.06642710517098571, 0.000000000000000000, 3.964492566432560761 ) ) ;
#51517 = ORIENTED_EDGE ( 'NONE', *, *, #25697, .F. ) ;
#51518 = LINE ( 'NONE', #25125, #53726 ) ;
#51519 = EDGE_CURVE ( 'NONE', #35036, #48042, #13038, .T. ) ;
#51520 = LINE ( 'NONE', #13712, #24228 ) ;
#51521 = VERTEX_POINT ( 'NONE', #22110 ) ;
#51522 = EDGE_CURVE ( 'NONE', #10313, #3654, #35446, .T. ) ;
#51523 = CARTESIAN_POINT ( 'NONE',  ( -19.60912206198628027, -0.1191753592594197858, 4.398475361799976113 ) ) ;
#51524 = DIRECTION ( 'NONE',  ( 0.007781995580012662783, 0.000000000000000000, -0.9999697198139514409 ) ) ;
#51525 = DIRECTION ( 'NONE',  ( 0.005002170337468016433, -0.7660444431189770143, -0.6427681459581293666 ) ) ;
#51526 = VERTEX_POINT ( 'NONE', #25823 ) ;
#51527 = EDGE_CURVE ( 'NONE', #49950, #13999, #39441, .T. ) ;
#51528 = AXIS2_PLACEMENT_3D ( 'NONE', #32072, #45142, #7544 ) ;
#51529 = LINE ( 'NONE', #34218, #22150 ) ;
#51530 = ORIENTED_EDGE ( 'NONE', *, *, #8122, .F. ) ;
#51531 = ORIENTED_EDGE ( 'NONE', *, *, #23920, .F. ) ;
#51532 = ORIENTED_EDGE ( 'NONE', *, *, #1948, .T. ) ;
#51533 = EDGE_LOOP ( 'NONE', ( #5561, #18494, #1551, #46884 ) ) ;
#51534 = CARTESIAN_POINT ( 'NONE',  ( 2.072287782118878319, 0.000000000000000000, -2.950529333540147015 ) ) ;
#51535 = EDGE_LOOP ( 'NONE', ( #30230, #45169, #5511, #18323 ) ) ;
#51536 = DIRECTION ( 'NONE',  ( 0.005002170337468016433, -0.7660444431189770143, -0.6427681459581293666 ) ) ;
#51537 = VERTEX_POINT ( 'NONE', #43419 ) ;
#51538 = CARTESIAN_POINT ( 'NONE',  ( -17.93139508144814442, 0.000000000000000000, 13.85596890686001537 ) ) ;
#51539 = EDGE_LOOP ( 'NONE', ( #18723, #17351, #50991, #47294 ) ) ;
#51540 = CARTESIAN_POINT ( 'NONE',  ( -13.96170819468429336, 0.000000000000000000, 7.127752359109486235 ) ) ;
#51541 = VERTEX_POINT ( 'NONE', #48513 ) ;
#51542 = DIRECTION ( 'NONE',  ( -0.005961354470445682716, -0.6427876096865404731, 0.7660212471507180654 ) ) ;
#51543 = CARTESIAN_POINT ( 'NONE',  ( -16.63288945721647494, -1.003701604285657911, 3.310076901536455729 ) ) ;
#51544 = FACE_OUTER_BOUND ( 'NONE', #11999, .T. ) ;
#51545 = DIRECTION ( 'NONE',  ( 0.007781995580012662783, 0.000000000000000000, -0.9999697198139514409 ) ) ;
#51546 = CARTESIAN_POINT ( 'NONE',  ( 2.072287782118878319, 0.000000000000000000, -2.950529333540147015 ) ) ;
#51547 = ORIENTED_EDGE ( 'NONE', *, *, #37977, .F. ) ;
#51548 = EDGE_LOOP ( 'NONE', ( #46456, #22106, #15776, #19368 ) ) ;
#51549 = CARTESIAN_POINT ( 'NONE',  ( -21.60330836122860276, -4.079838673713159558, 11.76910067310686081 ) ) ;
#51550 = CARTESIAN_POINT ( 'NONE',  ( -8.372583192005976116, 0.000000000000000000, 5.438704338890580026 ) ) ;
#51551 = DIRECTION ( 'NONE',  ( -0.9999697198139514409, -0.000000000000000000, -0.007781995580013368816 ) ) ;
#51552 = DIRECTION ( 'NONE',  ( -0.005002170337468016433, -0.7660444431189770143, 0.6427681459581293666 ) ) ;
#51553 = DIRECTION ( 'NONE',  ( -0.5364919789714478471, 0.6444004775717705469, -0.5449076811759709926 ) ) ;
#51554 = DIRECTION ( 'NONE',  ( 0.005002170337468016433, -0.7660444431189770143, -0.6427681459581293666 ) ) ;
#51555 = ORIENTED_EDGE ( 'NONE', *, *, #51450, .T. ) ;
#51556 = PLANE ( 'NONE',  #42915 ) ;
#51557 = CARTESIAN_POINT ( 'NONE',  ( -17.83139810946674686, -0.1191753592594197858, 13.85674710641801788 ) ) ;
#51558 = ORIENTED_EDGE ( 'NONE', *, *, #31772, .F. ) ;
#51559 = ADVANCED_FACE ( 'NONE', ( #35197 ), #48209, .F. ) ;
#51560 = EDGE_CURVE ( 'NONE', #16382, #4739, #38888, .T. ) ;
#51561 = VECTOR ( 'NONE', #39564, 1000.000000000000227 ) ;
#51562 = DIRECTION ( 'NONE',  ( -0.6427681459581293666, -0.7660444431189770143, -0.005002170337467561935 ) ) ;
#51563 = CARTESIAN_POINT ( 'NONE',  ( -12.54612273050805271, 0.000000000000000000, 4.353438227646377001 ) ) ;
#51564 = CARTESIAN_POINT ( 'NONE',  ( -22.40478740399063895, 0.000000000000000000, 5.384712028983816623 ) ) ;
#51565 = ADVANCED_FACE ( 'NONE', ( #4517 ), #17029, .F. ) ;
#51566 = CARTESIAN_POINT ( 'NONE',  ( -7.296103114018933411, -3.208161209119383628, 8.210037920513791221 ) ) ;
#51567 = ORIENTED_EDGE ( 'NONE', *, *, #54532, .T. ) ;
#51568 = EDGE_LOOP ( 'NONE', ( #53548, #54417, #40888, #43603 ) ) ;
#51569 = DIRECTION ( 'NONE',  ( 0.9999697198139515519, 0.000000000000000000, 0.007781995580013368816 ) ) ;
#51570 = CARTESIAN_POINT ( 'NONE',  ( -20.46240439165153191, 20.84430116209394868, 4.317727107778031481 ) ) ;
#51571 = LINE ( 'NONE', #35114, #28774 ) ;
#51572 = LINE ( 'NONE', #26282, #45495 ) ;
#51573 = CARTESIAN_POINT ( 'NONE',  ( -12.53750056999220597, 0.000000000000000000, 3.245509117873082605 ) ) ;
#51574 = DIRECTION ( 'NONE',  ( 0.9321478471874540261, 0.000000000000000000, -0.3620778797217457101 ) ) ;
#51575 = CARTESIAN_POINT ( 'NONE',  ( 2.072287782118878319, 0.000000000000000000, -2.950529333540147015 ) ) ;
#51577 = EDGE_CURVE ( 'NONE', #28691, #25884, #56195, .T. ) ;
#51576 = ORIENTED_EDGE ( 'NONE', *, *, #43595, .T. ) ;
#51578 = DIRECTION ( 'NONE',  ( -0.7660212471507179544, -0.6427876096865405842, -0.005961354470445141482 ) ) ;
#51579 = CARTESIAN_POINT ( 'NONE',  ( -16.36043429343423483, -0.6798977022406571535, 3.214577103081905474 ) ) ;
#51580 = ADVANCED_FACE ( 'NONE', ( #22417 ), #39730, .F. ) ;
#51581 = PLANE ( 'NONE',  #11132 ) ;
#51582 = ORIENTED_EDGE ( 'NONE', *, *, #43840, .T. ) ;
#51583 = DIRECTION ( 'NONE',  ( 0.007781995580012663651, 0.000000000000000000, -0.9999697198139515519 ) ) ;
#51584 = ORIENTED_EDGE ( 'NONE', *, *, #27869, .T. ) ;
#51585 = ADVANCED_FACE ( 'NONE', ( #13861 ), #34346, .F. ) ;
#51586 = ORIENTED_EDGE ( 'NONE', *, *, #15880, .T. ) ;
#51587 = EDGE_CURVE ( 'NONE', #53425, #26718, #9632, .T. ) ;
#51588 = ORIENTED_EDGE ( 'NONE', *, *, #36471, .F. ) ;
#51589 = ORIENTED_EDGE ( 'NONE', *, *, #16450, .F. ) ;
#51590 = ORIENTED_EDGE ( 'NONE', *, *, #33491, .F. ) ;
#51591 = VERTEX_POINT ( 'NONE', #21269 ) ;
#51592 = DIRECTION ( 'NONE',  ( 0.007781995580012663651, -3.146120232559066537E-19, -0.9999697198139514409 ) ) ;
#51593 = CARTESIAN_POINT ( 'NONE',  ( -11.83408720182036511, 0.000000000000000000, 6.574971871612978802 ) ) ;
#51594 = CARTESIAN_POINT ( 'NONE',  ( -8.581250235374994872, 0.000000000000000000, 6.551622587568105338 ) ) ;
#51595 = EDGE_LOOP ( 'NONE', ( #41859, #18207, #48296, #9255 ) ) ;
#51596 = DIRECTION ( 'NONE',  ( 0.8531650599175529814, -0.4028455766673920135, -0.3313982828793697877 ) ) ;
#51597 = VERTEX_POINT ( 'NONE', #38601 ) ;
#51598 = CARTESIAN_POINT ( 'NONE',  ( -27.06708303904391144, 0.000000000000000000, 7.395095371555332697 ) ) ;
#51599 = ORIENTED_EDGE ( 'NONE', *, *, #17056, .T. ) ;
#51600 = CARTESIAN_POINT ( 'NONE',  ( 5.454439161952889137, 0.000000000000000000, 2.500037857468615510 ) ) ;
#51601 = LINE ( 'NONE', #12699, #11062 ) ;
#51602 = CARTESIAN_POINT ( 'NONE',  ( -27.56484202182514665, 16.74370688441070953, -4.657437592157546824 ) ) ;
#51603 = ORIENTED_EDGE ( 'NONE', *, *, #52568, .T. ) ;
#51604 = CARTESIAN_POINT ( 'NONE',  ( -12.83169202443629509, 0.000000000000000000, 1.765891372722660169 ) ) ;
#51605 = ORIENTED_EDGE ( 'NONE', *, *, #54254, .F. ) ;
#51606 = FACE_OUTER_BOUND ( 'NONE', #33428, .T. ) ;
#51607 = DIRECTION ( 'NONE',  ( 0.007781995580012662783, 0.000000000000000000, -0.9999697198139514409 ) ) ;
#51608 = CARTESIAN_POINT ( 'NONE',  ( -11.13054826722768098, 24.50000000000005684, 3.000000000000000444 ) ) ;
#51609 = DIRECTION ( 'NONE',  ( 0.000000000000000000, -1.000000000000000000, 0.000000000000000000 ) ) ;
#51610 = CARTESIAN_POINT ( 'NONE',  ( -17.93139508144814442, 0.000000000000000000, 13.85596890686001537 ) ) ;
#51611 = DIRECTION ( 'NONE',  ( 0.007781995580012663651, 0.000000000000000000, -0.9999697198139515519 ) ) ;
#51612 = DIRECTION ( 'NONE',  ( 0.005002170337468016433, -0.7660444431189770143, -0.6427681459581293666 ) ) ;
#51613 = DIRECTION ( 'NONE',  ( 0.000000000000000000, -0.000000000000000000, -1.000000000000000000 ) ) ;
#51614 = EDGE_LOOP ( 'NONE', ( #51724, #27343, #19307, #29414 ) ) ;
#51615 = CARTESIAN_POINT ( 'NONE',  ( -11.15089438559551205, 0.000000000000000000, 4.194970203655428165 ) ) ;
#51616 = ORIENTED_EDGE ( 'NONE', *, *, #52141, .F. ) ;
#51617 = ADVANCED_FACE ( 'NONE', ( #12753 ), #30071, .F. ) ;
#51618 = CARTESIAN_POINT ( 'NONE',  ( -20.54126990917373519, -0.1191753592594197858, 4.760553241521720658 ) ) ;
#51619 = FACE_OUTER_BOUND ( 'NONE', #12489, .T. ) ;
#51620 = CARTESIAN_POINT ( 'NONE',  ( -8.168214455200342172, -0.1191753592594182315, 5.964839429474373844 ) ) ;
#51621 = CARTESIAN_POINT ( 'NONE',  ( -25.20278734466900517, 0.000000000000000000, 6.670939612111840944 ) ) ;
#51622 = CARTESIAN_POINT ( 'NONE',  ( -9.289472744725888020, 0.000000000000000000, 3.840124147469701654 ) ) ;
#51623 = EDGE_CURVE ( 'NONE', #12635, #49710, #36871, .T. ) ;
#51624 = EDGE_CURVE ( 'NONE', #41029, #17901, #32332, .T. ) ;
#51625 = DIRECTION ( 'NONE',  ( 0.000000000000000000, 1.000000000000000000, -0.000000000000000000 ) ) ;
#51626 = APPLICATION_PROTOCOL_DEFINITION ( 'draft international standard', 'automotive_design', 1998, #56163 ) ;
#51627 = ORIENTED_EDGE ( 'NONE', *, *, #44705, .F. ) ;
#51628 = DIRECTION ( 'NONE',  ( -0.7660212471507179544, -0.6427876096865405842, -0.005961354470445141482 ) ) ;
#51629 = FACE_OUTER_BOUND ( 'NONE', #17038, .T. ) ;
#51630 = PLANE ( 'NONE',  #43622 ) ;
#51631 = DIRECTION ( 'NONE',  ( -0.7660212471507179544, -0.6427876096865405842, -0.005961354470445141482 ) ) ;
#51632 = CARTESIAN_POINT ( 'NONE',  ( -8.609916609573598834, 0.000000000000000000, 10.23519010964256637 ) ) ;
#51633 = CARTESIAN_POINT ( 'NONE',  ( -15.80301146101693455, 0.000000000000000000, 4.897430492490863152 ) ) ;
#51634 = CARTESIAN_POINT ( 'NONE',  ( 3.520599301005862269, -1.000000000000000000, 0.7780620552096689790 ) ) ;
#51635 = ORIENTED_EDGE ( 'NONE', *, *, #39320, .T. ) ;
#51636 = CARTESIAN_POINT ( 'NONE',  ( -17.75702712210175349, -0.1134144341941959455, 3.679058789739912072 ) ) ;
#51637 = FACE_OUTER_BOUND ( 'NONE', #9789, .T. ) ;
#51638 = ORIENTED_EDGE ( 'NONE', *, *, #376, .T. ) ;
#51639 = ORIENTED_EDGE ( 'NONE', *, *, #46328, .F. ) ;
#51640 = PLANE ( 'NONE',  #50085 ) ;
#51641 = ORIENTED_EDGE ( 'NONE', *, *, #46174, .T. ) ;
#51642 = EDGE_CURVE ( 'NONE', #47757, #41032, #19527, .T. ) ;
#51643 = EDGE_LOOP ( 'NONE', ( #9800, #52776, #27608, #41962 ) ) ;
#51644 = ORIENTED_EDGE ( 'NONE', *, *, #54314, .F. ) ;
#51645 = ORIENTED_EDGE ( 'NONE', *, *, #33878, .T. ) ;
#51646 = ADVANCED_FACE ( 'NONE', ( #32031 ), #35740, .F. ) ;
#51647 = B_SPLINE_CURVE_WITH_KNOTS ( 'NONE', 3,
 ( #30513, #9181, #29931, #13461 ),
 .UNSPECIFIED., .F., .F.,
 ( 4, 4 ),
 ( 0.0009679422276756773124, 0.001611251064783924929 ),
 .UNSPECIFIED. ) ;
#51648 = DIRECTION ( 'NONE',  ( 0.005961354470445682716, -0.6427876096865404731, -0.7660212471507180654 ) ) ;
#51649 = ORIENTED_EDGE ( 'NONE', *, *, #45937, .T. ) ;
#51650 = LINE ( 'NONE', #26111, #44155 ) ;
#51651 = CARTESIAN_POINT ( 'NONE',  ( 2.602374448188125350E-16, 2.000000000000000000, 2.125000000000000000 ) ) ;
#51652 = ORIENTED_EDGE ( 'NONE', *, *, #32818, .F. ) ;
#51653 = EDGE_CURVE ( 'NONE', #44974, #54122, #19233, .T. ) ;
#51654 = ORIENTED_EDGE ( 'NONE', *, *, #24138, .F. ) ;
#51655 = LINE ( 'NONE', #39736, #53757 ) ;
#51656 = VERTEX_POINT ( 'NONE', #27209 ) ;
#51657 = CARTESIAN_POINT ( 'NONE',  ( -27.99923088623136636, 0.000000000000000000, 7.757173251277078130 ) ) ;
#51658 = LINE ( 'NONE', #33773, #49454 ) ;
#51659 = ORIENTED_EDGE ( 'NONE', *, *, #16189, .F. ) ;
#51660 = CARTESIAN_POINT ( 'NONE',  ( -18.89555915323239077, 4.010151117816511679, 3.893663786391856618 ) ) ;
#51661 = ORIENTED_EDGE ( 'NONE', *, *, #17886, .T. ) ;
#51662 = LINE ( 'NONE', #30088, #54529 ) ;
#51663 = ADVANCED_FACE ( 'NONE', ( #36291 ), #23771, .F. ) ;
#51664 = CARTESIAN_POINT ( 'NONE',  ( 5.558065690504402134, 8.867811663421879681E-06, -2.260478214935544017 ) ) ;
#51665 = ORIENTED_EDGE ( 'NONE', *, *, #35117, .T. ) ;
#51666 = FACE_OUTER_BOUND ( 'NONE', #46927, .T. ) ;
#51667 = LINE ( 'NONE', #4534, #31097 ) ;
#51668 = CARTESIAN_POINT ( 'NONE',  ( -61.38973930853472183, 7.404220597074748333, 2.999999999999993339 ) ) ;
#51669 = LINE ( 'NONE', #13359, #44654 ) ;
#51670 = EDGE_CURVE ( 'NONE', #25200, #866, #6210, .T. ) ;
#51671 = ORIENTED_EDGE ( 'NONE', *, *, #39050, .T. ) ;
#51672 = EDGE_CURVE ( 'NONE', #31703, #25139, #10466, .T. ) ;
#51673 = LINE ( 'NONE', #56215, #51874 ) ;
#51674 = DIRECTION ( 'NONE',  ( 0.7660212471507180654, -0.6427876096865404731, 0.005961354470445141482 ) ) ;
#51675 = DIRECTION ( 'NONE',  ( -0.5449076811759708816, 0.6444004775717707689, 0.5364919789714475140 ) ) ;
#51676 = CARTESIAN_POINT ( 'NONE',  ( -14.30946433947862495, -4.889348428825665671, 2.283607204660580869 ) ) ;
#51677 = PLANE ( 'NONE',  #15954 ) ;
#51678 = CARTESIAN_POINT ( 'NONE',  ( -17.22278863308774532, 0.000000000000000000, 8.210370086506713960 ) ) ;
#51679 = EDGE_CURVE ( 'NONE', #54483, #41210, #2191, .T. ) ;
#51680 = CARTESIAN_POINT ( 'NONE',  ( -10.47421230394850866, 0.000000000000000000, 10.95934586908605723 ) ) ;
#51681 = CARTESIAN_POINT ( 'NONE',  ( -24.26908309836554878, 0.000000000000000000, 6.108867788427308376 ) ) ;
#51682 = LINE ( 'NONE', #21860, #6845 ) ;
#51683 = ORIENTED_EDGE ( 'NONE', *, *, #2244, .F. ) ;
#51684 = CARTESIAN_POINT ( 'NONE',  ( -0.8459003381547196554, -5.709362246987525147, 3.546949993899496167 ) ) ;
#51685 = ORIENTED_EDGE ( 'NONE', *, *, #43834, .F. ) ;
#51686 = DIRECTION ( 'NONE',  ( 0.007781995580012663651, -3.146120232559066537E-19, -0.9999697198139514409 ) ) ;
#51687 = LINE ( 'NONE', #33277, #42647 ) ;
#51688 = CARTESIAN_POINT ( 'NONE',  ( -23.33771345073609638, -0.1191753592594197858, 5.846786880686956955 ) ) ;
#51689 = CARTESIAN_POINT ( 'NONE',  ( -18.22153117760466401, 2.067327705546506245, 7.352019596133413160 ) ) ;
#51690 = CARTESIAN_POINT ( 'NONE',  ( -17.46532115785441519, 0.000000000000000000, 13.67492996699914265 ) ) ;
#51691 = EDGE_CURVE ( 'NONE', #39994, #18681, #14442, .T. ) ;
#51692 = ORIENTED_EDGE ( 'NONE', *, *, #25017, .T. ) ;
#51693 = AXIS2_PLACEMENT_3D ( 'NONE', #41124, #19547, #19825 ) ;
#51694 = VERTEX_POINT ( 'NONE', #10993 ) ;
#51695 = DIRECTION ( 'NONE',  ( -0.005961354470445682716, -0.6427876096865404731, 0.7660212471507180654 ) ) ;
#51696 = PLANE ( 'NONE',  #45862 ) ;
#51697 = VERTEX_POINT ( 'NONE', #32589 ) ;
#51698 = PLANE ( 'NONE',  #3952 ) ;
#51699 = ORIENTED_EDGE ( 'NONE', *, *, #7502, .T. ) ;
#51700 = DIRECTION ( 'NONE',  ( -0.6427681459581293666, -0.7660444431189770143, -0.005002170337467561935 ) ) ;
#51701 = EDGE_LOOP ( 'NONE', ( #49714, #15916, #8317, #105 ) ) ;
#51702 = CARTESIAN_POINT ( 'NONE',  ( -16.79925329029790149, 0.000000000000000000, 13.49544742625427496 ) ) ;
#51703 = VERTEX_POINT ( 'NONE', #44263 ) ;
#51704 = ORIENTED_EDGE ( 'NONE', *, *, #33697, .F. ) ;
#51705 = ORIENTED_EDGE ( 'NONE', *, *, #8239, .T. ) ;
#51706 = LINE ( 'NONE', #30435, #32949 ) ;
#51707 = FACE_OUTER_BOUND ( 'NONE', #30635, .T. ) ;
#51708 = LINE ( 'NONE', #12816, #33920 ) ;
#51709 = LINE ( 'NONE', #55406, #49347 ) ;
#51710 = VERTEX_POINT ( 'NONE', #5366 ) ;
#51711 = ADVANCED_FACE ( 'NONE', ( #22671 ), #18400, .F. ) ;
#51712 = VERTEX_POINT ( 'NONE', #39981 ) ;
#51714 = ADVANCED_FACE ( 'NONE', ( #18709 ), #1365, .F. ) ;
#51713 = ORIENTED_EDGE ( 'NONE', *, *, #30691, .T. ) ;
#51715 = DIRECTION ( 'NONE',  ( 0.000000000000000000, -1.000000000000000000, 0.000000000000000000 ) ) ;
#51716 = ORIENTED_EDGE ( 'NONE', *, *, #26995, .F. ) ;
#51717 = FACE_OUTER_BOUND ( 'NONE', #26225, .T. ) ;
#51718 = ORIENTED_EDGE ( 'NONE', *, *, #33597, .F. ) ;
#51719 = CARTESIAN_POINT ( 'NONE',  ( -22.40634380310664397, 0.000000000000000000, 5.584705972946605534 ) ) ;
#51720 = DIRECTION ( 'NONE',  ( -0.005002170337468016433, -0.7660444431189770143, 0.6427681459581293666 ) ) ;
#51721 = EDGE_CURVE ( 'NONE', #10587, #15428, #31440, .T. ) ;
#51722 = ORIENTED_EDGE ( 'NONE', *, *, #31222, .F. ) ;
#51723 = LINE ( 'NONE', #13122, #29510 ) ;
#51724 = ORIENTED_EDGE ( 'NONE', *, *, #15337, .F. ) ;
#51725 = EDGE_CURVE ( 'NONE', #28729, #43960, #14707, .T. ) ;
#51726 = EDGE_CURVE ( 'NONE', #18328, #44507, #40829, .T. ) ;
#51727 = VECTOR ( 'NONE', #55972, 999.9999999999998863 ) ;
#51728 = LINE ( 'NONE', #33, #46406 ) ;
#51729 = PLANE ( 'NONE',  #9421 ) ;
#51730 = ORIENTED_EDGE ( 'NONE', *, *, #42005, .T. ) ;
#51731 = DIRECTION ( 'NONE',  ( 0.9321478471874540261, 0.000000000000000000, -0.3620778797217456546 ) ) ;
#51732 = CARTESIAN_POINT ( 'NONE',  ( -15.55118237654904867, 0.000000000000000000, 6.546044577468901338 ) ) ;
#51733 = PLANE ( 'NONE',  #2844 ) ;
#51734 = ADVANCED_FACE ( 'NONE', ( #1902 ), #48804, .F. ) ;
#51735 = VERTEX_POINT ( 'NONE', #54708 ) ;
#51736 = DIRECTION ( 'NONE',  ( 0.000000000000000000, -0.000000000000000000, -1.000000000000000000 ) ) ;
#51737 = EDGE_CURVE ( 'NONE', #14093, #54725, #15813, .T. ) ;
#51738 = DIRECTION ( 'NONE',  ( 0.5449076811759707706, 0.6444004775717708799, -0.5364919789714476250 ) ) ;
#51739 = CARTESIAN_POINT ( 'NONE',  ( -16.81345671998191449, 0.000000000000000000, 3.412238694616132495 ) ) ;
#51740 = DIRECTION ( 'NONE',  ( -0.6427681459581293666, -0.7660444431189770143, -0.005002170337467561935 ) ) ;
#51741 = CARTESIAN_POINT ( 'NONE',  ( -11.40636015113596180, 0.000000000000000000, 11.32142374880780089 ) ) ;
#51742 = EDGE_CURVE ( 'NONE', #20189, #35085, #33990, .T. ) ;
#51743 = PLANE ( 'NONE',  #53323 ) ;
#51744 = DIRECTION ( 'NONE',  ( 0.9335804264972041855, -0.3583679495452941066, 0.000000000000000000 ) ) ;
#51745 = VERTEX_POINT ( 'NONE', #46188 ) ;
#51746 = FACE_OUTER_BOUND ( 'NONE', #41550, .T. ) ;
#51747 = DIRECTION ( 'NONE',  ( -0.005002170337468016433, -0.7660444431189770143, 0.6427681459581293666 ) ) ;
#51748 = FACE_OUTER_BOUND ( 'NONE', #17342, .T. ) ;
#51749 = ORIENTED_EDGE ( 'NONE', *, *, #21590, .T. ) ;
#51750 = LINE ( 'NONE', #12861, #47423 ) ;
#51751 = CARTESIAN_POINT ( 'NONE',  ( -12.23851102634202448, -0.1191753592594197858, 11.68427982808754884 ) ) ;
#51752 = EDGE_LOOP ( 'NONE', ( #10743, #53157, #31898, #45458 ) ) ;
#51753 = ADVANCED_FACE ( 'NONE', ( #19804 ), #3335, .F. ) ;
#51754 = DIRECTION ( 'NONE',  ( 0.5449076811759707706, 0.6444004775717708799, -0.5364919789714476250 ) ) ;
#51755 = LINE ( 'NONE', #3771, #34888 ) ;
#51756 = AXIS2_PLACEMENT_3D ( 'NONE', #6733, #24331, #50155 ) ;
#51757 = DIRECTION ( 'NONE',  ( -0.6427681459581293666, -0.7660444431189770143, -0.005002170337467561935 ) ) ;
#51758 = CARTESIAN_POINT ( 'NONE',  ( -67.62757635072813400, 0.1329464987405940268, -2.709928232736921405 ) ) ;
#51759 = EDGE_CURVE ( 'NONE', #12964, #41663, #28892, .T. ) ;
#51760 = ORIENTED_EDGE ( 'NONE', *, *, #5992, .F. ) ;
#51761 = ORIENTED_EDGE ( 'NONE', *, *, #890, .F. ) ;
#51762 = DIRECTION ( 'NONE',  ( -0.9999697198139514409, -0.000000000000000000, -0.007781995580013368816 ) ) ;
#51763 = LINE ( 'NONE', #8327, #44935 ) ;
#51764 = PLANE ( 'NONE',  #10591 ) ;
#51765 = DIRECTION ( 'NONE',  ( 0.000000000000000000, -1.000000000000000000, 0.000000000000000000 ) ) ;
#51766 = DIRECTION ( 'NONE',  ( -0.9999697198139514409, -0.000000000000000000, -0.007781995580013368816 ) ) ;
#51767 = VECTOR ( 'NONE', #3420, 1000.000000000000114 ) ;
#51768 = DIRECTION ( 'NONE',  ( 0.5449076811759707706, 0.6444004775717708799, -0.5364919789714476250 ) ) ;
#51769 = ORIENTED_EDGE ( 'NONE', *, *, #54953, .T. ) ;
#51770 = FACE_OUTER_BOUND ( 'NONE', #13090, .T. ) ;
#51771 = CIRCLE ( 'NONE', #27289, 3.000000000000001332 ) ;
#51772 = LINE ( 'NONE', #4641, #31497 ) ;
#51773 = ORIENTED_EDGE ( 'NONE', *, *, #36396, .T. ) ;
#51774 = DIRECTION ( 'NONE',  ( -0.005961354470445682716, -0.6427876096865404731, 0.7660212471507180654 ) ) ;
#51775 = DIRECTION ( 'NONE',  ( -0.6246952433987894571, 0.7422098413412802076, 0.2426528472758539834 ) ) ;
#51776 = CARTESIAN_POINT ( 'NONE',  ( -14.01545677930355183, 0.000000000000000000, 2.126011111488108174 ) ) ;
#51777 = ORIENTED_EDGE ( 'NONE', *, *, #53262, .F. ) ;
#51778 = DIRECTION ( 'NONE',  ( 0.5449076811759707706, 0.6444004775717708799, -0.5364919789714476250 ) ) ;
#51779 = EDGE_CURVE ( 'NONE', #46331, #14535, #33692, .T. ) ;
#51780 = VERTEX_POINT ( 'NONE', #41920 ) ;
#51781 = VERTEX_POINT ( 'NONE', #29450 ) ;
#51782 = EDGE_LOOP ( 'NONE', ( #6056, #35302, #1652, #24612 ) ) ;
#51783 = ORIENTED_EDGE ( 'NONE', *, *, #30731, .F. ) ;
#51784 = DIRECTION ( 'NONE',  ( 0.000000000000000000, -0.000000000000000000, -1.000000000000000000 ) ) ;
#51786 = ADVANCED_FACE ( 'NONE', ( #25205 ), #38232, .F. ) ;
#51785 = ORIENTED_EDGE ( 'NONE', *, *, #26310, .F. ) ;
#51787 = CARTESIAN_POINT ( 'NONE',  ( -15.66898763994628574, 2.391131607591508335, 2.692009034675617141 ) ) ;
#51788 = EDGE_CURVE ( 'NONE', #45853, #1428, #45934, .T. ) ;
#51789 = VECTOR ( 'NONE', #28094, 1000.000000000000227 ) ;
#51790 = AXIS2_PLACEMENT_3D ( 'NONE', #32347, #49662, #10757 ) ;
#51791 = ORIENTED_EDGE ( 'NONE', *, *, #48987, .F. ) ;
#51792 = LINE ( 'NONE', #4401, #16853 ) ;
#51793 = EDGE_LOOP ( 'NONE', ( #55781, #39686, #17062, #9401 ) ) ;
#51794 = CARTESIAN_POINT ( 'NONE',  ( -12.60458797795435615, 0.000000000000000000, 11.86609696750642229 ) ) ;
#51795 = ORIENTED_EDGE ( 'NONE', *, *, #4274, .F. ) ;
#51796 = EDGE_CURVE ( 'NONE', #7109, #50616, #16111, .T. ) ;
#51797 = DIRECTION ( 'NONE',  ( 0.9999697198139515519, 0.000000000000000000, 0.007781995580013368816 ) ) ;
#51798 = CARTESIAN_POINT ( 'NONE',  ( -12.30159815216673458, 0.000000000000000000, 6.940665663102732807 ) ) ;
#51799 = PLANE ( 'NONE',  #37651 ) ;
#51800 = DIRECTION ( 'NONE',  ( -0.9999697198139514409, -0.000000000000000000, -0.007781995580013368816 ) ) ;
#51801 = DIRECTION ( 'NONE',  ( -0.6427681459581293666, -0.7660444431189770143, -0.005002170337467561935 ) ) ;
#51802 = ORIENTED_EDGE ( 'NONE', *, *, #18938, .F. ) ;
#51803 = ORIENTED_EDGE ( 'NONE', *, *, #23851, .T. ) ;
#51804 = EDGE_CURVE ( 'NONE', #37629, #23769, #46457, .T. ) ;
#51805 = CARTESIAN_POINT ( 'NONE',  ( -7.222176269732285547, -2.744276736922906856, 8.400358159916756051 ) ) ;
#51806 = CARTESIAN_POINT ( 'NONE',  ( -16.38607150127187140, 1.581621852479007106, 2.996376358121860761 ) ) ;
#51807 = VECTOR ( 'NONE', #43160, 1000.000000000000227 ) ;
#51808 = EDGE_CURVE ( 'NONE', #17431, #27972, #55552, .T. ) ;
#51809 = CYLINDRICAL_SURFACE ( 'NONE', #7026, 2.000000000000001332 ) ;
#51810 = CARTESIAN_POINT ( 'NONE',  ( -13.97164800958942266, 0.000000000000000000, 8.404997228177755630 ) ) ;
#51811 = EDGE_CURVE ( 'NONE', #33148, #223, #12115, .T. ) ;
#51812 = DIRECTION ( 'NONE',  ( 0.9999697198139515519, 0.000000000000000000, 0.007781995580013368816 ) ) ;
#51813 = LINE ( 'NONE', #38483, #47697 ) ;
#51814 = ORIENTED_EDGE ( 'NONE', *, *, #55945, .T. ) ;
#51815 = CARTESIAN_POINT ( 'NONE',  ( -17.98066455030807376, -5.375054281893166142, 3.694129481368514600 ) ) ;
#51816 = DIRECTION ( 'NONE',  ( -0.9999697198139514409, -0.000000000000000000, -0.007781995580013368816 ) ) ;
#51817 = VERTEX_POINT ( 'NONE', #20908 ) ;
#51818 = EDGE_CURVE ( 'NONE', #31643, #46025, #20655, .T. ) ;
#51819 = CARTESIAN_POINT ( 'NONE',  ( -13.64380565324295524, -2.946525016555660237, 6.817398727822249427 ) ) ;
#51820 = DIRECTION ( 'NONE',  ( 0.000000000000000000, 0.000000000000000000, -1.000000000000000000 ) ) ;
#51821 = CARTESIAN_POINT ( 'NONE',  ( -56.75000000000000711, 4.550000000000001599, -2.749999999999994671 ) ) ;
#51822 = LINE ( 'NONE', #51566, #20514 ) ;
#51823 = VERTEX_POINT ( 'NONE', #51316 ) ;
#51824 = ORIENTED_EDGE ( 'NONE', *, *, #3192, .F. ) ;
#51825 = DIRECTION ( 'NONE',  ( 0.005961354470445682716, -0.6427876096865404731, -0.7660212471507180654 ) ) ;
#51826 = DIRECTION ( 'NONE',  ( -0.5364919789714478471, 0.6444004775717705469, -0.5449076811759709926 ) ) ;
#51827 = DIRECTION ( 'NONE',  ( 0.007781995580012663651, -3.146120232559066537E-19, -0.9999697198139514409 ) ) ;
#51828 = VECTOR ( 'NONE', #27698, 999.9999999999998863 ) ;
#51829 = AXIS2_PLACEMENT_3D ( 'NONE', #42398, #29632, #50885 ) ;
#51830 = CARTESIAN_POINT ( 'NONE',  ( -27.99923088623136636, 0.000000000000000000, 7.757173251277078130 ) ) ;
#51831 = DIRECTION ( 'NONE',  ( 0.5364919789714477361, 0.6444004775717706579, 0.5449076811759711036 ) ) ;
#51832 = DIRECTION ( 'NONE',  ( -0.3620778797217457101, 0.000000000000000000, -0.9321478471874540261 ) ) ;
#51833 = CARTESIAN_POINT ( 'NONE',  ( -12.75776174254319173, 3.362543313726510164, 1.530196911152285733 ) ) ;
#51834 = ORIENTED_EDGE ( 'NONE', *, *, #37481, .T. ) ;
#51835 = DIRECTION ( 'NONE',  ( 0.6427681459581294776, -0.7660444431189769032, 0.005002170337467562802 ) ) ;
#51836 = DIRECTION ( 'NONE',  ( 0.007781995580012663651, 0.000000000000000000, -0.9999697198139515519 ) ) ;
#51837 = AXIS2_PLACEMENT_3D ( 'NONE', #29737, #42209, #34521 ) ;
#51838 = ORIENTED_EDGE ( 'NONE', *, *, #49755, .F. ) ;
#51839 = CARTESIAN_POINT ( 'NONE',  ( -18.39746900504187010, 0.000000000000000000, 14.03700784672088808 ) ) ;
#51840 = VERTEX_POINT ( 'NONE', #50475 ) ;
#51841 = PLANE ( 'NONE',  #49462 ) ;
#51842 = EDGE_CURVE ( 'NONE', #30962, #43904, #37971, .T. ) ;
#51843 = ORIENTED_EDGE ( 'NONE', *, *, #52886, .T. ) ;
#51844 = ADVANCED_FACE ( 'NONE', ( #11575 ), #24603, .F. ) ;
#51845 = EDGE_LOOP ( 'NONE', ( #42895, #17387, #56075, #20059 ) ) ;
#51846 = VECTOR ( 'NONE', #15681, 999.9999999999998863 ) ;
#51847 = ORIENTED_EDGE ( 'NONE', *, *, #49932, .T. ) ;
#51848 = VERTEX_POINT ( 'NONE', #3024 ) ;
#51849 = ORIENTED_EDGE ( 'NONE', *, *, #46538, .F. ) ;
#51850 = EDGE_LOOP ( 'NONE', ( #54073, #47683, #3598, #34672 ) ) ;
#51851 = CARTESIAN_POINT ( 'NONE',  ( -16.58663476131414427, 5.143464774974012776, 2.960640501956672832 ) ) ;
#51852 = LINE ( 'NONE', #21507, #48313 ) ;
#51853 = DIRECTION ( 'NONE',  ( 0.000000000000000000, -1.000000000000000000, 0.000000000000000000 ) ) ;
#51854 = EDGE_CURVE ( 'NONE', #53756, #1256, #7043, .T. ) ;
#51855 = ADVANCED_FACE ( 'NONE', ( #41648 ), #37126, .F. ) ;
#51856 = EDGE_CURVE ( 'NONE', #873, #4449, #40432, .T. ) ;
#51857 = ORIENTED_EDGE ( 'NONE', *, *, #10376, .T. ) ;
#51858 = DIRECTION ( 'NONE',  ( 0.000000000000000000, -0.000000000000000000, -1.000000000000000000 ) ) ;
#51859 = ORIENTED_EDGE ( 'NONE', *, *, #35167, .F. ) ;
#51860 = LINE ( 'NONE', #27647, #35885 ) ;
#51861 = EDGE_CURVE ( 'NONE', #24462, #14078, #25750, .T. ) ;
#51862 = ORIENTED_EDGE ( 'NONE', *, *, #37301, .T. ) ;
#51863 = LINE ( 'NONE', #43623, #37418 ) ;
#51864 = CARTESIAN_POINT ( 'NONE',  ( 5.446213544912834159, -1.070058632457644654, 0.6896135826588392082 ) ) ;
#51865 = ORIENTED_EDGE ( 'NONE', *, *, #15202, .T. ) ;
#51866 = CARTESIAN_POINT ( 'NONE',  ( -16.81267852042391198, -0.1191753592594197858, 3.312241722634738039 ) ) ;
#51867 = VERTEX_POINT ( 'NONE', #21768 ) ;
#51868 = VECTOR ( 'NONE', #21692, 999.9999999999998863 ) ;
#51869 = VECTOR ( 'NONE', #18148, 1000.000000000000227 ) ;
#51870 = LINE ( 'NONE', #29471, #46344 ) ;
#51871 = CARTESIAN_POINT ( 'NONE',  ( -21.47263955680318404, 0.000000000000000000, 5.022634149262071190 ) ) ;
#51872 = EDGE_CURVE ( 'NONE', #32655, #4253, #47898, .T. ) ;
#51873 = DIRECTION ( 'NONE',  ( 0.5364919789714477361, 0.6444004775717706579, 0.5449076811759711036 ) ) ;
#51874 = VECTOR ( 'NONE', #25551, 1000.000000000000227 ) ;
#51875 = DIRECTION ( 'NONE',  ( 0.9999697198139515519, 0.000000000000000000, 0.007781995580013368816 ) ) ;
#51876 = CARTESIAN_POINT ( 'NONE',  ( -20.54049170961573267, 0.000000000000000000, 4.660556269540326646 ) ) ;
#51877 = CARTESIAN_POINT ( 'NONE',  ( -56.38001980572109062, 4.410024460692103077, -3.000000000000007105 ) ) ;
#51878 = EDGE_CURVE ( 'NONE', #11293, #24035, #38824, .T. ) ;
#51879 = LINE ( 'NONE', #12996, #46583 ) ;
#51880 = CARTESIAN_POINT ( 'NONE',  ( -69.94833770632727976, -8.709315162003530730, 7.852029984319920608 ) ) ;
#51881 = ORIENTED_EDGE ( 'NONE', *, *, #681, .F. ) ;
#51882 = FACE_OUTER_BOUND ( 'NONE', #25331, .T. ) ;
#51883 = EDGE_CURVE ( 'NONE', #18261, #187, #26303, .T. ) ;
#51884 = FACE_OUTER_BOUND ( 'NONE', #14267, .T. ) ;
#51885 = CARTESIAN_POINT ( 'NONE',  ( -12.33850799832341849, 0.000000000000000000, 11.68350162852954632 ) ) ;
#51886 = LINE ( 'NONE', #43110, #4561 ) ;
#51887 = AXIS2_PLACEMENT_3D ( 'NONE', #29468, #16676, #42525 ) ;
#51888 = DIRECTION ( 'NONE',  ( -0.5364919789714478471, 0.6444004775717705469, -0.5449076811759709926 ) ) ;
#51889 = CARTESIAN_POINT ( 'NONE',  ( -8.374569218570126594, 0.000000000000000000, 5.693904487294544126 ) ) ;
#51890 = EDGE_CURVE ( 'NONE', #23769, #42201, #159, .T. ) ;
#51891 = CARTESIAN_POINT ( 'NONE',  ( 2.072287782118878319, 0.000000000000000000, -2.950529333540147015 ) ) ;
#51892 = DIRECTION ( 'NONE',  ( -0.9321478471874540261, 0.000000000000000000, 0.3620778797217457656 ) ) ;
#51893 = APPLICATION_PROTOCOL_DEFINITION ( 'draft international standard', 'automotive_design', 1998, #46339 ) ;
#51894 = ORIENTED_EDGE ( 'NONE', *, *, #9853, .T. ) ;
#51895 = CARTESIAN_POINT ( 'NONE',  ( -16.48620427724178938, 0.000000000000000000, 7.277432160448412013 ) ) ;
#51896 = FACE_OUTER_BOUND ( 'NONE', #53720, .T. ) ;
#51897 = CARTESIAN_POINT ( 'NONE',  ( -20.54049170961573267, 0.000000000000000000, 4.660556269540326646 ) ) ;
#51898 = DIRECTION ( 'NONE',  ( 0.000000000000000000, -0.000000000000000000, -1.000000000000000000 ) ) ;
#51899 = FACE_OUTER_BOUND ( 'NONE', #16141, .T. ) ;
#51900 = VECTOR ( 'NONE', #40747, 999.9999999999998863 ) ;
#51901 = DIRECTION ( 'NONE',  ( 0.6427681459581294776, -0.7660444431189769032, 0.005002170337467562802 ) ) ;
#51902 = CARTESIAN_POINT ( 'NONE',  ( -22.07366256627002699, 3.848249166794009746, 11.77111376987874358 ) ) ;
#51903 = CARTESIAN_POINT ( 'NONE',  ( -10.03886374922923075, -0.1191753592594202438, 1.148964696635692562 ) ) ;
#51904 = CARTESIAN_POINT ( 'NONE',  ( -68.92522653842155478, -9.732315607823066372, 6.824617610603313622 ) ) ;
#51905 = AXIS2_PLACEMENT_3D ( 'NONE', #10855, #19364, #14559 ) ;
#51906 = ORIENTED_EDGE ( 'NONE', *, *, #26090, .F. ) ;
#51907 = LINE ( 'NONE', #56188, #36481 ) ;
#51908 = VECTOR ( 'NONE', #35435, 1000.000000000000227 ) ;
#51909 = AXIS2_PLACEMENT_3D ( 'NONE', #11601, #55301, #20088 ) ;
#51910 = VERTEX_POINT ( 'NONE', #56133 ) ;
#51911 = AXIS2_PLACEMENT_3D ( 'NONE', #12680, #4448, #8720 ) ;
#51912 = EDGE_LOOP ( 'NONE', ( #12799, #36942, #27204, #10935 ) ) ;
#51913 = ORIENTED_EDGE ( 'NONE', *, *, #37432, .F. ) ;
#51914 = VECTOR ( 'NONE', #56164, 1000.000000000000227 ) ;
#51915 = ORIENTED_EDGE ( 'NONE', *, *, #28331, .F. ) ;
#51916 = ORIENTED_EDGE ( 'NONE', *, *, #719, .F. ) ;
#51917 = CARTESIAN_POINT ( 'NONE',  ( -11.30636317915456779, -0.1191753592594197858, 11.32220194836580340 ) ) ;
#51918 = CARTESIAN_POINT ( 'NONE',  ( -13.08408713167409942, -0.1191753592594197858, 1.863930203747758085 ) ) ;
#51919 = EDGE_CURVE ( 'NONE', #46599, #9606, #30597, .T. ) ;
#51920 = EDGE_CURVE ( 'NONE', #15779, #49029, #43364, .T. ) ;
#51921 = EDGE_LOOP ( 'NONE', ( #2513, #23247, #3810, #19353 ) ) ;
#51922 = VECTOR ( 'NONE', #9209, 999.9999999999998863 ) ;
#51923 = EDGE_CURVE ( 'NONE', #51035, #5744, #17499, .T. ) ;
#51924 = AXIS2_PLACEMENT_3D ( 'NONE', #21961, #56067, #39289 ) ;
#51925 = LINE ( 'NONE', #30374, #54773 ) ;
#51926 = EDGE_LOOP ( 'NONE', ( #16271, #1597, #22058, #25318 ) ) ;
#51927 = CARTESIAN_POINT ( 'NONE',  ( -27.99923088623136636, 0.000000000000000000, 7.757173251277078130 ) ) ;
#51928 = CARTESIAN_POINT ( 'NONE',  ( -16.79925329029790149, 0.000000000000000000, 13.49544742625427496 ) ) ;
#51929 = ORIENTED_EDGE ( 'NONE', *, *, #10507, .F. ) ;
#51930 = DIRECTION ( 'NONE',  ( -0.5364919789714478471, 0.6444004775717705469, -0.5449076811759709926 ) ) ;
#51931 = VECTOR ( 'NONE', #32276, 999.9999999999998863 ) ;
#51932 = VERTEX_POINT ( 'NONE', #4183 ) ;
#51933 = DIRECTION ( 'NONE',  ( 0.7660212471507180654, -0.6427876096865404731, 0.005961354470445141482 ) ) ;
#51934 = VECTOR ( 'NONE', #48261, 1000.000000000000227 ) ;
#51935 = CARTESIAN_POINT ( 'NONE',  ( 0.000000000000000000, 0.000000000000000000, 2.125000000000000000 ) ) ;
#51936 = EDGE_LOOP ( 'NONE', ( #21774, #19120, #44641, #37538 ) ) ;
#51937 = CARTESIAN_POINT ( 'NONE',  ( -19.60912206198628027, -0.1191753592594197858, 4.398475361799976113 ) ) ;
#51938 = LINE ( 'NONE', #51413, #16583 ) ;
#51939 = LINE ( 'NONE', #21001, #29385 ) ;
#51940 = VECTOR ( 'NONE', #34133, 1000.000000000000227 ) ;
#51941 = DIRECTION ( 'NONE',  ( 0.9335804264972044075, -0.3583679495452936070, 0.000000000000000000 ) ) ;
#51942 = VERTEX_POINT ( 'NONE', #25459 ) ;
#51943 = VECTOR ( 'NONE', #24937, 1000.000000000000114 ) ;
#51944 = AXIS2_PLACEMENT_3D ( 'NONE', #54738, #11018, #16140 ) ;
#51945 = DIRECTION ( 'NONE',  ( 0.5449076811759707706, 0.6444004775717708799, -0.5364919789714476250 ) ) ;
#51946 = DIRECTION ( 'NONE',  ( 0.007781995580012663651, 0.000000000000000000, -0.9999697198139515519 ) ) ;
#51947 = CARTESIAN_POINT ( 'NONE',  ( -11.67244013076689946, 0.000000000000000000, 11.50401908778467863 ) ) ;
#51948 = LINE ( 'NONE', #35228, #5110 ) ;
#51949 = LINE ( 'NONE', #16468, #6885 ) ;
#51950 = EDGE_CURVE ( 'NONE', #43913, #5651, #47313, .T. ) ;
#51951 = DIRECTION ( 'NONE',  ( 0.007781995580012663651, 0.000000000000000000, -0.9999697198139515519 ) ) ;
#51952 = DIRECTION ( 'NONE',  ( 0.000000000000000000, 0.000000000000000000, 1.000000000000000000 ) ) ;
#51953 = VECTOR ( 'NONE', #46124, 1000.000000000000114 ) ;
#51954 = DIRECTION ( 'NONE',  ( 0.005961354470445682716, -0.6427876096865404731, -0.7660212471507180654 ) ) ;
#51955 = CARTESIAN_POINT ( 'NONE',  ( -20.69132718766890022, -0.8417996532631562001, 4.891677461057035714 ) ) ;
#51956 = AXIS2_PLACEMENT_3D ( 'NONE', #4551, #47144, #55971 ) ;
#51957 = ORIENTED_EDGE ( 'NONE', *, *, #38842, .F. ) ;
#51959 = EDGE_CURVE ( 'NONE', #39021, #8140, #17807, .T. ) ;
#51958 = SURFACE_STYLE_USAGE ( .BOTH. , #29845 ) ;
#51960 = CARTESIAN_POINT ( 'NONE',  ( -17.46532115785441519, 0.000000000000000000, 13.67492996699914265 ) ) ;
#51961 = EDGE_LOOP ( 'NONE', ( #7288, #8869, #17123, #29088 ) ) ;
#51962 = CARTESIAN_POINT ( 'NONE',  ( -17.86155299234406968, 0.000000000000000000, 4.881410446302820283 ) ) ;
#51964 = EDGE_CURVE ( 'NONE', #27005, #34418, #43613, .T. ) ;
#51963 = CARTESIAN_POINT ( 'NONE',  ( -13.54949002605227726, -3.432230869623161595, 2.034897051475980323 ) ) ;
#51965 = ADVANCED_FACE ( 'NONE', ( #26582 ), #55855, .F. ) ;
#51966 = DIRECTION ( 'NONE',  ( -0.005002170337468016433, -0.7660444431189770143, 0.6427681459581293666 ) ) ;
#51967 = VECTOR ( 'NONE', #55362, 1000.000000000000000 ) ;
#51968 = VECTOR ( 'NONE', #42509, 1000.000000000000227 ) ;
#51969 = FACE_OUTER_BOUND ( 'NONE', #50116, .T. ) ;
#51970 = FACE_OUTER_BOUND ( 'NONE', #31871, .T. ) ;
#51971 = VERTEX_POINT ( 'NONE', #4726 ) ;
#51972 = ORIENTED_EDGE ( 'NONE', *, *, #55163, .F. ) ;
#51973 = DIRECTION ( 'NONE',  ( 0.000000000000000000, 0.000000000000000000, -1.000000000000000000 ) ) ;
#51974 = DIRECTION ( 'NONE',  ( -0.9999697198139514409, -0.000000000000000000, -0.007781995580013368816 ) ) ;
#51975 = ORIENTED_EDGE ( 'NONE', *, *, #29108, .F. ) ;
#51976 = VECTOR ( 'NONE', #38704, 1000.000000000000227 ) ;
#51977 = FACE_OUTER_BOUND ( 'NONE', #43489, .T. ) ;
#51978 = ORIENTED_EDGE ( 'NONE', *, *, #18533, .T. ) ;
#51979 = DIRECTION ( 'NONE',  ( -0.9999697198139514409, -0.000000000000000000, -0.007781995580013368816 ) ) ;
#51980 = VECTOR ( 'NONE', #32162, 1000.000000000000227 ) ;
#51981 = ORIENTED_EDGE ( 'NONE', *, *, #32818, .T. ) ;
#51982 = LINE ( 'NONE', #26708, #52882 ) ;
#51983 = VERTEX_POINT ( 'NONE', #12429 ) ;
#51984 = ORIENTED_EDGE ( 'NONE', *, *, #21695, .F. ) ;
#51985 = ORIENTED_EDGE ( 'NONE', *, *, #48274, .T. ) ;
#51986 = DIRECTION ( 'NONE',  ( 0.007781995580012663651, 0.000000000000000000, -0.9999697198139515519 ) ) ;
#51987 = VECTOR ( 'NONE', #5230, 999.9999999999998863 ) ;
#51988 = ADVANCED_FACE ( 'NONE', ( #5778 ), #52436, .F. ) ;
#51989 = DIRECTION ( 'NONE',  ( -0.005002170337468016433, -0.7660444431189770143, 0.6427681459581293666 ) ) ;
#51990 = CARTESIAN_POINT ( 'NONE',  ( -6.110905869600904872, 1.712176620043476140E-14, -4.599999999999999645 ) ) ;
#51991 = VECTOR ( 'NONE', #15684, 1000.000000000000000 ) ;
#51992 = VECTOR ( 'NONE', #15705, 1000.000000000000114 ) ;
#51993 = EDGE_CURVE ( 'NONE', #44163, #42918, #13532, .T. ) ;
#51994 = CARTESIAN_POINT ( 'NONE',  ( -12.29453239076688753, 0.000000000000000000, 6.032730497292229543 ) ) ;
#51995 = ORIENTED_EDGE ( 'NONE', *, *, #54952, .F. ) ;
#51996 = ORIENTED_EDGE ( 'NONE', *, *, #50651, .F. ) ;
#51997 = EDGE_CURVE ( 'NONE', #13096, #37283, #30846, .T. ) ;
#51998 = EDGE_CURVE ( 'NONE', #15364, #55560, #9258, .T. ) ;
#51999 = VECTOR ( 'NONE', #8565, 1000.000000000000000 ) ;
#52000 = ORIENTED_EDGE ( 'NONE', *, *, #46818, .F. ) ;
#52001 = VECTOR ( 'NONE', #41632, 999.9999999999998863 ) ;
#52002 = LINE ( 'NONE', #55152, #12231 ) ;
#52003 = ORIENTED_EDGE ( 'NONE', *, *, #6679, .T. ) ;
#52004 = DIRECTION ( 'NONE',  ( 0.7660212471507180654, -0.6427876096865404731, 0.005961354470445141482 ) ) ;
#52005 = ORIENTED_EDGE ( 'NONE', *, *, #40941, .T. ) ;
#52006 = CARTESIAN_POINT ( 'NONE',  ( -30.79411802867772607, 0.000000000000000000, 8.643412946479525516 ) ) ;
#52007 = DIRECTION ( 'NONE',  ( -0.005961354470445682716, -0.6427876096865404731, 0.7660212471507180654 ) ) ;
#52008 = ORIENTED_EDGE ( 'NONE', *, *, #19560, .F. ) ;
#52009 = LINE ( 'NONE', #4875, #47671 ) ;
#52010 = ORIENTED_EDGE ( 'NONE', *, *, #37894, .F. ) ;
#52011 = EDGE_CURVE ( 'NONE', #34091, #37711, #44661, .T. ) ;
#52012 = PLANE ( 'NONE',  #50863 ) ;
#52013 = VECTOR ( 'NONE', #8023, 1000.000000000000227 ) ;
#52014 = ORIENTED_EDGE ( 'NONE', *, *, #43340, .T. ) ;
#52015 = CARTESIAN_POINT ( 'NONE',  ( -24.27063949748155380, 0.000000000000000000, 6.308861732390097288 ) ) ;
#52016 = DIRECTION ( 'NONE',  ( 0.005961354470445682716, -0.6427876096865404731, -0.7660212471507180654 ) ) ;
#52017 = DIRECTION ( 'NONE',  ( 0.9999697198139515519, 0.000000000000000000, 0.007781995580013368816 ) ) ;
#52018 = EDGE_LOOP ( 'NONE', ( #23464, #45439, #43412, #48463 ) ) ;
#52019 = VECTOR ( 'NONE', #50753, 1000.000000000000227 ) ;
#52020 = LINE ( 'NONE', #40851, #52887 ) ;
#52021 = DIRECTION ( 'NONE',  ( 0.007781995580012662783, 0.000000000000000000, -0.9999697198139514409 ) ) ;
#52022 = CARTESIAN_POINT ( 'NONE',  ( -23.23471500290295921, 19.24370688441070953, -4.657437592157546824 ) ) ;
#52023 = AXIS2_PLACEMENT_3D ( 'NONE', #4265, #17882, #29816 ) ;
#52024 = DIRECTION ( 'NONE',  ( -0.6427681459581293666, -0.7660444431189770143, -0.005002170337467561935 ) ) ;
#52025 = PLANE ( 'NONE',  #27648 ) ;
#52026 = FACE_OUTER_BOUND ( 'NONE', #4779, .T. ) ;
#52027 = SURFACE_STYLE_FILL_AREA ( #4609 ) ;
#52028 = ORIENTED_EDGE ( 'NONE', *, *, #23773, .F. ) ;
#52029 = PLANE ( 'NONE',  #18941 ) ;
#52030 = CARTESIAN_POINT ( 'NONE',  ( -18.24297520525825433, 4.819660872929008910, 11.87739681187417773 ) ) ;
#52031 = CARTESIAN_POINT ( 'NONE',  ( -18.98145280571277027, -5.375054281893163477, 12.87635240835876438 ) ) ;
#52032 = ORIENTED_EDGE ( 'NONE', *, *, #25254, .F. ) ;
#52033 = VECTOR ( 'NONE', #39849, 999.9999999999998863 ) ;
#52034 = CARTESIAN_POINT ( 'NONE',  ( -24.27063949748155380, 0.000000000000000000, 6.308861732390097288 ) ) ;
#52035 = ORIENTED_EDGE ( 'NONE', *, *, #42708, .F. ) ;
#52036 = AXIS2_PLACEMENT_3D ( 'NONE', #35217, #31212, #26381 ) ;
#52037 = FACE_OUTER_BOUND ( 'NONE', #49856, .T. ) ;
#52038 = ADVANCED_FACE ( 'NONE', ( #36424 ), #37257, .F. ) ;
#52039 = DIRECTION ( 'NONE',  ( -0.5364919789714478471, 0.6444004775717705469, -0.5449076811759709926 ) ) ;
#52040 = LINE ( 'NONE', #52600, #18750 ) ;
#52041 = CARTESIAN_POINT ( 'NONE',  ( -68.28917301125578376, 0.1329764677542568940, 4.678579668399310165 ) ) ;
#52042 = ORIENTED_EDGE ( 'NONE', *, *, #51861, .F. ) ;
#52043 = AXIS2_PLACEMENT_3D ( 'NONE', #6798, #15866, #41152 ) ;
#52044 = VECTOR ( 'NONE', #41304, 999.9999999999998863 ) ;
#52045 = ORIENTED_EDGE ( 'NONE', *, *, #30144, .F. ) ;
#52046 = CARTESIAN_POINT ( 'NONE',  ( -13.95727774206300786, 0.000000000000000000, 6.558448711888932969 ) ) ;
#52047 = LINE ( 'NONE', #48066, #31358 ) ;
#52048 = LINE ( 'NONE', #21944, #36090 ) ;
#52049 = ADVANCED_FACE ( 'NONE', ( #54559 ), #15667, .F. ) ;
#52050 = DIRECTION ( 'NONE',  ( 0.007781995580012663651, -3.146120232559066537E-19, -0.9999697198139514409 ) ) ;
#52051 = CARTESIAN_POINT ( 'NONE',  ( -9.829290562097927619, 1.000354561442236001, 1.688498333329506051 ) ) ;
#52052 = DIRECTION ( 'NONE',  ( 0.000000000000000000, -1.000000000000000000, 0.000000000000000000 ) ) ;
#52054 = EDGE_CURVE ( 'NONE', #27710, #27265, #54305, .T. ) ;
#52053 = VERTEX_POINT ( 'NONE', #37003 ) ;
#52055 = CARTESIAN_POINT ( 'NONE',  ( -6.110905869600904872, 1.712176620043476140E-14, 2.600000000000000089 ) ) ;
#52056 = EDGE_CURVE ( 'NONE', #11058, #20365, #54039, .T. ) ;
#52057 = VECTOR ( 'NONE', #24994, 1000.000000000000227 ) ;
#52058 = PLANE ( 'NONE',  #7016 ) ;
#52059 = EDGE_LOOP ( 'NONE', ( #48993, #47307, #21830, #2415, #15386 ) ) ;
#52060 = AXIS2_PLACEMENT_3D ( 'NONE', #9771, #22262, #1518 ) ;
#52061 = PLANE ( 'NONE',  #39231 ) ;
#52062 = ADVANCED_FACE ( 'NONE', ( #6338 ), #33004, .F. ) ;
#52063 = CARTESIAN_POINT ( 'NONE',  ( -19.49193266702258853, -0.5179957512181551094, 5.103379603946674337 ) ) ;
#52064 = VECTOR ( 'NONE', #33644, 1000.000000000000000 ) ;
#52065 = LINE ( 'NONE', #56064, #52929 ) ;
#52066 = EDGE_LOOP ( 'NONE', ( #20269, #42423, #34664, #13766 ) ) ;
#52067 = DIRECTION ( 'NONE',  ( 0.5364919789714477361, 0.6444004775717706579, 0.5449076811759711036 ) ) ;
#52068 = EDGE_CURVE ( 'NONE', #14352, #5802, #2045, .T. ) ;
#52069 = VECTOR ( 'NONE', #36578, 1000.000000000000114 ) ;
#52070 = ORIENTED_EDGE ( 'NONE', *, *, #31837, .F. ) ;
#52071 = ADVANCED_FACE ( 'NONE', ( #50322 ), #19099, .F. ) ;
#52072 = ORIENTED_EDGE ( 'NONE', *, *, #33697, .T. ) ;
#52073 = ORIENTED_EDGE ( 'NONE', *, *, #19365, .T. ) ;
#52074 = VERTEX_POINT ( 'NONE', #49507 ) ;
#52075 = VECTOR ( 'NONE', #42570, 999.9999999999998863 ) ;
#52076 = DIRECTION ( 'NONE',  ( -0.5364919789714478471, 0.6444004775717705469, -0.5449076811759709926 ) ) ;
#52077 = VERTEX_POINT ( 'NONE', #36717 ) ;
#52078 = CARTESIAN_POINT ( 'NONE',  ( -12.12997044929294965, 23.92298333415059375, -3.477585481046854721 ) ) ;
#52079 = VECTOR ( 'NONE', #18362, 999.9999999999998863 ) ;
#52080 = EDGE_CURVE ( 'NONE', #45468, #41108, #24471, .T. ) ;
#52081 = ORIENTED_EDGE ( 'NONE', *, *, #22725, .F. ) ;
#52082 = DIRECTION ( 'NONE',  ( -0.9999697198139514409, -0.000000000000000000, -0.007781995580013368816 ) ) ;
#52083 = ORIENTED_EDGE ( 'NONE', *, *, #20186, .F. ) ;
#52084 = FACE_OUTER_BOUND ( 'NONE', #50640, .T. ) ;
#52085 = ORIENTED_EDGE ( 'NONE', *, *, #5022, .T. ) ;
#52086 = EDGE_CURVE ( 'NONE', #32862, #11430, #53474, .T. ) ;
#52087 = VECTOR ( 'NONE', #39425, 1000.000000000000227 ) ;
#52088 = VECTOR ( 'NONE', #41875, 1000.000000000000227 ) ;
#52089 = FACE_OUTER_BOUND ( 'NONE', #35200, .T. ) ;
#52090 = DIRECTION ( 'NONE',  ( 0.9999697198139515519, 0.000000000000000000, 0.007781995580013368816 ) ) ;
#52091 = LINE ( 'NONE', #8669, #34142 ) ;
#52092 = DIRECTION ( 'NONE',  ( -0.6427681459581293666, -0.7660444431189770143, -0.005002170337467561935 ) ) ;
#52093 = DIRECTION ( 'NONE',  ( 0.5449076811759707706, 0.6444004775717708799, -0.5364919789714476250 ) ) ;
#52094 = EDGE_LOOP ( 'NONE', ( #34475, #5221, #3410, #46169 ) ) ;
#52095 = ORIENTED_EDGE ( 'NONE', *, *, #26297, .T. ) ;
#52096 = DIRECTION ( 'NONE',  ( 0.5449076811759707706, 0.6444004775717708799, -0.5364919789714476250 ) ) ;
#52097 = CARTESIAN_POINT ( 'NONE',  ( -58.00000000000000711, -9.000000000000000000, 3.457106781186559896 ) ) ;
#52098 = DIRECTION ( 'NONE',  ( 0.000000000000000000, -1.000000000000000000, 0.000000000000000000 ) ) ;
#52099 = VECTOR ( 'NONE', #9268, 1000.000000000000227 ) ;
#52100 = PLANE ( 'NONE',  #14162 ) ;
#52101 = VECTOR ( 'NONE', #15579, 1000.000000000000227 ) ;
#52102 = FACE_OUTER_BOUND ( 'NONE', #4389, .T. ) ;
#52103 = LINE ( 'NONE', #50962, #54950 ) ;
#52104 = ORIENTED_EDGE ( 'NONE', *, *, #28454, .F. ) ;
#52105 = DIRECTION ( 'NONE',  ( 0.5364919789714477361, 0.6444004775717706579, 0.5449076811759711036 ) ) ;
#52106 = DIRECTION ( 'NONE',  ( 0.007781995580012662783, 0.000000000000000000, -0.9999697198139514409 ) ) ;
#52107 = AXIS2_PLACEMENT_3D ( 'NONE', #10197, #44841, #35477 ) ;
#52108 = EDGE_LOOP ( 'NONE', ( #50838, #48288, #50614, #21501 ) ) ;
#52109 = LINE ( 'NONE', #16931, #24316 ) ;
#52110 = FACE_OUTER_BOUND ( 'NONE', #46014, .T. ) ;
#52111 = EDGE_CURVE ( 'NONE', #6114, #93, #46066, .T. ) ;
#52112 = CARTESIAN_POINT ( 'NONE',  ( -33.59056157024009082, 0.000000000000000000, 9.729646585644761814 ) ) ;
#52113 = DIRECTION ( 'NONE',  ( 0.005002170337468016433, -0.7660444431189770143, -0.6427681459581293666 ) ) ;
#52114 = DIRECTION ( 'NONE',  ( 0.7660212471507180654, -0.6427876096865404731, 0.005961354470445141482 ) ) ;
#52115 = ORIENTED_EDGE ( 'NONE', *, *, #39489, .T. ) ;
#52116 = VECTOR ( 'NONE', #39691, 1000.000000000000227 ) ;
#52117 = ORIENTED_EDGE ( 'NONE', *, *, #29291, .T. ) ;
#52118 = VECTOR ( 'NONE', #7434, 1000.000000000000227 ) ;
#52119 = FACE_OUTER_BOUND ( 'NONE', #30657, .T. ) ;
#52120 = CARTESIAN_POINT ( 'NONE',  ( -58.00000000000000711, 0.000000000000000000, 3.000000000000008438 ) ) ;
#52121 = DIRECTION ( 'NONE',  ( 0.007781995580012663651, 0.000000000000000000, -0.9999697198139515519 ) ) ;
#52122 = AXIS2_PLACEMENT_3D ( 'NONE', #9668, #27523, #10505 ) ;
#52123 = LINE ( 'NONE', #39064, #1037 ) ;
#52124 = DIRECTION ( 'NONE',  ( 0.000000000000000000, -0.000000000000000000, -1.000000000000000000 ) ) ;
#52125 = CARTESIAN_POINT ( 'NONE',  ( -18.33325565058499862, 0.000000000000000000, 5.785729700345316751 ) ) ;
#52126 = PLANE ( 'NONE',  #31125 ) ;
#52128 = EDGE_CURVE ( 'NONE', #32474, #48923, #19937, .T. ) ;
#52127 = ORIENTED_EDGE ( 'NONE', *, *, #46327, .F. ) ;
#52129 = VECTOR ( 'NONE', #669, 1000.000000000000000 ) ;
#52130 = LINE ( 'NONE', #9830, #45904 ) ;
#52131 = AXIS2_PLACEMENT_3D ( 'NONE', #16075, #54393, #54666 ) ;
#52132 = PLANE ( 'NONE',  #37815 ) ;
#52133 = ORIENTED_EDGE ( 'NONE', *, *, #20660, .T. ) ;
#52134 = FACE_OUTER_BOUND ( 'NONE', #17290, .T. ) ;
#52135 = ORIENTED_EDGE ( 'NONE', *, *, #51352, .T. ) ;
#52136 = LINE ( 'NONE', #30838, #54931 ) ;
#52137 = FACE_OUTER_BOUND ( 'NONE', #14448, .T. ) ;
#52138 = EDGE_LOOP ( 'NONE', ( #50854, #843, #42702, #40832 ) ) ;
#52139 = EDGE_CURVE ( 'NONE', #49589, #30407, #6908, .T. ) ;
#52140 = ORIENTED_EDGE ( 'NONE', *, *, #18641, .F. ) ;
#52141 = EDGE_CURVE ( 'NONE', #52348, #28760, #41251, .T. ) ;
#52142 = AXIS2_PLACEMENT_3D ( 'NONE', #30882, #34580, #9609 ) ;
#52143 = EDGE_LOOP ( 'NONE', ( #41183, #12420, #26590 ) ) ;
#52144 = EDGE_LOOP ( 'NONE', ( #28528, #13423, #22953, #47410 ) ) ;
#52145 = ORIENTED_EDGE ( 'NONE', *, *, #41044, .T. ) ;
#52146 = VECTOR ( 'NONE', #163, 999.9999999999998863 ) ;
#52147 = EDGE_LOOP ( 'NONE', ( #43524, #41853, #48051, #10898 ) ) ;
#52148 = DIRECTION ( 'NONE',  ( 0.9999697198139515519, 0.000000000000000000, 0.007781995580013368816 ) ) ;
#52149 = CARTESIAN_POINT ( 'NONE',  ( -20.54126990917373519, -0.1191753592594197858, 4.760553241521720658 ) ) ;
#52150 = AXIS2_PLACEMENT_3D ( 'NONE', #2382, #45525, #12004 ) ;
#52151 = EDGE_CURVE ( 'NONE', #35896, #34812, #310, .T. ) ;
#52152 = ORIENTED_EDGE ( 'NONE', *, *, #27315, .F. ) ;
#52153 = DIRECTION ( 'NONE',  ( 0.000000000000000000, -1.000000000000000000, 0.000000000000000000 ) ) ;
#52154 = ORIENTED_EDGE ( 'NONE', *, *, #18798, .T. ) ;
#52155 = VECTOR ( 'NONE', #45071, 999.9999999999998863 ) ;
#52156 = ORIENTED_EDGE ( 'NONE', *, *, #38954, .F. ) ;
#52157 = EDGE_CURVE ( 'NONE', #16476, #11761, #20208, .T. ) ;
#52158 = AXIS2_PLACEMENT_3D ( 'NONE', #8356, #20853, #25401 ) ;
#52159 = AXIS2_PLACEMENT_3D ( 'NONE', #37282, #28791, #46650 ) ;
#52160 = DIRECTION ( 'NONE',  ( 0.007781995580012662783, 0.000000000000000000, -0.9999697198139514409 ) ) ;
#52161 = DIRECTION ( 'NONE',  ( -0.6427681459581293666, -0.7660444431189770143, -0.005002170337467561935 ) ) ;
#52162 = VECTOR ( 'NONE', #29704, 1000.000000000000227 ) ;
#52163 = CARTESIAN_POINT ( 'NONE',  ( -10.76106947438395167, -0.1191753592594190225, 0.9615912556445452841 ) ) ;
#52164 = EDGE_LOOP ( 'NONE', ( #51671, #27615, #37241, #19250 ) ) ;
#52165 = DIRECTION ( 'NONE',  ( -0.3620778797217457101, 0.000000000000000000, -0.9321478471874540261 ) ) ;
#52166 = EDGE_LOOP ( 'NONE', ( #7552, #1883, #47537, #23073 ) ) ;
#52167 = VECTOR ( 'NONE', #41141, 1000.000000000000227 ) ;
#52168 = DIRECTION ( 'NONE',  ( -0.5449076811759708816, 0.6444004775717707689, 0.5364919789714475140 ) ) ;
#52169 = PLANE ( 'NONE',  #32095 ) ;
#52170 = VECTOR ( 'NONE', #7567, 999.9999999999998863 ) ;
#52171 = FACE_OUTER_BOUND ( 'NONE', #29315, .T. ) ;
#52172 = VECTOR ( 'NONE', #6571, 1000.000000000000227 ) ;
#52173 = CARTESIAN_POINT ( 'NONE',  ( -15.81582532942734431, 0.000000000000000000, 6.543985064816895125 ) ) ;
#52174 = CARTESIAN_POINT ( 'NONE',  ( -18.75581683353525619, -4.565544526780660917, 11.46016431438283334 ) ) ;
#52175 = PLANE ( 'NONE',  #7656 ) ;
#52176 = DIRECTION ( 'NONE',  ( 0.6246952433987893460, 0.7422098413412802076, -0.2426528472758539279 ) ) ;
#52177 = DIRECTION ( 'NONE',  ( -0.5449076811759708816, 0.6444004775717707689, 0.5364919789714475140 ) ) ;
#52178 = ORIENTED_EDGE ( 'NONE', *, *, #1235, .T. ) ;
#52179 = CARTESIAN_POINT ( 'NONE',  ( -17.14676106981525550, -2.137015261443158565, 6.849522152733298341 ) ) ;
#52180 = EDGE_CURVE ( 'NONE', #8547, #46010, #28458, .T. ) ;
#52181 = PLANE ( 'NONE',  #30162 ) ;
#52182 = DIRECTION ( 'NONE',  ( 0.000000000000000000, -1.000000000000000000, 0.000000000000000000 ) ) ;
#52183 = DIRECTION ( 'NONE',  ( 0.007781995580012662783, 0.000000000000000000, -0.9999697198139514409 ) ) ;
#52184 = EDGE_CURVE ( 'NONE', #15174, #37067, #5976, .T. ) ;
#52185 = DIRECTION ( 'NONE',  ( -0.005961354470445682716, -0.6427876096865404731, 0.7660212471507180654 ) ) ;
#52186 = PLANE ( 'NONE',  #32237 ) ;
#52187 = DIRECTION ( 'NONE',  ( 0.005002170337468016433, -0.7660444431189770143, -0.6427681459581293666 ) ) ;
#52188 = VECTOR ( 'NONE', #18304, 1000.000000000000227 ) ;
#52189 = DIRECTION ( 'NONE',  ( -0.6427681459581293666, -0.7660444431189770143, -0.005002170337467561935 ) ) ;
#52190 = ADVANCED_FACE ( 'NONE', ( #42075 ), #50612, .F. ) ;
#52191 = SHAPE_DEFINITION_REPRESENTATION ( #40961, #24540 ) ;
#52192 = VECTOR ( 'NONE', #47745, 1000.000000000000114 ) ;
#52193 = ORIENTED_EDGE ( 'NONE', *, *, #8176, .T. ) ;
#52194 = EDGE_CURVE ( 'NONE', #42137, #4086, #15977, .T. ) ;
#52195 = CARTESIAN_POINT ( 'NONE',  ( -19.06545585621813999, 19.91877896750159138, 4.274096488885640532 ) ) ;
#52196 = DIRECTION ( 'NONE',  ( 0.007781995580012663651, 0.000000000000000000, -0.9999697198139515519 ) ) ;
#52197 = CARTESIAN_POINT ( 'NONE',  ( -12.30447220567201860, 0.000000000000000000, 7.309975366360497162 ) ) ;
#52198 = VECTOR ( 'NONE', #16076, 999.9999999999998863 ) ;
#52199 = ADVANCED_FACE ( 'NONE', ( #20516 ), #55703, .F. ) ;
#52200 = EDGE_CURVE ( 'NONE', #2695, #26378, #56005, .T. ) ;
#52201 = EDGE_CURVE ( 'NONE', #28225, #12870, #55151, .T. ) ;
#52202 = LINE ( 'NONE', #26342, #44528 ) ;
#52203 = VECTOR ( 'NONE', #34705, 1000.000000000000114 ) ;
#52204 = DIRECTION ( 'NONE',  ( 0.000000000000000000, -1.000000000000000000, 0.000000000000000000 ) ) ;
#52205 = LINE ( 'NONE', #4502, #37702 ) ;
#52206 = CARTESIAN_POINT ( 'NONE',  ( -14.66887761629205222, 0.000000000000000000, 12.58869632783390990 ) ) ;
#52207 = CARTESIAN_POINT ( 'NONE',  ( -14.92512947252347466, -5.536956232915663634, 11.56644735637827104 ) ) ;
#52208 = AXIS2_PLACEMENT_3D ( 'NONE', #48682, #2054, #36434 ) ;
#52209 = DIRECTION ( 'NONE',  ( 0.7660212471507180654, -0.6427876096865404731, 0.005961354470445141482 ) ) ;
#52210 = AXIS2_PLACEMENT_3D ( 'NONE', #51010, #42775, #55866 ) ;
#52211 = EDGE_LOOP ( 'NONE', ( #16914, #45568, #44335, #36660 ) ) ;
#52212 = LINE ( 'NONE', #43955, #23782 ) ;
#52213 = VECTOR ( 'NONE', #47279, 1000.000000000000227 ) ;
#52214 = ORIENTED_EDGE ( 'NONE', *, *, #50856, .T. ) ;
#52215 = VECTOR ( 'NONE', #10624, 1000.000000000000227 ) ;
#52216 = EDGE_CURVE ( 'NONE', #40111, #17065, #29023, .T. ) ;
#52217 = AXIS2_PLACEMENT_3D ( 'NONE', #36920, #15319, #32630 ) ;
#52218 = VECTOR ( 'NONE', #5295, 1000.000000000000114 ) ;
#52219 = EDGE_CURVE ( 'NONE', #19083, #41253, #51162, .T. ) ;
#52220 = ORIENTED_EDGE ( 'NONE', *, *, #32555, .F. ) ;
#52221 = VECTOR ( 'NONE', #5061, 999.9999999999998863 ) ;
#52222 = VERTEX_POINT ( 'NONE', #42636 ) ;
#52223 = ORIENTED_EDGE ( 'NONE', *, *, #28853, .F. ) ;
#52224 = ADVANCED_FACE ( 'NONE', ( #3469 ), #34151, .F. ) ;
#52225 = ORIENTED_EDGE ( 'NONE', *, *, #53156, .T. ) ;
#52226 = CARTESIAN_POINT ( 'NONE',  ( -14.66494788901886714, 5.629170628041515023, 2.198695500334132191 ) ) ;
#52227 = CARTESIAN_POINT ( 'NONE',  ( -20.54126990917373519, -0.1191753592594197858, 4.760553241521720658 ) ) ;
#52228 = EDGE_CURVE ( 'NONE', #4182, #17775, #50869, .T. ) ;
#52229 = ORIENTED_EDGE ( 'NONE', *, *, #29913, .T. ) ;
#52230 = EDGE_LOOP ( 'NONE', ( #2955, #31425, #31970 ) ) ;
#52231 = VECTOR ( 'NONE', #52809, 1000.000000000000000 ) ;
#52232 = DIRECTION ( 'NONE',  ( 0.007781995580012662783, 0.000000000000000000, -0.9999697198139514409 ) ) ;
#52233 = ORIENTED_EDGE ( 'NONE', *, *, #54800, .T. ) ;
#52234 = DIRECTION ( 'NONE',  ( -0.7660212471507179544, -0.6427876096865405842, -0.005961354470445141482 ) ) ;
#52235 = LINE ( 'NONE', #13343, #488 ) ;
#52236 = ORIENTED_EDGE ( 'NONE', *, *, #20159, .F. ) ;
#52237 = VECTOR ( 'NONE', #16855, 1000.000000000000227 ) ;
#52238 = DIRECTION ( 'NONE',  ( 0.007781995580012663651, 0.000000000000000000, -0.9999697198139515519 ) ) ;
#52239 = VERTEX_POINT ( 'NONE', #46320 ) ;
#52240 = DIRECTION ( 'NONE',  ( 0.007781995580012663651, -3.146120232559066537E-19, -0.9999697198139514409 ) ) ;
#52241 = AXIS2_PLACEMENT_3D ( 'NONE', #35017, #43505, #21918 ) ;
#52242 = LINE ( 'NONE', #13351, #3687 ) ;
#52243 = VECTOR ( 'NONE', #40604, 1000.000000000000114 ) ;
#52244 = VECTOR ( 'NONE', #100, 1000.000000000000114 ) ;
#52245 = EDGE_LOOP ( 'NONE', ( #10602, #50446, #20513, #36156 ) ) ;
#52246 = PLANE ( 'NONE',  #13169 ) ;
#52247 = DIRECTION ( 'NONE',  ( 0.007781995580012662783, 0.000000000000000000, -0.9999697198139514409 ) ) ;
#52248 = CARTESIAN_POINT ( 'NONE',  ( -12.80458192191714595, 0.000000000000000000, 11.86454056839041726 ) ) ;
#52249 = ORIENTED_EDGE ( 'NONE', *, *, #24626, .F. ) ;
#52250 = CARTESIAN_POINT ( 'NONE',  ( -9.764049456472102761, 0.000000000000000000, 5.113753104769962476 ) ) ;
#52251 = ORIENTED_EDGE ( 'NONE', *, *, #9865, .F. ) ;
#52252 = VECTOR ( 'NONE', #26994, 1000.000000000000227 ) ;
#52253 = AXIS2_PLACEMENT_3D ( 'NONE', #45318, #32279, #32548 ) ;
#52254 = LINE ( 'NONE', #21301, #17422 ) ;
#52255 = CARTESIAN_POINT ( 'NONE',  ( -20.02908140811766913, -1.193365355704625541, 6.079151905931945876 ) ) ;
#52256 = DIRECTION ( 'NONE',  ( -0.3313982828793700097, 0.4028455766673915694, -0.8531650599175529814 ) ) ;
#52257 = CARTESIAN_POINT ( 'NONE',  ( -10.37421533196711465, -0.1191753592594197858, 10.96012406864405975 ) ) ;
#52258 = FACE_OUTER_BOUND ( 'NONE', #41274, .T. ) ;
#52259 = CARTESIAN_POINT ( 'NONE',  ( -14.43784130554650424, 0.000000000000000000, 8.601375260372536857 ) ) ;
#52260 = DIRECTION ( 'NONE',  ( -0.2426528472758541499, 0.7422098413412800966, -0.6246952433987894571 ) ) ;
#52261 = AXIS2_PLACEMENT_3D ( 'NONE', #21890, #34667, #51989 ) ;
#52262 = VECTOR ( 'NONE', #53510, 999.9999999999998863 ) ;
#52263 = CARTESIAN_POINT ( 'NONE',  ( 5.618093942130458096, -1.050357310661657939, 2.260478214906367800 ) ) ;
#52264 = DIRECTION ( 'NONE',  ( -0.6427681459581293666, -0.7660444431189770143, -0.005002170337467561935 ) ) ;
#52265 = EDGE_LOOP ( 'NONE', ( #38028, #27796, #22945 ) ) ;
#52266 = CARTESIAN_POINT ( 'NONE',  ( -11.67244013076689946, 0.000000000000000000, 11.50401908778467863 ) ) ;
#52267 = CARTESIAN_POINT ( 'NONE',  ( -15.87975247367846166, 0.000000000000000000, 2.850166870931599927 ) ) ;
#52268 = LINE ( 'NONE', #38136, #36820 ) ;
#52269 = EDGE_CURVE ( 'NONE', #36106, #54291, #4029, .T. ) ;
#52270 = EDGE_CURVE ( 'NONE', #2049, #35294, #55412, .T. ) ;
#52271 = DIRECTION ( 'NONE',  ( -0.9999697198139514409, -0.000000000000000000, -0.007781995580013368816 ) ) ;
#52272 = EDGE_CURVE ( 'NONE', #43300, #3456, #37844, .T. ) ;
#52273 = DIRECTION ( 'NONE',  ( -0.6427681459581293666, -0.7660444431189770143, -0.005002170337467561935 ) ) ;
#52274 = CARTESIAN_POINT ( 'NONE',  ( -13.18201201109693166, 2.714935509636505984, 6.457333944872381437 ) ) ;
#52275 = VECTOR ( 'NONE', #22028, 1000.000000000000000 ) ;
#52276 = ORIENTED_EDGE ( 'NONE', *, *, #817, .F. ) ;
#52277 = ORIENTED_EDGE ( 'NONE', *, *, #31652, .F. ) ;
#52278 = DIRECTION ( 'NONE',  ( 0.7660212471507180654, -0.6427876096865404731, 0.005961354470445141482 ) ) ;
#52279 = CARTESIAN_POINT ( 'NONE',  ( -20.41930778315827766, 0.3880542636427237180, 5.074537440973727165 ) ) ;
#52280 = ORIENTED_EDGE ( 'NONE', *, *, #1552, .F. ) ;
#52281 = AXIS2_PLACEMENT_3D ( 'NONE', #44009, #35234, #52264 ) ;
#52282 = DIRECTION ( 'NONE',  ( 0.000000000000000000, -1.000000000000000000, 0.000000000000000000 ) ) ;
#52283 = VERTEX_POINT ( 'NONE', #54863 ) ;
#52284 = DIRECTION ( 'NONE',  ( -0.005002170337468016433, -0.7660444431189770143, 0.6427681459581293666 ) ) ;
#52285 = VECTOR ( 'NONE', #8328, 1000.000000000000227 ) ;
#52286 = ORIENTED_EDGE ( 'NONE', *, *, #33111, .F. ) ;
#52287 = PLANE ( 'NONE',  #3918 ) ;
#52288 = EDGE_CURVE ( 'NONE', #1421, #1358, #24757, .T. ) ;
#52289 = AXIS2_PLACEMENT_3D ( 'NONE', #8455, #52182, #35708 ) ;
#52290 = ORIENTED_EDGE ( 'NONE', *, *, #41163, .F. ) ;
#52291 = ORIENTED_EDGE ( 'NONE', *, *, #1491, .F. ) ;
#52292 = EDGE_LOOP ( 'NONE', ( #537, #29181, #23137, #45885 ) ) ;
#52293 = ADVANCED_FACE ( 'NONE', ( #33843 ), #12273, .F. ) ;
#52294 = CARTESIAN_POINT ( 'NONE',  ( 1.086233639165236964, 0.000000000000000000, 2.796443541562362078 ) ) ;
#52295 = CARTESIAN_POINT ( 'NONE',  ( -10.74029228357944987, 0.000000000000000000, 11.14194120806293320 ) ) ;
#52296 = DIRECTION ( 'NONE',  ( 0.007781995580012663651, 0.000000000000000000, -0.9999697198139515519 ) ) ;
#52297 = EDGE_CURVE ( 'NONE', #34418, #8057, #38382, .T. ) ;
#52298 = VECTOR ( 'NONE', #14944, 1000.000000000000227 ) ;
#52299 = DIRECTION ( 'NONE',  ( -0.005961354470445682716, -0.6427876096865404731, 0.7660212471507180654 ) ) ;
#52300 = ORIENTED_EDGE ( 'NONE', *, *, #4209, .T. ) ;
#52301 = ORIENTED_EDGE ( 'NONE', *, *, #35122, .F. ) ;
#52302 = EDGE_CURVE ( 'NONE', #51780, #41612, #12502, .T. ) ;
#52303 = AXIS2_PLACEMENT_3D ( 'NONE', #52491, #31187, #34601 ) ;
#52304 = VECTOR ( 'NONE', #25305, 1000.000000000000227 ) ;
#52305 = ORIENTED_EDGE ( 'NONE', *, *, #54635, .T. ) ;
#52306 = CARTESIAN_POINT ( 'NONE',  ( -14.90368544486988789, -2.784623065533159636, 7.041070140637504693 ) ) ;
#52307 = VERTEX_POINT ( 'NONE', #55636 ) ;
#52308 = DIRECTION ( 'NONE',  ( -0.9999697198139514409, 0.000000000000000000, -0.007781995580013368816 ) ) ;
#52309 = EDGE_CURVE ( 'NONE', #9006, #55190, #12201, .T. ) ;
#52310 = ORIENTED_EDGE ( 'NONE', *, *, #3592, .T. ) ;
#52311 = CARTESIAN_POINT ( 'NONE',  ( -32.65997012216863737, 0.000000000000000000, 9.567562649885804404 ) ) ;
#52312 = FACE_OUTER_BOUND ( 'NONE', #24980, .T. ) ;
#52313 = ORIENTED_EDGE ( 'NONE', *, *, #8906, .T. ) ;
#52314 = LINE ( 'NONE', #43494, #5966 ) ;
#52315 = ORIENTED_EDGE ( 'NONE', *, *, #35218, .F. ) ;
#52316 = AXIS2_PLACEMENT_3D ( 'NONE', #7683, #46875, #33520 ) ;
#52317 = LINE ( 'NONE', #38393, #13663 ) ;
#52318 = ORIENTED_EDGE ( 'NONE', *, *, #47587, .F. ) ;
#52319 = LINE ( 'NONE', #49148, #23144 ) ;
#52320 = CARTESIAN_POINT ( 'NONE',  ( -13.63673279712320507, -0.1191753592594197858, 12.22739664767016521 ) ) ;
#52321 = DIRECTION ( 'NONE',  ( -0.7660212471507179544, -0.6427876096865405842, -0.005961354470445141482 ) ) ;
#52322 = ORIENTED_EDGE ( 'NONE', *, *, #18047, .F. ) ;
#52323 = DIRECTION ( 'NONE',  ( 0.007781995580012663651, -3.146120232559066537E-19, -0.9999697198139514409 ) ) ;
#52324 = PLANE ( 'NONE',  #2851 ) ;
#52325 = AXIS2_PLACEMENT_3D ( 'NONE', #19733, #31414, #48730 ) ;
#52326 = CARTESIAN_POINT ( 'NONE',  ( -29.86197018149027116, 0.000000000000000000, 8.281335066757780083 ) ) ;
#52327 = LINE ( 'NONE', #13140, #42178 ) ;
#52328 = PLANE ( 'NONE',  #13091 ) ;
#52329 = CARTESIAN_POINT ( 'NONE',  ( -9.512215248562165826, 1.791064371115911102, 2.504789765260621248 ) ) ;
#52330 = VECTOR ( 'NONE', #5527, 1000.000000000000114 ) ;
#52331 = LINE ( 'NONE', #22511, #11338 ) ;
#52332 = VERTEX_POINT ( 'NONE', #29542 ) ;
#52333 = DIRECTION ( 'NONE',  ( 0.005002170337468016433, -0.7660444431189770143, -0.6427681459581293666 ) ) ;
#52334 = CARTESIAN_POINT ( 'NONE',  ( 2.072287782118878319, 0.000000000000000000, -2.950529333540147015 ) ) ;
#52335 = LINE ( 'NONE', #13438, #50451 ) ;
#52336 = ORIENTED_EDGE ( 'NONE', *, *, #29887, .F. ) ;
#52337 = FACE_OUTER_BOUND ( 'NONE', #45132, .T. ) ;
#52338 = LINE ( 'NONE', #48323, #28143 ) ;
#52339 = ORIENTED_EDGE ( 'NONE', *, *, #1517, .F. ) ;
#52340 = EDGE_CURVE ( 'NONE', #39021, #9132, #42854, .T. ) ;
#52341 = CARTESIAN_POINT ( 'NONE',  ( -9.808144436391993182, 0.000000000000000000, 10.77986332834118777 ) ) ;
#52342 = AXIS2_PLACEMENT_3D ( 'NONE', #1665, #40592, #18993 ) ;
#52343 = CARTESIAN_POINT ( 'NONE',  ( -24.27063949748155380, 0.000000000000000000, 6.308861732390097288 ) ) ;
#52344 = ADVANCED_FACE ( 'NONE', ( #7965 ), #4268, .F. ) ;
#52345 = EDGE_CURVE ( 'NONE', #32268, #44507, #12760, .T. ) ;
#52346 = FACE_OUTER_BOUND ( 'NONE', #50408, .T. ) ;
#52347 = DIRECTION ( 'NONE',  ( 0.5364919789714477361, 0.6444004775717706579, 0.5449076811759711036 ) ) ;
#52348 = VERTEX_POINT ( 'NONE', #21283 ) ;
#52349 = VECTOR ( 'NONE', #52738, 1000.000000000000227 ) ;
#52350 = ORIENTED_EDGE ( 'NONE', *, *, #40815, .F. ) ;
#52351 = CARTESIAN_POINT ( 'NONE',  ( -10.70769351768068844, 0.000000000000000000, 6.953069797522764439 ) ) ;
#52352 = PLANE ( 'NONE',  #13247 ) ;
#52353 = CARTESIAN_POINT ( 'NONE',  ( 2.072287782118878319, 0.000000000000000000, -2.950529333540147015 ) ) ;
#52354 = CARTESIAN_POINT ( 'NONE',  ( -19.60990026154428278, 0.000000000000000000, 4.498472333781370125 ) ) ;
#52355 = CARTESIAN_POINT ( 'NONE',  ( -14.04402961146700335, -5.051250379848162275, 10.42707219621531678 ) ) ;
#52356 = CARTESIAN_POINT ( 'NONE',  ( -18.67619601524082285, 0.000000000000000000, 3.936400510096834893 ) ) ;
#52357 = EDGE_LOOP ( 'NONE', ( #27157, #39252, #43963, #24837 ) ) ;
#52358 = FACE_OUTER_BOUND ( 'NONE', #12460, .T. ) ;
#52359 = LINE ( 'NONE', #38746, #41461 ) ;
#52360 = ORIENTED_EDGE ( 'NONE', *, *, #5793, .T. ) ;
#52361 = CARTESIAN_POINT ( 'NONE',  ( -11.81971693429394854, 0.000000000000000000, 4.728423355324156141 ) ) ;
#52362 = LINE ( 'NONE', #40117, #2302 ) ;
#52363 = CARTESIAN_POINT ( 'NONE',  ( -23.33771345073609638, -0.1191753592594197858, 5.846786880686956955 ) ) ;
#52364 = ORIENTED_EDGE ( 'NONE', *, *, #13424, .T. ) ;
#52365 = CARTESIAN_POINT ( 'NONE',  ( -9.285042292104602524, 0.000000000000000000, 3.270820500249148388 ) ) ;
#52366 = ORIENTED_EDGE ( 'NONE', *, *, #23993, .F. ) ;
#52367 = EDGE_CURVE ( 'NONE', #38901, #53603, #34610, .T. ) ;
#52368 = ORIENTED_EDGE ( 'NONE', *, *, #37229, .T. ) ;
#52369 = VECTOR ( 'NONE', #40178, 999.9999999999998863 ) ;
#52370 = EDGE_LOOP ( 'NONE', ( #20426, #24100, #18269, #33590 ) ) ;
#52371 = EDGE_CURVE ( 'NONE', #25320, #46187, #55942, .T. ) ;
#52372 = ORIENTED_EDGE ( 'NONE', *, *, #27650, .F. ) ;
#52373 = CARTESIAN_POINT ( 'NONE',  ( -20.54204810873173415, 0.000000000000000000, 4.860550213503115558 ) ) ;
#52374 = EDGE_CURVE ( 'NONE', #53467, #54772, #20989, .T. ) ;
#52375 = ORIENTED_EDGE ( 'NONE', *, *, #35667, .F. ) ;
#52376 = LINE ( 'NONE', #35904, #23149 ) ;
#52377 = AXIS2_PLACEMENT_3D ( 'NONE', #6708, #15489, #1867 ) ;
#52378 = VERTEX_POINT ( 'NONE', #34354 ) ;
#52379 = DIRECTION ( 'NONE',  ( 0.7660212471507180654, -0.6427876096865404731, 0.005961354470445141482 ) ) ;
#52380 = EDGE_CURVE ( 'NONE', #7825, #48284, #39501, .T. ) ;
#52381 = EDGE_LOOP ( 'NONE', ( #41521, #33549, #23087, #4444 ) ) ;
#52382 = DIRECTION ( 'NONE',  ( 0.5449076811759707706, 0.6444004775717708799, -0.5364919789714476250 ) ) ;
#52383 = ORIENTED_EDGE ( 'NONE', *, *, #13298, .F. ) ;
#52384 = CARTESIAN_POINT ( 'NONE',  ( -14.46888367232926420, 0.000000000000000000, 12.59025272694991315 ) ) ;
#52385 = CARTESIAN_POINT ( 'NONE',  ( -13.68976073567942642, 0.000000000000000000, 6.191198521283176603 ) ) ;
#52386 = CARTESIAN_POINT ( 'NONE',  ( -12.64114979503688474, -0.1191753592594185784, 3.714037593554236238 ) ) ;
#52387 = CARTESIAN_POINT ( 'NONE',  ( -19.57250508090073993, -5.051250379848164940, 4.322785442357456098 ) ) ;
#52388 = DIRECTION ( 'NONE',  ( 0.9999697198139515519, 0.000000000000000000, 0.007781995580013368816 ) ) ;
#52389 = ORIENTED_EDGE ( 'NONE', *, *, #16425, .T. ) ;
#52390 = ORIENTED_EDGE ( 'NONE', *, *, #13867, .T. ) ;
#52391 = DIRECTION ( 'NONE',  ( 0.007781995580012663651, 0.000000000000000000, -0.9999697198139515519 ) ) ;
#52392 = CARTESIAN_POINT ( 'NONE',  ( -20.29001881650349759, 0.1245042932765033361, 4.966986233812068718 ) ) ;
#52393 = EDGE_CURVE ( 'NONE', #15287, #49949, #13048, .T. ) ;
#52394 = DIRECTION ( 'NONE',  ( 0.3535533905932738974, -0.6123724356957929160, 0.7071067811865487940 ) ) ;
#52395 = CARTESIAN_POINT ( 'NONE',  ( -27.99845268667336384, -0.1191753592594197858, 7.657176279295684118 ) ) ;
#52396 = LINE ( 'NONE', #4139, #1373 ) ;
#52397 = CARTESIAN_POINT ( 'NONE',  ( -20.39447655573265195, -3.756034771668158356, 10.76813197985039139 ) ) ;
#52398 = EDGE_LOOP ( 'NONE', ( #7114, #24966, #49021, #47679, #38696 ) ) ;
#52399 = CARTESIAN_POINT ( 'NONE',  ( -13.07066190154808361, 0.000000000000000000, 12.04713590736729678 ) ) ;
#52400 = EDGE_CURVE ( 'NONE', #53142, #26572, #47964, .T. ) ;
#52401 = DIRECTION ( 'NONE',  ( -0.6427681459581293666, -0.7660444431189770143, -0.005002170337467561935 ) ) ;
#52402 = EDGE_LOOP ( 'NONE', ( #21131, #2988, #52154, #26236 ) ) ;
#52403 = LINE ( 'NONE', #52948, #11633 ) ;
#52404 = LINE ( 'NONE', #34506, #46897 ) ;
#52405 = EDGE_CURVE ( 'NONE', #40825, #52596, #43428, .T. ) ;
#52406 = DIRECTION ( 'NONE',  ( 0.6427681459581294776, -0.7660444431189769032, 0.005002170337467562802 ) ) ;
#52407 = EDGE_CURVE ( 'NONE', #54772, #17736, #51658, .T. ) ;
#52408 = LINE ( 'NONE', #47280, #16880 ) ;
#52409 = PLANE ( 'NONE',  #38318 ) ;
#52410 = ORIENTED_EDGE ( 'NONE', *, *, #29248, .F. ) ;
#52411 = ORIENTED_EDGE ( 'NONE', *, *, #8027, .F. ) ;
#52412 = DIRECTION ( 'NONE',  ( -0.5364919789714478471, 0.6444004775717705469, -0.5449076811759709926 ) ) ;
#52413 = DIRECTION ( 'NONE',  ( 0.007781995580012662783, 0.000000000000000000, -0.9999697198139514409 ) ) ;
#52414 = CARTESIAN_POINT ( 'NONE',  ( -14.14864952550994559, 0.000000000000000000, 5.448963202999637545 ) ) ;
#52415 = EDGE_CURVE ( 'NONE', #32585, #20350, #21832, .T. ) ;
#52416 = AXIS2_PLACEMENT_3D ( 'NONE', #7200, #37028, #54895 ) ;
#52417 = LINE ( 'NONE', #35368, #48212 ) ;
#52418 = LINE ( 'NONE', #1270, #53865 ) ;
#52419 = CARTESIAN_POINT ( 'NONE',  ( -10.43023669639197770, 0.000000000000000000, 5.308574737848737790 ) ) ;
#52420 = PLANE ( 'NONE',  #2975 ) ;
#52421 = ORIENTED_EDGE ( 'NONE', *, *, #40051, .F. ) ;
#52422 = EDGE_CURVE ( 'NONE', #55415, #33685, #43682, .T. ) ;
#52423 = CARTESIAN_POINT ( 'NONE',  ( -21.47419595591918906, 0.000000000000000000, 5.222628093224860102 ) ) ;
#52424 = CARTESIAN_POINT ( 'NONE',  ( -15.86710544311044302, 0.000000000000000000, 13.13336954653252953 ) ) ;
#52425 = ORIENTED_EDGE ( 'NONE', *, *, #11286, .F. ) ;
#52426 = CARTESIAN_POINT ( 'NONE',  ( -14.94916102560700821, 0.000000000000000000, 2.688082935172642962 ) ) ;
#52427 = VERTEX_POINT ( 'NONE', #47695 ) ;
#52428 = FACE_OUTER_BOUND ( 'NONE', #33493, .T. ) ;
#52429 = PLANE ( 'NONE',  #9394 ) ;
#52430 = EDGE_LOOP ( 'NONE', ( #53871, #34605, #19520, #4657, #3638, #3716, #37549, #16775 ) ) ;
#52431 = VERTEX_POINT ( 'NONE', #4798 ) ;
#52432 = ORIENTED_EDGE ( 'NONE', *, *, #36293, .F. ) ;
#52433 = ORIENTED_EDGE ( 'NONE', *, *, #25639, .F. ) ;
#52434 = ORIENTED_EDGE ( 'NONE', *, *, #14530, .T. ) ;
#52435 = VERTEX_POINT ( 'NONE', #38045 ) ;
#52436 = PLANE ( 'NONE',  #30458 ) ;
#52437 = CARTESIAN_POINT ( 'NONE',  ( -9.442067484779661513, -0.1191753592594197858, 10.59804618892231254 ) ) ;
#52438 = LINE ( 'NONE', #5019, #23104 ) ;
#52439 = ORIENTED_EDGE ( 'NONE', *, *, #53734, .F. ) ;
#52440 = LINE ( 'NONE', #17814, #36750 ) ;
#52441 = EDGE_CURVE ( 'NONE', #40396, #21504, #237, .T. ) ;
#52442 = ORIENTED_EDGE ( 'NONE', *, *, #42442, .F. ) ;
#52443 = ORIENTED_EDGE ( 'NONE', *, *, #20459, .F. ) ;
#52444 = LINE ( 'NONE', #4733, #12957 ) ;
#52445 = CARTESIAN_POINT ( 'NONE',  ( -20.08971041202067198, -0.1191753592594192862, 5.502731521554907523 ) ) ;
#52446 = DIRECTION ( 'NONE',  ( 0.9999697198139515519, 0.000000000000000000, 0.007781995580013368816 ) ) ;
#52447 = ORIENTED_EDGE ( 'NONE', *, *, #33931, .F. ) ;
#52448 = DIRECTION ( 'NONE',  ( 0.005002170337468016433, -0.7660444431189770143, -0.6427681459581293666 ) ) ;
#52449 = ORIENTED_EDGE ( 'NONE', *, *, #41783, .T. ) ;
#52450 = EDGE_CURVE ( 'NONE', #52596, #21479, #52235, .T. ) ;
#52451 = AXIS2_PLACEMENT_3D ( 'NONE', #18157, #26393, #51952 ) ;
#52452 = FACE_OUTER_BOUND ( 'NONE', #33526, .T. ) ;
#52453 = PLANE ( 'NONE',  #50185 ) ;
#52454 = ADVANCED_FACE ( 'NONE', ( #17885 ), #49073, .F. ) ;
#52455 = ADVANCED_FACE ( 'NONE', ( #26961 ), #36052, .F. ) ;
#52456 = CARTESIAN_POINT ( 'NONE',  ( -11.22614204225105539, -2.298917212465658277, 4.815461341309315024 ) ) ;
#52457 = DIRECTION ( 'NONE',  ( 0.9999697198139515519, 0.000000000000000000, 0.007781995580013368816 ) ) ;
#52458 = LINE ( 'NONE', #26911, #53148 ) ;
#52459 = DIRECTION ( 'NONE',  ( 0.9999697198139515519, 0.000000000000000000, 0.007781995580013368816 ) ) ;
#52460 = PLANE ( 'NONE',  #53850 ) ;
#52461 = LINE ( 'NONE', #48472, #55844 ) ;
#52462 = ORIENTED_EDGE ( 'NONE', *, *, #53040, .F. ) ;
#52463 = DIRECTION ( 'NONE',  ( 0.000000000000000000, -1.000000000000000000, 0.000000000000000000 ) ) ;
#52464 = CARTESIAN_POINT ( 'NONE',  ( -18.85347906554464004, 0.000000000000000000, 9.105669829700502760 ) ) ;
#52465 = PLANE ( 'NONE',  #40507 ) ;
#52466 = EDGE_CURVE ( 'NONE', #41612, #38710, #44523, .T. ) ;
#52467 = DIRECTION ( 'NONE',  ( 0.5364919789714477361, 0.6444004775717706579, 0.5449076811759711036 ) ) ;
#52468 = DIRECTION ( 'NONE',  ( 0.000000000000000000, -1.000000000000000000, 0.000000000000000000 ) ) ;
#52469 = CARTESIAN_POINT ( 'NONE',  ( -23.33849165029409889, 0.000000000000000000, 5.946783852668351855 ) ) ;
#52470 = EDGE_CURVE ( 'NONE', #16632, #53347, #32040, .T. ) ;
#52471 = CARTESIAN_POINT ( 'NONE',  ( -18.61957337711627858, 0.000000000000000000, 8.568832054460452596 ) ) ;
#52472 = CARTESIAN_POINT ( 'NONE',  ( -16.99924723426068951, 0.000000000000000000, 13.49389102713827171 ) ) ;
#52473 = ORIENTED_EDGE ( 'NONE', *, *, #46692, .T. ) ;
#52474 = CARTESIAN_POINT ( 'NONE',  ( -11.32789590151604209, 0.000000000000000000, 1.238936178477310524 ) ) ;
#52475 = DIRECTION ( 'NONE',  ( 0.000000000000000000, -1.000000000000000000, 0.000000000000000000 ) ) ;
#52476 = LINE ( 'NONE', #21551, #44509 ) ;
#52477 = EDGE_CURVE ( 'NONE', #31034, #40803, #31197, .T. ) ;
#52478 = CARTESIAN_POINT ( 'NONE',  ( -25.83279121425626812, 17.74370688441070953, -4.657437592157546824 ) ) ;
#52479 = LINE ( 'NONE', #13576, #13989 ) ;
#52480 = CARTESIAN_POINT ( 'NONE',  ( -17.83139810946674686, -0.1191753592594197858, 13.85674710641801788 ) ) ;
#52481 = DIRECTION ( 'NONE',  ( 0.6427681459581294776, -0.7660444431189769032, 0.005002170337467562802 ) ) ;
#52482 = EDGE_CURVE ( 'NONE', #14570, #48938, #27495, .T. ) ;
#52483 = CARTESIAN_POINT ( 'NONE',  ( -14.46888367232926420, 0.000000000000000000, 12.59025272694991315 ) ) ;
#52484 = CARTESIAN_POINT ( 'NONE',  ( -14.93495759592298988, 0.000000000000000000, 12.77129166681078409 ) ) ;
#52485 = VECTOR ( 'NONE', #29906, 1000.000000000000114 ) ;
#52486 = ORIENTED_EDGE ( 'NONE', *, *, #8109, .T. ) ;
#52487 = EDGE_LOOP ( 'NONE', ( #55266, #30778, #26025, #9772 ) ) ;
#52488 = VERTEX_POINT ( 'NONE', #10174 ) ;
#52489 = ORIENTED_EDGE ( 'NONE', *, *, #9168, .T. ) ;
#52490 = ORIENTED_EDGE ( 'NONE', *, *, #1503, .F. ) ;
#52491 = CARTESIAN_POINT ( 'NONE',  ( -19.12962290826653700, 0.000000000000000000, 14.40064212555863854 ) ) ;
#52492 = CARTESIAN_POINT ( 'NONE',  ( -27.99923088623136636, 0.000000000000000000, 7.757173251277078130 ) ) ;
#52493 = ORIENTED_EDGE ( 'NONE', *, *, #44814, .T. ) ;
#52494 = VERTEX_POINT ( 'NONE', #44274 ) ;
#52495 = EDGE_CURVE ( 'NONE', #33688, #18589, #18718, .T. ) ;
#52496 = EDGE_CURVE ( 'NONE', #44308, #34678, #22678, .T. ) ;
#52497 = CARTESIAN_POINT ( 'NONE',  ( -12.13851405436063047, 0.000000000000000000, 11.68505802764555135 ) ) ;
#52498 = ORIENTED_EDGE ( 'NONE', *, *, #46826, .F. ) ;
#52499 = LINE ( 'NONE', #13594, #42726 ) ;
#52500 = LINE ( 'NONE', #23259, #15968 ) ;
#52501 = ORIENTED_EDGE ( 'NONE', *, *, #18186, .F. ) ;
#52502 = CARTESIAN_POINT ( 'NONE',  ( -17.21548412696117225, 0.000000000000000000, 7.271756736028395451 ) ) ;
#52503 = EDGE_CURVE ( 'NONE', #56039, #19075, #53610, .T. ) ;
#52504 = EDGE_CURVE ( 'NONE', #308, #37252, #35751, .T. ) ;
#52505 = EDGE_CURVE ( 'NONE', #6183, #31672, #52500, .T. ) ;
#52506 = ORIENTED_EDGE ( 'NONE', *, *, #10844, .T. ) ;
#52507 = FACE_OUTER_BOUND ( 'NONE', #26480, .T. ) ;
#52508 = ADVANCED_FACE ( 'NONE', ( #40583 ), #5633, .F. ) ;
#52509 = DIRECTION ( 'NONE',  ( 0.007781995580012663651, -3.146120232559066537E-19, -0.9999697198139514409 ) ) ;
#52510 = DIRECTION ( 'NONE',  ( 0.005002170337468016433, -0.7660444431189770143, -0.6427681459581293666 ) ) ;
#52511 = ORIENTED_EDGE ( 'NONE', *, *, #15279, .F. ) ;
#52512 = DIRECTION ( 'NONE',  ( -0.6427681459581293666, -0.7660444431189770143, -0.005002170337467561935 ) ) ;
#52513 = LINE ( 'NONE', #22973, #33813 ) ;
#52514 = DIRECTION ( 'NONE',  ( -0.005961354470445682716, -0.6427876096865404731, 0.7660212471507180654 ) ) ;
#52515 = ORIENTED_EDGE ( 'NONE', *, *, #38449, .F. ) ;
#52516 = CARTESIAN_POINT ( 'NONE',  ( -21.24737399725141174, 5.143464774974014553, 4.771029900565397774 ) ) ;
#52517 = ORIENTED_EDGE ( 'NONE', *, *, #5629, .T. ) ;
#52518 =( GEOMETRIC_REPRESENTATION_CONTEXT ( 3 ) GLOBAL_UNCERTAINTY_ASSIGNED_CONTEXT ( ( #55806 ) ) GLOBAL_UNIT_ASSIGNED_CONTEXT ( ( #55666, #25865, #29573 ) ) REPRESENTATION_CONTEXT ( 'NONE', 'WORKASPACE' ) );
#52519 = CARTESIAN_POINT ( 'NONE',  ( -22.40556560354864146, -0.1191753592594197858, 5.484709000965211523 ) ) ;
#52520 = PLANE ( 'NONE',  #9683 ) ;
#52521 = DIRECTION ( 'NONE',  ( 0.000000000000000000, -1.000000000000000000, 0.000000000000000000 ) ) ;
#52522 = ADVANCED_FACE ( 'NONE', ( #27804 ), #14452, .F. ) ;
#52523 = CARTESIAN_POINT ( 'NONE',  ( -10.47421230394850866, 0.000000000000000000, 10.95934586908605723 ) ) ;
#52524 = DIRECTION ( 'NONE',  ( 0.6427681459581294776, -0.7660444431189769032, 0.005002170337467562802 ) ) ;
#52525 = CARTESIAN_POINT ( 'NONE',  ( -7.370172463670563445, -9.191392189769848287, 6.081198852663857402 ) ) ;
#52526 = DIRECTION ( 'NONE',  ( 0.000000000000000000, -1.000000000000000000, 0.000000000000000000 ) ) ;
#52527 = EDGE_CURVE ( 'NONE', #37525, #18912, #31768, .T. ) ;
#52528 = CARTESIAN_POINT ( 'NONE',  ( 2.072287782118878319, 0.000000000000000000, -2.950529333540147015 ) ) ;
#52529 = FILL_AREA_STYLE ('',( #841 ) ) ;
#52530 = ADVANCED_FACE ( 'NONE', ( #13595 ), #53356, .F. ) ;
#52531 = CARTESIAN_POINT ( 'NONE',  ( -9.888614050034579606, -0.1191753592594203132, 7.059447091443916911 ) ) ;
#52532 = ORIENTED_EDGE ( 'NONE', *, *, #16253, .F. ) ;
#52533 = CARTESIAN_POINT ( 'NONE',  ( -20.54126990917373519, -0.1191753592594197858, 4.760553241521720658 ) ) ;
#52534 = CARTESIAN_POINT ( 'NONE',  ( -10.37421533196711465, -0.1191753592594197858, 10.96012406864405975 ) ) ;
#52535 = CARTESIAN_POINT ( 'NONE',  ( -14.83712142277997081, 4.172053068839012724, 2.312063226871277077 ) ) ;
#52536 = EDGE_CURVE ( 'NONE', #50536, #3468, #48221, .T. ) ;
#52537 = DIRECTION ( 'NONE',  ( -0.7660212471507179544, -0.6427876096865405842, -0.005961354470445141482 ) ) ;
#52538 = FACE_OUTER_BOUND ( 'NONE', #45017, .T. ) ;
#52539 = DIRECTION ( 'NONE',  ( 0.9999697198139515519, 0.000000000000000000, 0.007781995580013368816 ) ) ;
#52540 = ORIENTED_EDGE ( 'NONE', *, *, #2169, .F. ) ;
#52541 = ORIENTED_EDGE ( 'NONE', *, *, #923, .T. ) ;
#52542 = DIRECTION ( 'NONE',  ( 0.5449076811759707706, 0.6444004775717708799, -0.5364919789714476250 ) ) ;
#52543 = FACE_OUTER_BOUND ( 'NONE', #18143, .T. ) ;
#52544 = ORIENTED_EDGE ( 'NONE', *, *, #2792, .F. ) ;
#52545 = PLANE ( 'NONE',  #45794 ) ;
#52546 = EDGE_LOOP ( 'NONE', ( #1908, #28484, #24855, #40980 ) ) ;
#52547 = LINE ( 'NONE', #35505, #48339 ) ;
#52548 = ORIENTED_EDGE ( 'NONE', *, *, #10574, .F. ) ;
#52549 = ORIENTED_EDGE ( 'NONE', *, *, #16299, .T. ) ;
#52550 = EDGE_LOOP ( 'NONE', ( #40706, #14405, #22105, #799 ) ) ;
#52551 = CARTESIAN_POINT ( 'NONE',  ( -17.36532418587302473, -0.1191753592594177458, 13.67570816655714516 ) ) ;
#52552 = FACE_OUTER_BOUND ( 'NONE', #10655, .T. ) ;
#52553 = CARTESIAN_POINT ( 'NONE',  ( -16.06709938707323460, 0.000000000000000000, 13.13181314741652628 ) ) ;
#52554 = EDGE_CURVE ( 'NONE', #24619, #37122, #18131, .T. ) ;
#52555 = PRESENTATION_LAYER_ASSIGNMENT (  '', '', ( #46182 ) ) ;
#52556 = LINE ( 'NONE', #44325, #31102 ) ;
#52557 = EDGE_LOOP ( 'NONE', ( #45486, #36197, #8379 ) ) ;
#52559 = EDGE_LOOP ( 'NONE', ( #27159, #54, #37776, #45185 ) ) ;
#52558 = EDGE_CURVE ( 'NONE', #34341, #24350, #43976, .T. ) ;
#52560 = CARTESIAN_POINT ( 'NONE',  ( -19.60834386242827776, 0.000000000000000000, 4.298478389818581213 ) ) ;
#52561 = ORIENTED_EDGE ( 'NONE', *, *, #1849, .F. ) ;
#52562 = LINE ( 'NONE', #13658, #38226 ) ;
#52563 = ORIENTED_EDGE ( 'NONE', *, *, #34073, .F. ) ;
#52564 = FACE_OUTER_BOUND ( 'NONE', #28628, .T. ) ;
#52565 = DIRECTION ( 'NONE',  ( -0.9999697198139514409, -0.000000000000000000, -0.007781995580013368816 ) ) ;
#52566 = EDGE_CURVE ( 'NONE', #34403, #30589, #37138, .T. ) ;
#52567 = ADVANCED_FACE ( 'NONE', ( #23523 ), #32868, .F. ) ;
#52568 = EDGE_CURVE ( 'NONE', #52618, #46492, #23786, .T. ) ;
#52569 = VERTEX_POINT ( 'NONE', #37710 ) ;
#52570 = PLANE ( 'NONE',  #5029 ) ;
#52571 = ORIENTED_EDGE ( 'NONE', *, *, #34808, .F. ) ;
#52572 = EDGE_CURVE ( 'NONE', #17790, #36664, #24353, .T. ) ;
#52573 = CARTESIAN_POINT ( 'NONE',  ( -10.98261119617138526, -1.489407457353158160, 1.099820381026936023 ) ) ;
#52574 = VERTEX_POINT ( 'NONE', #36881 ) ;
#52575 = CARTESIAN_POINT ( 'NONE',  ( -20.58768131384620403, 5.467268677019013978, 4.504451819298203930 ) ) ;
#52576 = CARTESIAN_POINT ( 'NONE',  ( -11.36238454357943084, 0.000000000000000000, 5.670652617570483223 ) ) ;
#52577 = DIRECTION ( 'NONE',  ( 0.5449076811759707706, 0.6444004775717708799, -0.5364919789714476250 ) ) ;
#52578 = ORIENTED_EDGE ( 'NONE', *, *, #7293, .F. ) ;
#52579 = DIRECTION ( 'NONE',  ( 0.000000000000000000, -0.000000000000000000, -1.000000000000000000 ) ) ;
#52580 = PLANE ( 'NONE',  #38299 ) ;
#52581 = CARTESIAN_POINT ( 'NONE',  ( 2.072287782118878319, 0.000000000000000000, -2.950529333540147015 ) ) ;
#52582 = LINE ( 'NONE', #22508, #44996 ) ;
#52583 = LINE ( 'NONE', #13681, #5892 ) ;
#52585 = ADVANCED_FACE ( 'NONE', ( #37399 ), #41115, .F. ) ;
#52584 = DIRECTION ( 'NONE',  ( 0.000000000000000000, -1.000000000000000000, 0.000000000000000000 ) ) ;
#52586 = VECTOR ( 'NONE', #30328, 1000.000000000000227 ) ;
#52587 =( NAMED_UNIT ( * ) PLANE_ANGLE_UNIT ( ) SI_UNIT ( $, .RADIAN. ) );
#52588 = ORIENTED_EDGE ( 'NONE', *, *, #22697, .T. ) ;
#52589 = LINE ( 'NONE', #13685, #53387 ) ;
#52590 = DIRECTION ( 'NONE',  ( 0.9999697198139515519, 0.000000000000000000, 0.007781995580013368816 ) ) ;
#52591 = EDGE_CURVE ( 'NONE', #18181, #52283, #20370, .T. ) ;
#52592 = DIRECTION ( 'NONE',  ( -0.005002170337468016433, -0.7660444431189770143, 0.6427681459581293666 ) ) ;
#52593 = VERTEX_POINT ( 'NONE', #2203 ) ;
#52594 = FACE_OUTER_BOUND ( 'NONE', #50098, .T. ) ;
#52595 = CARTESIAN_POINT ( 'NONE',  ( -19.60990026154428278, 0.000000000000000000, 4.498472333781370125 ) ) ;
#52596 = VERTEX_POINT ( 'NONE', #29161 ) ;
#52597 = PLANE ( 'NONE',  #37974 ) ;
#52598 = EDGE_CURVE ( 'NONE', #18918, #17751, #50747, .T. ) ;
#52599 = CARTESIAN_POINT ( 'NONE',  ( -17.47449301425473323, -1.975113310420658852, 6.711115685826810839 ) ) ;
#52600 = CARTESIAN_POINT ( 'NONE',  ( -11.79859221955444681, 1.095915999411503750, 3.262879877198777034 ) ) ;
#52601 = EDGE_CURVE ( 'NONE', #7109, #43104, #10754, .T. ) ;
#52602 = DIRECTION ( 'NONE',  ( -0.005002170337468016433, -0.7660444431189770143, 0.6427681459581293666 ) ) ;
#52603 = ORIENTED_EDGE ( 'NONE', *, *, #21089, .F. ) ;
#52604 = VERTEX_POINT ( 'NONE', #28625 ) ;
#52605 = DIRECTION ( 'NONE',  ( 0.000000000000000000, -1.000000000000000000, 0.000000000000000000 ) ) ;
#52606 = FACE_OUTER_BOUND ( 'NONE', #6883, .T. ) ;
#52607 = CARTESIAN_POINT ( 'NONE',  ( -23.66772770479517618, 18.99370688441070953, -4.503111145262439052 ) ) ;
#52608 = CARTESIAN_POINT ( 'NONE',  ( -17.30188903097415576, -0.1191753592594164690, 5.524426992162961625 ) ) ;
#52609 = DIRECTION ( 'NONE',  ( 0.9999697198139515519, 0.000000000000000000, 0.007781995580013368816 ) ) ;
#52610 = LINE ( 'NONE', #30774, #31254 ) ;
#52611 = ORIENTED_EDGE ( 'NONE', *, *, #20974, .T. ) ;
#52612 = CARTESIAN_POINT ( 'NONE',  ( -25.20123094555300369, 0.000000000000000000, 6.470945668149052032 ) ) ;
#52613 = FACE_OUTER_BOUND ( 'NONE', #963, .T. ) ;
#52614 = ORIENTED_EDGE ( 'NONE', *, *, #5545, .T. ) ;
#52615 = CARTESIAN_POINT ( 'NONE',  ( -10.74029228357944987, 0.000000000000000000, 11.14194120806293320 ) ) ;
#52616 = DIRECTION ( 'NONE',  ( -0.6427681459581293666, -0.7660444431189770143, -0.005002170337467561935 ) ) ;
#52617 = LINE ( 'NONE', #9768, #5756 ) ;
#52618 = VERTEX_POINT ( 'NONE', #28061 ) ;
#52619 = DIRECTION ( 'NONE',  ( 0.7660212471507180654, -0.6427876096865404731, 0.005961354470445141482 ) ) ;
#52620 = ORIENTED_EDGE ( 'NONE', *, *, #36974, .F. ) ;
#52621 = VECTOR ( 'NONE', #35664, 1000.000000000000227 ) ;
#52622 = EDGE_LOOP ( 'NONE', ( #8036, #4876, #23014, #16311 ) ) ;
#52623 = ORIENTED_EDGE ( 'NONE', *, *, #15966, .T. ) ;
#52624 = ORIENTED_EDGE ( 'NONE', *, *, #33762, .F. ) ;
#52625 = DIRECTION ( 'NONE',  ( 0.005961354470445682716, -0.6427876096865404731, -0.7660212471507180654 ) ) ;
#52626 = ORIENTED_EDGE ( 'NONE', *, *, #46747, .T. ) ;
#52627 = CARTESIAN_POINT ( 'NONE',  ( -17.30476308447943978, -0.1191753592594171213, 5.893736695420727756 ) ) ;
#52628 = EDGE_CURVE ( 'NONE', #41034, #36178, #50489, .T. ) ;
#52629 = ORIENTED_EDGE ( 'NONE', *, *, #23206, .T. ) ;
#52630 = DIRECTION ( 'NONE',  ( -0.5449076811759708816, 0.6444004775717707689, 0.5364919789714475140 ) ) ;
#52631 = ORIENTED_EDGE ( 'NONE', *, *, #46164, .T. ) ;
#52632 = DIRECTION ( 'NONE',  ( -0.005961354470445682716, -0.6427876096865404731, 0.7660212471507180654 ) ) ;
#52633 = ORIENTED_EDGE ( 'NONE', *, *, #6960, .F. ) ;
#52634 = EDGE_CURVE ( 'NONE', #10990, #40728, #15286, .T. ) ;
#52635 = EDGE_CURVE ( 'NONE', #21963, #32592, #32598, .T. ) ;
#52636 = CARTESIAN_POINT ( 'NONE',  ( -21.47341775636118655, -0.1191753592594197858, 5.122631121243466090 ) ) ;
#52637 = DIRECTION ( 'NONE',  ( -0.7660212471507179544, -0.6427876096865405842, -0.005961354470445141482 ) ) ;
#52638 = DIRECTION ( 'NONE',  ( 0.9999697198139515519, 0.000000000000000000, 0.007781995580013368816 ) ) ;
#52639 = LINE ( 'NONE', #27949, #13015 ) ;
#52640 = DIRECTION ( 'NONE',  ( -0.2426528472758541499, 0.7422098413412800966, -0.6246952433987894571 ) ) ;
#52641 = DIRECTION ( 'NONE',  ( 0.005002170337468016433, -0.7660444431189770143, -0.6427681459581293666 ) ) ;
#52642 = ORIENTED_EDGE ( 'NONE', *, *, #25020, .T. ) ;
#52643 = ORIENTED_EDGE ( 'NONE', *, *, #40743, .F. ) ;
#52644 = DIRECTION ( 'NONE',  ( 0.000000000000000000, -1.000000000000000000, 0.000000000000000000 ) ) ;
#52645 = DIRECTION ( 'NONE',  ( 0.000000000000000000, -0.000000000000000000, -1.000000000000000000 ) ) ;
#52646 = LINE ( 'NONE', #44689, #7957 ) ;
#52647 = LINE ( 'NONE', #43857, #16726 ) ;
#52648 = VERTEX_POINT ( 'NONE', #3038 ) ;
#52649 = CARTESIAN_POINT ( 'NONE',  ( -12.26710951010334405, 0.000000000000000000, 2.508949224009560108 ) ) ;
#52650 = LINE ( 'NONE', #43575, #48635 ) ;
#52651 = ORIENTED_EDGE ( 'NONE', *, *, #50465, .F. ) ;
#52652 = DIRECTION ( 'NONE',  ( 0.000000000000000000, -0.000000000000000000, -1.000000000000000000 ) ) ;
#52653 = CARTESIAN_POINT ( 'NONE',  ( -16.33317936670417225, 0.000000000000000000, 13.31440848639340224 ) ) ;
#52654 = EDGE_LOOP ( 'NONE', ( #54336, #9482, #9120, #22549 ) ) ;
#52655 = CARTESIAN_POINT ( 'NONE',  ( -66.99903215919390220, -8.772469562030201118, -3.320464512871846186 ) ) ;
#52656 = CARTESIAN_POINT ( 'NONE',  ( -58.00000000000000711, -8.999999999999998224, 7.102951435054649637E-15 ) ) ;
#52657 = VECTOR ( 'NONE', #41731, 1000.000000000000114 ) ;
#52658 = CARTESIAN_POINT ( 'NONE',  ( -10.27421835998572064, 0.000000000000000000, 10.96090226820206048 ) ) ;
#52659 = EDGE_CURVE ( 'NONE', #394, #29284, #45643, .T. ) ;
#52660 = DIRECTION ( 'NONE',  ( 0.000000000000000000, -0.000000000000000000, -1.000000000000000000 ) ) ;
#52661 = VECTOR ( 'NONE', #39183, 999.9999999999998863 ) ;
#52662 = CARTESIAN_POINT ( 'NONE',  ( -32.47108885958310509, -1.000000000000000000, 15.83124721154520387 ) ) ;
#52663 = ORIENTED_EDGE ( 'NONE', *, *, #1512, .T. ) ;
#52664 = ADVANCED_FACE ( 'NONE', ( #7304 ), #6220, .F. ) ;
#52665 = VERTEX_POINT ( 'NONE', #33443 ) ;
#52666 = FACE_OUTER_BOUND ( 'NONE', #35528, .T. ) ;
#52667 = CARTESIAN_POINT ( 'NONE',  ( -16.06709938707323460, 0.000000000000000000, 13.13181314741652628 ) ) ;
#52668 = PLANE ( 'NONE',  #14319 ) ;
#52669 = FACE_OUTER_BOUND ( 'NONE', #38461, .T. ) ;
#52670 = EDGE_CURVE ( 'NONE', #39202, #27276, #1913, .T. ) ;
#52671 = CARTESIAN_POINT ( 'NONE',  ( 5.551076178010876383, -1.058033593491026769, -2.420903799066405071 ) ) ;
#52672 = ORIENTED_EDGE ( 'NONE', *, *, #38642, .T. ) ;
#52673 = CARTESIAN_POINT ( 'NONE',  ( -16.79925329029790149, 0.000000000000000000, 13.49544742625427496 ) ) ;
#52674 = CARTESIAN_POINT ( 'NONE',  ( -21.47341775636118655, -0.1191753592594197858, 5.122631121243466090 ) ) ;
#52675 = DIRECTION ( 'NONE',  ( -0.005961354470445682716, -0.6427876096865404731, 0.7660212471507180654 ) ) ;
#52676 = CARTESIAN_POINT ( 'NONE',  ( -12.15116108492864377, 0.000000000000000000, 1.401855352044617975 ) ) ;
#52677 = ORIENTED_EDGE ( 'NONE', *, *, #48812, .F. ) ;
#52678 = CARTESIAN_POINT ( 'NONE',  ( -15.50810134761786507, -2.946525016555658905, 7.541554487265736739 ) ) ;
#52679 = VERTEX_POINT ( 'NONE', #45367 ) ;
#52680 = LINE ( 'NONE', #43604, #52218 ) ;
#52681 = CARTESIAN_POINT ( 'NONE',  ( 2.072287782118878319, 0.000000000000000000, -2.950529333540147015 ) ) ;
#52682 = ORIENTED_EDGE ( 'NONE', *, *, #28692, .T. ) ;
#52683 = VECTOR ( 'NONE', #35788, 1000.000000000000227 ) ;
#52684 = VECTOR ( 'NONE', #39216, 999.9999999999998863 ) ;
#52685 = LINE ( 'NONE', #13788, #15411 ) ;
#52686 = VERTEX_POINT ( 'NONE', #41410 ) ;
#52687 = EDGE_LOOP ( 'NONE', ( #3941, #18034, #43552, #23324 ) ) ;
#52688 = ORIENTED_EDGE ( 'NONE', *, *, #44745, .F. ) ;
#52689 = CARTESIAN_POINT ( 'NONE',  ( -25.20278734466900517, 0.000000000000000000, 6.670939612111840944 ) ) ;
#52690 = ORIENTED_EDGE ( 'NONE', *, *, #46363, .F. ) ;
#52691 = ORIENTED_EDGE ( 'NONE', *, *, #30894, .F. ) ;
#52692 = DIRECTION ( 'NONE',  ( 0.9999697198139515519, 0.000000000000000000, 0.007781995580013368816 ) ) ;
#52693 = ADVANCED_FACE ( 'NONE', ( #2497 ), #19817, .F. ) ;
#52694 = DIRECTION ( 'NONE',  ( 0.007781995580012662783, 0.000000000000000000, -0.9999697198139514409 ) ) ;
#52695 = VERTEX_POINT ( 'NONE', #52163 ) ;
#52696 = ADVANCED_FACE ( 'NONE', ( #34550 ), #168, .F. ) ;
#52697 = VECTOR ( 'NONE', #9340, 1000.000000000000000 ) ;
#52698 = EDGE_LOOP ( 'NONE', ( #6911, #9264, #53068, #35311 ) ) ;
#52699 = CARTESIAN_POINT ( 'NONE',  ( -16.85908992509638082, 5.467268677019013090, 3.056140300411222643 ) ) ;
#52700 = VERTEX_POINT ( 'NONE', #34008 ) ;
#52701 = ORIENTED_EDGE ( 'NONE', *, *, #38472, .F. ) ;
#52702 = ADVANCED_FACE ( 'NONE', ( #3614 ), #51332, .F. ) ;
#52703 = VECTOR ( 'NONE', #37433, 999.9999999999998863 ) ;
#52704 = PLANE ( 'NONE',  #25769 ) ;
#52705 = DIRECTION ( 'NONE',  ( -0.5449076811759708816, 0.6444004775717707689, 0.5364919789714475140 ) ) ;
#52706 = DIRECTION ( 'NONE',  ( -0.6246952433987894571, 0.7422098413412802076, 0.2426528472758539834 ) ) ;
#52707 = VERTEX_POINT ( 'NONE', #21520 ) ;
#52708 = LINE ( 'NONE', #22368, #37368 ) ;
#52709 = EDGE_LOOP ( 'NONE', ( #18180, #36731, #5320, #55637 ) ) ;
#52710 = CARTESIAN_POINT ( 'NONE',  ( -16.79056226515798045, -2.298917212465660054, 3.329998215632909986 ) ) ;
#52711 = ADVANCED_FACE ( 'NONE', ( #21778 ), #16976, .F. ) ;
#52712 = CARTESIAN_POINT ( 'NONE',  ( -15.07792331919211293, 0.000000000000000000, 5.441731379463618623 ) ) ;
#52713 = DIRECTION ( 'NONE',  ( -0.6427681459581293666, -0.7660444431189770143, -0.005002170337467561935 ) ) ;
#52714 = CARTESIAN_POINT ( 'NONE',  ( -14.87792937522932668, 0.000000000000000000, 5.443287778579622760 ) ) ;
#52715 = CARTESIAN_POINT ( 'NONE',  ( -13.60775715277214637, -0.1191753592594198830, 8.504088575178599285 ) ) ;
#52716 = DIRECTION ( 'NONE',  ( -0.7660212471507179544, -0.6427876096865405842, -0.005961354470445141482 ) ) ;
#52717 = CARTESIAN_POINT ( 'NONE',  ( -23.33771345073609638, -0.1191753592594197858, 5.846786880686956955 ) ) ;
#52718 = ORIENTED_EDGE ( 'NONE', *, *, #25034, .T. ) ;
#52719 = CARTESIAN_POINT ( 'NONE',  ( -14.20280369269832832, 0.000000000000000000, 12.40765738797303719 ) ) ;
#52720 = PRODUCT_DEFINITION_SHAPE ( 'NONE', 'NONE',  #56241 ) ;
#52721 = VECTOR ( 'NONE', #1888, 1000.000000000000227 ) ;
#52722 = AXIS2_PLACEMENT_3D ( 'NONE', #3678, #13349, #56205 ) ;
#52723 = CARTESIAN_POINT ( 'NONE',  ( -9.442067484779661513, -0.1191753592594197858, 10.59804618892231254 ) ) ;
#52724 = PLANE ( 'NONE',  #12415 ) ;
#52725 = CARTESIAN_POINT ( 'NONE',  ( -4.546219555552018399, 7.433331870878916448, -1.452467510021419717 ) ) ;
#52726 = CARTESIAN_POINT ( 'NONE',  ( -15.46945900645201100, 21.99492871671912653, -3.969181436210386771 ) ) ;
#52727 = DIRECTION ( 'NONE',  ( 0.005002170337468016433, -0.7660444431189770143, -0.6427681459581293666 ) ) ;
#52728 = LINE ( 'NONE', #26927, #38643 ) ;
#52729 = FACE_OUTER_BOUND ( 'NONE', #14648, .T. ) ;
#52730 = VECTOR ( 'NONE', #14079, 999.9999999999998863 ) ;
#52731 = VERTEX_POINT ( 'NONE', #16673 ) ;
#52732 = CARTESIAN_POINT ( 'NONE',  ( -19.05546973890454154, 0.000000000000000000, 4.872119110114796925 ) ) ;
#52733 = FACE_OUTER_BOUND ( 'NONE', #48592, .T. ) ;
#52734 = DIRECTION ( 'NONE',  ( 0.000000000000000000, -1.000000000000000000, 0.000000000000000000 ) ) ;
#52735 = DIRECTION ( 'NONE',  ( 0.9999697198139515519, 0.000000000000000000, 0.007781995580013368816 ) ) ;
#52736 = EDGE_CURVE ( 'NONE', #52707, #32780, #47627, .T. ) ;
#52737 = CARTESIAN_POINT ( 'NONE',  ( -11.13784177245837981, 0.000000000000000000, 2.517737446661582723 ) ) ;
#52738 = DIRECTION ( 'NONE',  ( 0.007781995580012663651, -3.146120232559066537E-19, -0.9999697198139514409 ) ) ;
#52739 = DIRECTION ( 'NONE',  ( -0.5449076811759708816, 0.6444004775717707689, 0.5364919789714475140 ) ) ;
#52740 = AXIS2_PLACEMENT_3D ( 'NONE', #48815, #13342, #49072 ) ;
#52741 = DIRECTION ( 'NONE',  ( 0.007781995580012663651, 0.000000000000000000, -0.9999697198139515519 ) ) ;
#52742 = LINE ( 'NONE', #52484, #3844 ) ;
#52743 = EDGE_CURVE ( 'NONE', #27886, #34394, #29763, .T. ) ;
#52744 = VERTEX_POINT ( 'NONE', #8164 ) ;
#52745 = ADVANCED_FACE ( 'NONE', ( #55874 ), #47326, .F. ) ;
#52746 = ADVANCED_FACE ( 'NONE', ( #55567 ), #4470, .F. ) ;
#52747 = ORIENTED_EDGE ( 'NONE', *, *, #31239, .F. ) ;
#52748 = VERTEX_POINT ( 'NONE', #7592 ) ;
#52749 = EDGE_LOOP ( 'NONE', ( #45307, #15480, #2484, #24961 ) ) ;
#52750 = ORIENTED_EDGE ( 'NONE', *, *, #89, .T. ) ;
#52751 = DIRECTION ( 'NONE',  ( 0.000000000000000000, -0.000000000000000000, -1.000000000000000000 ) ) ;
#52752 = EDGE_CURVE ( 'NONE', #1154, #54036, #8746, .T. ) ;
#52753 = DIRECTION ( 'NONE',  ( 0.000000000000000000, -0.000000000000000000, -1.000000000000000000 ) ) ;
#52754 = VECTOR ( 'NONE', #26780, 999.9999999999998863 ) ;
#52755 = VECTOR ( 'NONE', #11988, 1000.000000000000000 ) ;
#52757 = EDGE_CURVE ( 'NONE', #47190, #16329, #14776, .T. ) ;
#52756 = ORIENTED_EDGE ( 'NONE', *, *, #37201, .T. ) ;
#52758 = ORIENTED_EDGE ( 'NONE', *, *, #16667, .T. ) ;
#52759 = ADVANCED_FACE ( 'NONE', ( #34296 ), #30307, .T. ) ;
#52760 = VECTOR ( 'NONE', #25291, 1000.000000000000227 ) ;
#52761 = DIRECTION ( 'NONE',  ( 0.9999697198139515519, 0.000000000000000000, 0.007781995580013368816 ) ) ;
#52762 = ORIENTED_EDGE ( 'NONE', *, *, #23913, .T. ) ;
#52763 = LINE ( 'NONE', #44818, #28261 ) ;
#52764 = DIRECTION ( 'NONE',  ( 0.007781995580012663651, -3.146120232559066537E-19, -0.9999697198139514409 ) ) ;
#52765 = VERTEX_POINT ( 'NONE', #42245 ) ;
#52766 = DIRECTION ( 'NONE',  ( -0.6427681459581293666, -0.7660444431189770143, -0.005002170337467561935 ) ) ;
#52767 = EDGE_CURVE ( 'NONE', #53756, #38710, #26063, .T. ) ;
#52768 = ORIENTED_EDGE ( 'NONE', *, *, #3204, .F. ) ;
#52769 = DIRECTION ( 'NONE',  ( 0.007781995580012663651, 0.000000000000000000, -0.9999697198139515519 ) ) ;
#52770 = VECTOR ( 'NONE', #32346, 999.9999999999998863 ) ;
#52771 = CARTESIAN_POINT ( 'NONE',  ( -24.27063949748155380, 0.000000000000000000, 6.308861732390097288 ) ) ;
#52772 = VECTOR ( 'NONE', #23399, 999.9999999999998863 ) ;
#52773 = EDGE_CURVE ( 'NONE', #10380, #16523, #45730, .T. ) ;
#52774 = LINE ( 'NONE', #44533, #28218 ) ;
#52775 = DIRECTION ( 'NONE',  ( 0.9999697198139515519, 0.000000000000000000, 0.007781995580013368816 ) ) ;
#52776 = ORIENTED_EDGE ( 'NONE', *, *, #9372, .F. ) ;
#52777 = DIRECTION ( 'NONE',  ( -0.7660212471507179544, -0.6427876096865405842, -0.005961354470445141482 ) ) ;
#52778 = LINE ( 'NONE', #14461, #22022 ) ;
#52779 = CARTESIAN_POINT ( 'NONE',  ( -19.78282706061121132, 0.000000000000000000, 6.713118996285826867 ) ) ;
#52780 = EDGE_LOOP ( 'NONE', ( #29483, #39511, #28684, #52443 ) ) ;
#52781 = CARTESIAN_POINT ( 'NONE',  ( -11.24436505100834260, -0.1191753592594186895, 3.355575625600500711 ) ) ;
#52782 = VERTEX_POINT ( 'NONE', #30857 ) ;
#52783 = DIRECTION ( 'NONE',  ( -0.6427681459581293666, -0.7660444431189770143, -0.005002170337467561935 ) ) ;
#52784 = CARTESIAN_POINT ( 'NONE',  ( -14.00280974873554030, 0.000000000000000000, 12.40921378708904044 ) ) ;
#52785 = FACE_OUTER_BOUND ( 'NONE', #30782, .T. ) ;
#52786 = CARTESIAN_POINT ( 'NONE',  ( -14.88942558925045745, 0.000000000000000000, 6.920526591610678402 ) ) ;
#52787 = VECTOR ( 'NONE', #15193, 1000.000000000000227 ) ;
#52788 = DIRECTION ( 'NONE',  ( 0.007781995580012663651, 0.000000000000000000, -0.9999697198139515519 ) ) ;
#52789 = CARTESIAN_POINT ( 'NONE',  ( 2.072287782118878319, 0.000000000000000000, -2.950529333540147015 ) ) ;
#52790 = DIRECTION ( 'NONE',  ( 0.7660212471507180654, -0.6427876096865404731, 0.005961354470445141482 ) ) ;
#52791 = PLANE ( 'NONE',  #29295 ) ;
#52792 = DIRECTION ( 'NONE',  ( 1.007958083594381669E-15, -3.869188571150966625E-16, 1.000000000000000000 ) ) ;
#52793 = ORIENTED_EDGE ( 'NONE', *, *, #23438, .F. ) ;
#52794 = AXIS2_PLACEMENT_3D ( 'NONE', #41143, #18442, #44554 ) ;
#52795 = DIRECTION ( 'NONE',  ( 0.007781995580012663651, -3.146120232559066537E-19, -0.9999697198139514409 ) ) ;
#52796 = FACE_OUTER_BOUND ( 'NONE', #15767, .T. ) ;
#52797 = DIRECTION ( 'NONE',  ( 0.005961354470445682716, -0.6427876096865404731, -0.7660212471507180654 ) ) ;
#52798 = LINE ( 'NONE', #48562, #52252 ) ;
#52799 = CIRCLE ( 'NONE', #18307, 6.000000000000002665 ) ;
#52800 = VECTOR ( 'NONE', #41678, 1000.000000000000000 ) ;
#52801 = CARTESIAN_POINT ( 'NONE',  ( -17.74560456716937296, 0.000000000000000000, 3.774316574337878372 ) ) ;
#52802 = EDGE_CURVE ( 'NONE', #3819, #43814, #18079, .T. ) ;
#52803 = DIRECTION ( 'NONE',  ( 0.000000000000000000, -1.000000000000000000, 0.000000000000000000 ) ) ;
#52804 = DIRECTION ( 'NONE',  ( 0.007781995580012662783, 0.000000000000000000, -0.9999697198139514409 ) ) ;
#52805 = ORIENTED_EDGE ( 'NONE', *, *, #3756, .T. ) ;
#52806 = VECTOR ( 'NONE', #7878, 999.9999999999998863 ) ;
#52807 = VECTOR ( 'NONE', #55367, 999.9999999999998863 ) ;
#52808 = VERTEX_POINT ( 'NONE', #53004 ) ;
#52809 = DIRECTION ( 'NONE',  ( -0.5364919789714478471, 0.6444004775717705469, -0.5449076811759709926 ) ) ;
#52810 = CARTESIAN_POINT ( 'NONE',  ( 0.1285714285714296967, 2.000000000000000000, 5.998622290806041590 ) ) ;
#52811 = EDGE_CURVE ( 'NONE', #49206, #24901, #22057, .T. ) ;
#52812 = ORIENTED_EDGE ( 'NONE', *, *, #45451, .F. ) ;
#52813 = CARTESIAN_POINT ( 'NONE',  ( -27.99767448711536133, 0.000000000000000000, 7.557179307314289218 ) ) ;
#52814 = VECTOR ( 'NONE', #38470, 1000.000000000000227 ) ;
#52815 = ORIENTED_EDGE ( 'NONE', *, *, #12276, .F. ) ;
#52816 = LINE ( 'NONE', #18464, #33833 ) ;
#52817 = EDGE_CURVE ( 'NONE', #40480, #2840, #14119, .T. ) ;
#52818 = ORIENTED_EDGE ( 'NONE', *, *, #43235, .F. ) ;
#52819 = ORIENTED_EDGE ( 'NONE', *, *, #26882, .F. ) ;
#52820 = ORIENTED_EDGE ( 'NONE', *, *, #38781, .T. ) ;
#52821 = LINE ( 'NONE', #40340, #5766 ) ;
#52822 = CARTESIAN_POINT ( 'NONE',  ( 2.072287782118878319, 0.000000000000000000, -2.950529333540147015 ) ) ;
#52823 = CARTESIAN_POINT ( 'NONE',  ( -13.29462968114988897, -0.3560938001956550081, 2.430427978987968807 ) ) ;
#52824 = LINE ( 'NONE', #22738, #6620 ) ;
#52825 = ADVANCED_FACE ( 'NONE', ( #31446 ), #5575, .F. ) ;
#52826 = ORIENTED_EDGE ( 'NONE', *, *, #44914, .T. ) ;
#52827 = ORIENTED_EDGE ( 'NONE', *, *, #19636, .T. ) ;
#52828 = VECTOR ( 'NONE', #15436, 999.9999999999998863 ) ;
#52829 = EDGE_CURVE ( 'NONE', #10480, #29513, #48761, .T. ) ;
#52830 = CARTESIAN_POINT ( 'NONE',  ( -28.93137873341882127, 0.000000000000000000, 8.119251130998824451 ) ) ;
#52831 = ORIENTED_EDGE ( 'NONE', *, *, #10544, .F. ) ;
#52832 = AXIS2_PLACEMENT_3D ( 'NONE', #34460, #38744, #11757 ) ;
#52833 = DIRECTION ( 'NONE',  ( -0.005002170337468016433, -0.7660444431189770143, 0.6427681459581293666 ) ) ;
#52834 = VERTEX_POINT ( 'NONE', #53306 ) ;
#52835 = DIRECTION ( 'NONE',  ( -2.551063935260010306E-17, 4.081702296416016490E-16, -1.000000000000000000 ) ) ;
#52836 = FACE_OUTER_BOUND ( 'NONE', #21027, .T. ) ;
#52837 = VECTOR ( 'NONE', #55003, 1000.000000000000227 ) ;
#52838 = ADVANCED_FACE ( 'NONE', ( #23198 ), #40528, .F. ) ;
#52839 = AXIS2_PLACEMENT_3D ( 'NONE', #54983, #15247, #16078 ) ;
#52840 = VERTEX_POINT ( 'NONE', #14402 ) ;
#52841 = CARTESIAN_POINT ( 'NONE',  ( -13.73672976910459909, 0.000000000000000000, 12.22661844811216270 ) ) ;
#52842 = ORIENTED_EDGE ( 'NONE', *, *, #528, .F. ) ;
#52843 = EDGE_CURVE ( 'NONE', #15160, #26242, #9269, .T. ) ;
#52844 = VECTOR ( 'NONE', #34214, 1000.000000000000227 ) ;
#52845 = DIRECTION ( 'NONE',  ( 0.000000000000000000, -0.000000000000000000, -1.000000000000000000 ) ) ;
#52846 = VECTOR ( 'NONE', #5334, 999.9999999999998863 ) ;
#52847 = VERTEX_POINT ( 'NONE', #44470 ) ;
#52848 = CARTESIAN_POINT ( 'NONE',  ( -11.83983530883092961, 0.000000000000000000, 7.313591278128507511 ) ) ;
#52849 = LINE ( 'NONE', #44602, #36598 ) ;
#52850 = CARTESIAN_POINT ( 'NONE',  ( -11.40636015113596180, 0.000000000000000000, 11.32142374880780089 ) ) ;
#52851 = ORIENTED_EDGE ( 'NONE', *, *, #35348, .T. ) ;
#52852 = CARTESIAN_POINT ( 'NONE',  ( -12.28016212324047807, 0.000000000000000000, 4.186181981003405994 ) ) ;
#52853 = LINE ( 'NONE', #31842, #44616 ) ;
#52854 = LINE ( 'NONE', #13962, #43033 ) ;
#52855 = VECTOR ( 'NONE', #2508, 1000.000000000000227 ) ;
#52856 = DIRECTION ( 'NONE',  ( 0.000000000000000000, -1.000000000000000000, 0.000000000000000000 ) ) ;
#52857 = AXIS2_PLACEMENT_3D ( 'NONE', #23714, #9561, #53296 ) ;
#52858 = FACE_OUTER_BOUND ( 'NONE', #35901, .T. ) ;
#52859 = CARTESIAN_POINT ( 'NONE',  ( -17.20111385943475923, 0.000000000000000000, 5.425208219739572790 ) ) ;
#52860 = LINE ( 'NONE', #47797, #39437 ) ;
#52861 = ORIENTED_EDGE ( 'NONE', *, *, #7629, .T. ) ;
#52862 = FACE_OUTER_BOUND ( 'NONE', #13869, .T. ) ;
#52863 = LINE ( 'NONE', #902, #29526 ) ;
#52864 = LINE ( 'NONE', #43784, #5150 ) ;
#52865 = ORIENTED_EDGE ( 'NONE', *, *, #43402, .F. ) ;
#52866 = CARTESIAN_POINT ( 'NONE',  ( -18.78942900545214201, -0.04243879960735808671, 9.270562878879108126 ) ) ;
#52867 = LINE ( 'NONE', #21930, #24527 ) ;
#52868 = EDGE_LOOP ( 'NONE', ( #40191, #8210, #11689, #8264 ) ) ;
#52869 = EDGE_CURVE ( 'NONE', #31317, #16382, #39388, .T. ) ;
#52870 = VECTOR ( 'NONE', #39870, 999.9999999999998863 ) ;
#52871 = DIRECTION ( 'NONE',  ( 1.000000000000000000, 0.000000000000000000, 0.000000000000000000 ) ) ;
#52872 = LINE ( 'NONE', #35863, #54750 ) ;
#52873 = EDGE_CURVE ( 'NONE', #32323, #9930, #13544, .T. ) ;
#52874 = VECTOR ( 'NONE', #25306, 1000.000000000000227 ) ;
#52875 = DIRECTION ( 'NONE',  ( 0.007781995580012663651, 0.000000000000000000, -0.9999697198139515519 ) ) ;
#52876 = CARTESIAN_POINT ( 'NONE',  ( -7.883669827136422725, -9.688797144239941872, 6.280658667077863022 ) ) ;
#52877 = ORIENTED_EDGE ( 'NONE', *, *, #42575, .T. ) ;
#52878 = ORIENTED_EDGE ( 'NONE', *, *, #48145, .F. ) ;
#52879 = ADVANCED_FACE ( 'NONE', ( #17822 ), #43626, .F. ) ;
#52880 = DIRECTION ( 'NONE',  ( -0.005961354470445682716, -0.6427876096865404731, 0.7660212471507180654 ) ) ;
#52881 = LINE ( 'NONE', #13993, #18678 ) ;
#52882 = VECTOR ( 'NONE', #44032, 999.9999999999998863 ) ;
#52883 = CARTESIAN_POINT ( 'NONE',  ( -67.50810339439870233, 2.000000000000000000, 7.448312483692316022 ) ) ;
#52884 = EDGE_CURVE ( 'NONE', #37965, #32796, #40223, .T. ) ;
#52885 = ADVANCED_FACE ( 'NONE', ( #22628 ), #10118, .F. ) ;
#52886 = EDGE_CURVE ( 'NONE', #2632, #14570, #30607, .T. ) ;
#52887 = VECTOR ( 'NONE', #17959, 1000.000000000000227 ) ;
#52888 = FACE_OUTER_BOUND ( 'NONE', #28260, .T. ) ;
#52889 = CIRCLE ( 'NONE', #47458, 2.125000000000000000 ) ;
#52890 = CARTESIAN_POINT ( 'NONE',  ( -17.70012898643225085, -2.784623065533160524, 8.127303779802742767 ) ) ;
#52891 = DIRECTION ( 'NONE',  ( 0.000000000000000000, -0.000000000000000000, -1.000000000000000000 ) ) ;
#52892 = ORIENTED_EDGE ( 'NONE', *, *, #5092, .T. ) ;
#52893 = CARTESIAN_POINT ( 'NONE',  ( -32.65919192261063841, -0.1191753592594197858, 9.467565677904410393 ) ) ;
#52894 = AXIS2_PLACEMENT_3D ( 'NONE', #37834, #50603, #41773 ) ;
#52895 = CARTESIAN_POINT ( 'NONE',  ( -13.53673582514181106, 0.000000000000000000, 12.22817484722816772 ) ) ;
#52896 = AXIS2_PLACEMENT_3D ( 'NONE', #10839, #3439, #15369 ) ;
#52897 = ORIENTED_EDGE ( 'NONE', *, *, #5747, .F. ) ;
#52898 = FACE_OUTER_BOUND ( 'NONE', #19591, .T. ) ;
#52899 = FACE_OUTER_BOUND ( 'NONE', #12899, .T. ) ;
#52900 = LINE ( 'NONE', #31337, #22975 ) ;
#52901 = ORIENTED_EDGE ( 'NONE', *, *, #47021, .T. ) ;
#52902 = DIRECTION ( 'NONE',  ( -0.6427681459581293666, -0.7660444431189770143, -0.005002170337467561935 ) ) ;
#52903 = EDGE_CURVE ( 'NONE', #54093, #47959, #43912, .T. ) ;
#52904 = ORIENTED_EDGE ( 'NONE', *, *, #53113, .F. ) ;
#52905 = EDGE_CURVE ( 'NONE', #48904, #17751, #44219, .T. ) ;
#52907 = VERTEX_POINT ( 'NONE', #2971 ) ;
#52906 = EDGE_CURVE ( 'NONE', #25423, #52707, #41049, .T. ) ;
#52908 = ORIENTED_EDGE ( 'NONE', *, *, #12822, .T. ) ;
#52909 = EDGE_CURVE ( 'NONE', #16557, #11724, #2438, .T. ) ;
#52910 = VERTEX_POINT ( 'NONE', #6170 ) ;
#52911 = CARTESIAN_POINT ( 'NONE',  ( -68.01236371044051054, -8.487308885305189676, 5.059064008999122564 ) ) ;
#52912 = ORIENTED_EDGE ( 'NONE', *, *, #25465, .F. ) ;
#52913 = VECTOR ( 'NONE', #10420, 1000.000000000000227 ) ;
#52914 = CARTESIAN_POINT ( 'NONE',  ( -18.29747203306047609, -0.1191753592594177458, 14.03778604627889059 ) ) ;
#52915 = DIRECTION ( 'NONE',  ( 0.7660212471507180654, -0.6427876096865404731, 0.005961354470445141482 ) ) ;
#52916 = EDGE_CURVE ( 'NONE', #32990, #2010, #6422, .T. ) ;
#52917 = EDGE_LOOP ( 'NONE', ( #27722, #6277, #7674, #44694 ) ) ;
#52918 = CARTESIAN_POINT ( 'NONE',  ( -23.33771345073609638, -0.1191753592594197858, 5.846786880686956955 ) ) ;
#52919 = ORIENTED_EDGE ( 'NONE', *, *, #16304, .F. ) ;
#52920 = DIRECTION ( 'NONE',  ( 0.5364919789714477361, 0.6444004775717706579, 0.5449076811759711036 ) ) ;
#52921 = AXIS2_PLACEMENT_3D ( 'NONE', #17333, #39504, #55986 ) ;
#52922 = ORIENTED_EDGE ( 'NONE', *, *, #48425, .F. ) ;
#52923 = EDGE_CURVE ( 'NONE', #21379, #6407, #37339, .T. ) ;
#52924 = DIRECTION ( 'NONE',  ( -0.005002170337468016433, -0.7660444431189770143, 0.6427681459581293666 ) ) ;
#52925 = CARTESIAN_POINT ( 'NONE',  ( -17.74404816805336793, 0.000000000000000000, 3.574322630375089460 ) ) ;
#52926 = CARTESIAN_POINT ( 'NONE',  ( -14.88337611868230326, -0.03228989815065527041, 2.661499626451061751 ) ) ;
#52927 = CARTESIAN_POINT ( 'NONE',  ( -17.40841230952411323, 0.000000000000000000, 6.362265171101888939 ) ) ;
#52928 = DIRECTION ( 'NONE',  ( 0.007781995580012663651, -3.146120232559066537E-19, -0.9999697198139514409 ) ) ;
#52929 = VECTOR ( 'NONE', #46385, 1000.000000000000227 ) ;
#52930 = DIRECTION ( 'NONE',  ( -0.005002170337468016433, -0.7660444431189770143, 0.6427681459581293666 ) ) ;
#52931 = ORIENTED_EDGE ( 'NONE', *, *, #31695, .T. ) ;
#52932 = AXIS2_PLACEMENT_3D ( 'NONE', #31905, #19114, #27359 ) ;
#52933 = VECTOR ( 'NONE', #17847, 1000.000000000000227 ) ;
#52934 = ORIENTED_EDGE ( 'NONE', *, *, #54583, .F. ) ;
#52935 = CARTESIAN_POINT ( 'NONE',  ( -12.28591023025104079, 0.000000000000000000, 4.924801387518935591 ) ) ;
#52936 = CARTESIAN_POINT ( 'NONE',  ( -16.74952957573080425, 0.000000000000000000, 7.106056888501429469 ) ) ;
#52937 = LINE ( 'NONE', #18582, #13394 ) ;
#52938 = VECTOR ( 'NONE', #8494, 1000.000000000000227 ) ;
#52939 = AXIS2_PLACEMENT_3D ( 'NONE', #36913, #54462, #45976 ) ;
#52940 = LINE ( 'NONE', #48110, #33068 ) ;
#52941 = ORIENTED_EDGE ( 'NONE', *, *, #13384, .T. ) ;
#52942 = DIRECTION ( 'NONE',  ( 0.9999697198139515519, 0.000000000000000000, 0.007781995580013368816 ) ) ;
#52943 = CARTESIAN_POINT ( 'NONE',  ( -16.25513951096779053, 3.038739411681507185, 8.182458397572339948 ) ) ;
#52944 = ORIENTED_EDGE ( 'NONE', *, *, #16034, .T. ) ;
#52945 = LINE ( 'NONE', #13758, #11176 ) ;
#52946 = LINE ( 'NONE', #48968, #37637 ) ;
#52947 = EDGE_LOOP ( 'NONE', ( #6468, #52701, #51978, #117 ) ) ;
#52948 = CARTESIAN_POINT ( 'NONE',  ( -21.47419595591918906, 0.000000000000000000, 5.222628093224860102 ) ) ;
#52949 = LINE ( 'NONE', #15189, #49621 ) ;
#52950 = DIRECTION ( 'NONE',  ( 0.000000000000000000, 1.000000000000000000, 0.000000000000000000 ) ) ;
#52951 = DIRECTION ( 'NONE',  ( 0.005002170337468016433, -0.7660444431189770143, -0.6427681459581293666 ) ) ;
#52952 = FACE_OUTER_BOUND ( 'NONE', #54040, .T. ) ;
#52953 = ORIENTED_EDGE ( 'NONE', *, *, #39360, .T. ) ;
#52954 = AXIS2_PLACEMENT_3D ( 'NONE', #22272, #47243, #4655 ) ;
#52955 = ORIENTED_EDGE ( 'NONE', *, *, #36194, .T. ) ;
#52956 = FACE_OUTER_BOUND ( 'NONE', #22359, .T. ) ;
#52957 = FACE_OUTER_BOUND ( 'NONE', #46085, .T. ) ;
#52958 = LINE ( 'NONE', #18900, #27000 ) ;
#52959 = AXIS2_PLACEMENT_3D ( 'NONE', #37026, #41278, #28204 ) ;
#52960 = EDGE_CURVE ( 'NONE', #15384, #42326, #37635, .T. ) ;
#52961 = ADVANCED_FACE ( 'NONE', ( #19760 ), #41871, .F. ) ;
#52962 = CARTESIAN_POINT ( 'NONE',  ( -30.79411802867772607, 0.000000000000000000, 8.643412946479525516 ) ) ;
#52963 = CARTESIAN_POINT ( 'NONE',  ( -15.88130887279446490, 0.000000000000000000, 3.050160814894388839 ) ) ;
#52964 = VECTOR ( 'NONE', #7115, 999.9999999999998863 ) ;
#52966 = EDGE_CURVE ( 'NONE', #34545, #43064, #24016, .T. ) ;
#52965 = ORIENTED_EDGE ( 'NONE', *, *, #11059, .F. ) ;
#52967 = DIRECTION ( 'NONE',  ( 0.9999697198139515519, 0.000000000000000000, 0.007781995580013368816 ) ) ;
#52968 = DIRECTION ( 'NONE',  ( 0.007781995580012663651, -3.146120232559066537E-19, -0.9999697198139514409 ) ) ;
#52969 = CARTESIAN_POINT ( 'NONE',  ( -21.47263955680318404, 0.000000000000000000, 5.022634149262071190 ) ) ;
#52970 = LINE ( 'NONE', #40494, #29688 ) ;
#52971 = VECTOR ( 'NONE', #31261, 1000.000000000000114 ) ;
#52972 = ORIENTED_EDGE ( 'NONE', *, *, #7091, .T. ) ;
#52973 = LINE ( 'NONE', #10383, #31088 ) ;
#52974 = EDGE_LOOP ( 'NONE', ( #21446, #56193, #24077, #41996 ) ) ;
#52975 = CARTESIAN_POINT ( 'NONE',  ( -15.95937329197289678, -4.565544526780660917, 10.37393067521759704 ) ) ;
#52976 = CARTESIAN_POINT ( 'NONE',  ( -10.57812043228527266, 0.7721120973665049902, 0.7661985235158867980 ) ) ;
#52977 = VECTOR ( 'NONE', #25287, 1000.000000000000114 ) ;
#52978 = ORIENTED_EDGE ( 'NONE', *, *, #29785, .F. ) ;
#52979 = CARTESIAN_POINT ( 'NONE',  ( -27.99923088623136636, 0.000000000000000000, 7.757173251277078130 ) ) ;
#52980 = ORIENTED_EDGE ( 'NONE', *, *, #3357, .F. ) ;
#52981 = EDGE_CURVE ( 'NONE', #42035, #12550, #10949, .T. ) ;
#52982 = VECTOR ( 'NONE', #3926, 999.9999999999998863 ) ;
#52983 = ORIENTED_EDGE ( 'NONE', *, *, #23456, .F. ) ;
#52984 = ORIENTED_EDGE ( 'NONE', *, *, #11059, .T. ) ;
#52985 = CARTESIAN_POINT ( 'NONE',  ( -18.67619601524082285, 0.000000000000000000, 3.936400510096834893 ) ) ;
#52986 = VECTOR ( 'NONE', #51569, 999.9999999999998863 ) ;
#52987 = EDGE_LOOP ( 'NONE', ( #34952, #31857, #31909, #456 ) ) ;
#52988 = ORIENTED_EDGE ( 'NONE', *, *, #42886, .F. ) ;
#52989 = DIRECTION ( 'NONE',  ( -0.6246952433987894571, 0.7422098413412802076, 0.2426528472758539834 ) ) ;
#52990 = CARTESIAN_POINT ( 'NONE',  ( -10.00813838035478298, 0.000000000000000000, 10.77830692922518452 ) ) ;
#52991 = VERTEX_POINT ( 'NONE', #1858 ) ;
#52992 = ADVANCED_FACE ( 'NONE', ( #19184 ), #54382, .T. ) ;
#52993 = ORIENTED_EDGE ( 'NONE', *, *, #55673, .T. ) ;
#52994 = CARTESIAN_POINT ( 'NONE',  ( -15.88130887279446490, 0.000000000000000000, 3.050160814894388839 ) ) ;
#52995 = VERTEX_POINT ( 'NONE', #54131 ) ;
#52996 = ORIENTED_EDGE ( 'NONE', *, *, #36851, .T. ) ;
#52997 = EDGE_CURVE ( 'NONE', #6183, #12574, #15235, .T. ) ;
#52998 = VECTOR ( 'NONE', #31712, 1000.000000000000227 ) ;
#52999 = DIRECTION ( 'NONE',  ( 0.7660212471507180654, -0.6427876096865404731, 0.005961354470445141482 ) ) ;
#53000 = ADVANCED_FACE ( 'NONE', ( #53832 ), #23728, .F. ) ;
#53001 = VECTOR ( 'NONE', #10558, 999.9999999999998863 ) ;
#53002 = CARTESIAN_POINT ( 'NONE',  ( -55.84246788140315942, 5.810395100437911076, 5.000000000000000000 ) ) ;
#53003 = CARTESIAN_POINT ( 'NONE',  ( -21.47419595591918906, 0.000000000000000000, 5.222628093224860102 ) ) ;
#53004 = CARTESIAN_POINT ( 'NONE',  ( -15.89360807292448285, -0.1191753592594205352, 3.688726211178170455 ) ) ;
#53005 = EDGE_CURVE ( 'NONE', #33548, #20460, #49853, .T. ) ;
#53006 = EDGE_LOOP ( 'NONE', ( #33409, #26876, #43796, #15282 ) ) ;
#53007 = CARTESIAN_POINT ( 'NONE',  ( -9.768479909093388258, 0.000000000000000000, 5.683056751990515743 ) ) ;
#53008 = AXIS2_PLACEMENT_3D ( 'NONE', #21303, #42596, #38062 ) ;
#53009 = EDGE_LOOP ( 'NONE', ( #36406, #36350, #10388, #53353 ) ) ;
#53010 = EDGE_CURVE ( 'NONE', #25448, #43321, #36513, .T. ) ;
#53011 = DIRECTION ( 'NONE',  ( -0.6427681459581293666, -0.7660444431189770143, -0.005002170337467561935 ) ) ;
#53012 = CARTESIAN_POINT ( 'NONE',  ( -27.22333567087903461, 16.65220053346459750, -4.407437592157545048 ) ) ;
#53013 = VECTOR ( 'NONE', #12387, 999.9999999999998863 ) ;
#53014 = LINE ( 'NONE', #9282, #47665 ) ;
#53015 = DIRECTION ( 'NONE',  ( 0.5364919789714477361, 0.6444004775717706579, 0.5449076811759711036 ) ) ;
#53016 = CARTESIAN_POINT ( 'NONE',  ( -28.93137873341882127, 0.000000000000000000, 8.119251130998824451 ) ) ;
#53017 = CARTESIAN_POINT ( 'NONE',  ( -14.96146022573702972, -0.1191753592594187450, 3.326648331456423247 ) ) ;
#53018 = AXIS2_PLACEMENT_3D ( 'NONE', #52492, #17281, #35741 ) ;
#53019 = CARTESIAN_POINT ( 'NONE',  ( -8.833458008400651096, 0.000000000000000000, 4.951669169011005067 ) ) ;
#53020 = ORIENTED_EDGE ( 'NONE', *, *, #15266, .T. ) ;
#53021 = CARTESIAN_POINT ( 'NONE',  ( -18.15493648027519669, 0.000000000000000000, 8.572447966228459393 ) ) ;
#53022 = VECTOR ( 'NONE', #55579, 999.9999999999998863 ) ;
#53023 = CARTESIAN_POINT ( 'NONE',  ( 0.000000000000000000, 2.000000000000000000, 0.000000000000000000 ) ) ;
#53024 = CARTESIAN_POINT ( 'NONE',  ( -19.98537980836135119, 5.305366725996514710, 4.275662980210056752 ) ) ;
#53025 = FACE_OUTER_BOUND ( 'NONE', #27713, .T. ) ;
#53026 = CARTESIAN_POINT ( 'NONE',  ( -44.29771021218551397, 5.350930122822688872, -5.000000000000003553 ) ) ;
#53027 = CARTESIAN_POINT ( 'NONE',  ( -13.68401262866885482, 0.000000000000000000, 5.452579114767647894 ) ) ;
#53028 = CARTESIAN_POINT ( 'NONE',  ( -20.26176469941677993, 0.000000000000000000, 14.76116360616437895 ) ) ;
#53029 = VECTOR ( 'NONE', #49488, 1000.000000000000114 ) ;
#53030 = CARTESIAN_POINT ( 'NONE',  ( -12.13851405436063047, 0.000000000000000000, 11.68505802764555135 ) ) ;
#53031 = VECTOR ( 'NONE', #7097, 999.9999999999998863 ) ;
#53032 = EDGE_LOOP ( 'NONE', ( #44803, #43162, #50183, #19331 ) ) ;
#53033 = CARTESIAN_POINT ( 'NONE',  ( -19.18184055174032920, -0.1191753592594164968, 8.260322821228706758 ) ) ;
#53034 = DIRECTION ( 'NONE',  ( 0.005961354470445682716, -0.6427876096865404731, -0.7660212471507180654 ) ) ;
#53035 = PLANE ( 'NONE',  #21567 ) ;
#53036 = ADVANCED_FACE ( 'NONE', ( #19473 ), #54651, .F. ) ;
#53037 = CARTESIAN_POINT ( 'NONE',  ( -14.86930721471348171, 0.000000000000000000, 4.335358668806328808 ) ) ;
#53038 = CARTESIAN_POINT ( 'NONE',  ( -12.15828988943850675, -2.298917212465657833, 5.177539221031057792 ) ) ;
#53039 = CARTESIAN_POINT ( 'NONE',  ( -15.46058576464150569, -0.1191753592594190225, 7.754748858781589149 ) ) ;
#53040 = EDGE_CURVE ( 'NONE', #27291, #48737, #31978, .T. ) ;
#53041 = EDGE_CURVE ( 'NONE', #14703, #18484, #6997, .T. ) ;
#53042 = CARTESIAN_POINT ( 'NONE',  ( -2.276746449950904694, -3.901742918183043418, -2.334007935867973949 ) ) ;
#53043 = AXIS2_PLACEMENT_3D ( 'NONE', #43121, #7624, #29790 ) ;
#53044 = CARTESIAN_POINT ( 'NONE',  ( -29.86197018149027116, 0.000000000000000000, 8.281335066757780083 ) ) ;
#53045 = VECTOR ( 'NONE', #42773, 999.9999999999998863 ) ;
#53046 = CARTESIAN_POINT ( 'NONE',  ( -9.502241701925603579, 0.000000000000000000, 2.530466064606057053 ) ) ;
#53047 = AXIS2_PLACEMENT_3D ( 'NONE', #49918, #47015, #23279 ) ;
#53048 = VERTEX_POINT ( 'NONE', #41609 ) ;
#53049 = AXIS2_PLACEMENT_3D ( 'NONE', #30923, #52777, #43437 ) ;
#53050 = EDGE_CURVE ( 'NONE', #41210, #48904, #10413, .T. ) ;
#53051 = ORIENTED_EDGE ( 'NONE', *, *, #29439, .F. ) ;
#53052 = ORIENTED_EDGE ( 'NONE', *, *, #25881, .T. ) ;
#53053 = VECTOR ( 'NONE', #3912, 1000.000000000000227 ) ;
#53054 = AXIS2_PLACEMENT_3D ( 'NONE', #24499, #39251, #38720 ) ;
#53055 = ORIENTED_EDGE ( 'NONE', *, *, #998, .F. ) ;
#53056 = AXIS2_PLACEMENT_3D ( 'NONE', #20173, #38073, #47146 ) ;
#53057 = VECTOR ( 'NONE', #467, 1000.000000000000227 ) ;
#53058 = ORIENTED_EDGE ( 'NONE', *, *, #51796, .F. ) ;
#53059 = DIRECTION ( 'NONE',  ( -0.7660212471507179544, -0.6427876096865405842, -0.005961354470445141482 ) ) ;
#53060 = LINE ( 'NONE', #52227, #43926 ) ;
#53061 = VECTOR ( 'NONE', #21307, 1000.000000000000114 ) ;
#53062 = VERTEX_POINT ( 'NONE', #33937 ) ;
#53063 = EDGE_LOOP ( 'NONE', ( #28570, #40838, #10110, #18124 ) ) ;
#53064 = EDGE_CURVE ( 'NONE', #28751, #5616, #56090, .T. ) ;
#53065 = VECTOR ( 'NONE', #55135, 1000.000000000000227 ) ;
#53066 = VECTOR ( 'NONE', #21459, 999.9999999999998863 ) ;
#53067 = LINE ( 'NONE', #15007, #52069 ) ;
#53068 = ORIENTED_EDGE ( 'NONE', *, *, #24887, .T. ) ;
#53069 = CARTESIAN_POINT ( 'NONE',  ( 2.072287782118878319, 0.000000000000000000, -2.950529333540147015 ) ) ;
#53070 = DIRECTION ( 'NONE',  ( 0.007781995580012662783, 0.000000000000000000, -0.9999697198139514409 ) ) ;
#53071 = EDGE_LOOP ( 'NONE', ( #29885, #51699, #5300 ) ) ;
#53072 = CARTESIAN_POINT ( 'NONE',  ( -21.47263955680318404, 0.000000000000000000, 5.022634149262071190 ) ) ;
#53073 = ORIENTED_EDGE ( 'NONE', *, *, #26069, .F. ) ;
#53074 = PLANE ( 'NONE',  #49078 ) ;
#53075 = EDGE_CURVE ( 'NONE', #13988, #48977, #17175, .T. ) ;
#53076 = DIRECTION ( 'NONE',  ( 0.7660212471507180654, -0.6427876096865404731, 0.005961354470445141482 ) ) ;
#53077 = VECTOR ( 'NONE', #30826, 1000.000000000000227 ) ;
#53078 = DIRECTION ( 'NONE',  ( -0.6427681459581293666, -0.7660444431189770143, -0.005002170337467561935 ) ) ;
#53079 = LINE ( 'NONE', #18729, #48694 ) ;
#53080 = VERTEX_POINT ( 'NONE', #25689 ) ;
#53081 = FACE_OUTER_BOUND ( 'NONE', #47840, .T. ) ;
#53082 = CARTESIAN_POINT ( 'NONE',  ( -19.60990026154428278, 0.000000000000000000, 4.498472333781370125 ) ) ;
#53084 = VECTOR ( 'NONE', #39610, 999.9999999999998863 ) ;
#53083 = FACE_OUTER_BOUND ( 'NONE', #24017, .T. ) ;
#53085 = ORIENTED_EDGE ( 'NONE', *, *, #34188, .T. ) ;
#53086 = CARTESIAN_POINT ( 'NONE',  ( -13.22380618444906197, 0.000000000000000000, 6.025498673756209733 ) ) ;
#53087 = EDGE_LOOP ( 'NONE', ( #54333, #50852, #53656 ) ) ;
#53088 = VECTOR ( 'NONE', #37580, 1000.000000000000227 ) ;
#53089 = EDGE_CURVE ( 'NONE', #14783, #38400, #42171, .T. ) ;
#53090 = CARTESIAN_POINT ( 'NONE',  ( -15.32532195103871686, 0.000000000000000000, 3.223813647265023619 ) ) ;
#53091 = LINE ( 'NONE', #30682, #37805 ) ;
#53092 = CARTESIAN_POINT ( 'NONE',  ( -12.53175246298163970, 0.000000000000000000, 2.506889711357553008 ) ) ;
#53093 = CARTESIAN_POINT ( 'NONE',  ( -18.67775241435682432, 0.000000000000000000, 4.136394454059623804 ) ) ;
#53094 = VECTOR ( 'NONE', #25093, 1000.000000000000114 ) ;
#53095 = CARTESIAN_POINT ( 'NONE',  ( -20.24669849012556000, -1.975113310420658852, 4.682809936065343237 ) ) ;
#53096 = EDGE_CURVE ( 'NONE', #47218, #3340, #29705, .T. ) ;
#53097 = DIRECTION ( 'NONE',  ( 0.000000000000000000, 0.000000000000000000, 1.000000000000000000 ) ) ;
#53099 = ADVANCED_FACE ( 'NONE', ( #46713 ), #12910, .F. ) ;
#53098 = DIRECTION ( 'NONE',  ( -0.7660212471507179544, -0.6427876096865405842, -0.005961354470445141482 ) ) ;
#53101 = VECTOR ( 'NONE', #1459, 999.9999999999998863 ) ;
#53100 = CARTESIAN_POINT ( 'NONE',  ( -12.54324867700277046, 0.000000000000000000, 3.984128524388611314 ) ) ;
#53102 = AXIS2_PLACEMENT_3D ( 'NONE', #15459, #50397, #24830 ) ;
#53103 =( NAMED_UNIT ( * ) PLANE_ANGLE_UNIT ( ) SI_UNIT ( $, .RADIAN. ) );
#53104 = CARTESIAN_POINT ( 'NONE',  ( -15.60102546347950536, 0.000000000000000000, 12.95077420755565356 ) ) ;
#53105 = ORIENTED_EDGE ( 'NONE', *, *, #34777, .T. ) ;
#53106 = DIRECTION ( 'NONE',  ( -0.5364919789714478471, 0.6444004775717705469, -0.5449076811759709926 ) ) ;
#53107 = PLANE ( 'NONE',  #16050 ) ;
#53108 = EDGE_CURVE ( 'NONE', #1004, #45599, #42462, .T. ) ;
#53109 = CARTESIAN_POINT ( 'NONE',  ( -14.94916102560700821, 0.000000000000000000, 2.688082935172642962 ) ) ;
#53111 = AXIS2_PLACEMENT_3D ( 'NONE', #2519, #15559, #41685 ) ;
#53110 = DIRECTION ( 'NONE',  ( 0.007781995580012663651, 0.000000000000000000, -0.9999697198139515519 ) ) ;
#53112 = VECTOR ( 'NONE', #19680, 1000.000000000000000 ) ;
#53113 = EDGE_CURVE ( 'NONE', #29459, #15659, #21140, .T. ) ;
#53114 = DIRECTION ( 'NONE',  ( -0.5364919789714478471, 0.6444004775717705469, -0.5449076811759709926 ) ) ;
#53115 = CARTESIAN_POINT ( 'NONE',  ( -14.03700917569638840, -4.565544526780664469, 2.188107406206031502 ) ) ;
#53116 = ADVANCED_FACE ( 'NONE', ( #30240 ), #20610, .F. ) ;
#53117 = CARTESIAN_POINT ( 'NONE',  ( -22.40478740399063895, 0.000000000000000000, 5.384712028983816623 ) ) ;
#53118 = ORIENTED_EDGE ( 'NONE', *, *, #24253, .T. ) ;
#53119 = VECTOR ( 'NONE', #22540, 999.9999999999998863 ) ;
#53120 = VECTOR ( 'NONE', #37284, 999.9999999999998863 ) ;
#53121 = ORIENTED_EDGE ( 'NONE', *, *, #3800, .T. ) ;
#53122 = LINE ( 'NONE', #44310, #52231 ) ;
#53123 = DIRECTION ( 'NONE',  ( 0.007781995580012663651, 0.000000000000000000, -0.9999697198139515519 ) ) ;
#53124 = ADVANCED_FACE ( 'NONE', ( #29099 ), #4123, .F. ) ;
#53125 = ORIENTED_EDGE ( 'NONE', *, *, #27912, .F. ) ;
#53126 = DIRECTION ( 'NONE',  ( 0.005002170337468016433, -0.7660444431189770143, -0.6427681459581293666 ) ) ;
#53127 = EDGE_LOOP ( 'NONE', ( #44621, #48384, #33615, #3990 ) ) ;
#53128 = LINE ( 'NONE', #14770, #40159 ) ;
#53129 = AXIS2_PLACEMENT_3D ( 'NONE', #40105, #6318, #18239 ) ;
#53130 = EDGE_CURVE ( 'NONE', #23668, #42246, #21453, .T. ) ;
#53131 = EDGE_LOOP ( 'NONE', ( #45105, #43630, #54311, #1726 ) ) ;
#53132 = ORIENTED_EDGE ( 'NONE', *, *, #53580, .F. ) ;
#53133 = ORIENTED_EDGE ( 'NONE', *, *, #1487, .T. ) ;
#53134 = VECTOR ( 'NONE', #46591, 1000.000000000000114 ) ;
#53135 = DIRECTION ( 'NONE',  ( -0.005002170337468016433, -0.7660444431189770143, 0.6427681459581293666 ) ) ;
#53136 = CARTESIAN_POINT ( 'NONE',  ( -13.73672976910459909, 0.000000000000000000, 12.22661844811216270 ) ) ;
#53137 = VECTOR ( 'NONE', #26835, 1000.000000000000227 ) ;
#53138 = DIRECTION ( 'NONE',  ( 0.000000000000000000, -0.000000000000000000, -1.000000000000000000 ) ) ;
#53139 = DIRECTION ( 'NONE',  ( 0.5364919789714477361, 0.6444004775717706579, 0.5449076811759711036 ) ) ;
#53140 = EDGE_LOOP ( 'NONE', ( #13589, #2130, #23275, #13887 ) ) ;
#53141 = VECTOR ( 'NONE', #34631, 1000.000000000000227 ) ;
#53142 = VERTEX_POINT ( 'NONE', #37922 ) ;
#53143 = AXIS2_PLACEMENT_3D ( 'NONE', #55589, #54455, #2768 ) ;
#53144 = VECTOR ( 'NONE', #39871, 1000.000000000000114 ) ;
#53145 = CARTESIAN_POINT ( 'NONE',  ( -8.573006763416911369, 0.000000000000000000, 5.492354144215751965 ) ) ;
#53146 = EDGE_LOOP ( 'NONE', ( #37248, #9184, #14578, #1502 ) ) ;
#53147 = PLANE ( 'NONE',  #20056 ) ;
#53148 = VECTOR ( 'NONE', #13555, 999.9999999999998863 ) ;
#53149 = ORIENTED_EDGE ( 'NONE', *, *, #39929, .T. ) ;
#53150 = DIRECTION ( 'NONE',  ( 0.007781995580012663651, 0.000000000000000000, -0.9999697198139515519 ) ) ;
#53151 = DIRECTION ( 'NONE',  ( 0.000000000000000000, -1.000000000000000000, 0.000000000000000000 ) ) ;
#53152 = VECTOR ( 'NONE', #43582, 999.9999999999998863 ) ;
#53153 = EDGE_LOOP ( 'NONE', ( #34866, #28380, #52993, #17799 ) ) ;
#53154 = VECTOR ( 'NONE', #15009, 1000.000000000000227 ) ;
#53155 = DIRECTION ( 'NONE',  ( 0.000000000000000000, -0.000000000000000000, -1.000000000000000000 ) ) ;
#53156 = EDGE_CURVE ( 'NONE', #42084, #6779, #12640, .T. ) ;
#53157 = ORIENTED_EDGE ( 'NONE', *, *, #35532, .F. ) ;
#53158 = VECTOR ( 'NONE', #19034, 1000.000000000000227 ) ;
#53159 = PLANE ( 'NONE',  #46314 ) ;
#53160 = AXIS2_PLACEMENT_3D ( 'NONE', #10836, #28147, #2307 ) ;
#53161 = ORIENTED_EDGE ( 'NONE', *, *, #20035, .F. ) ;
#53162 = CARTESIAN_POINT ( 'NONE',  ( -20.54204810873173415, 0.000000000000000000, 4.860550213503115558 ) ) ;
#53163 = LINE ( 'NONE', #18209, #4008 ) ;
#53164 = LINE ( 'NONE', #40657, #17416 ) ;
#53165 = EDGE_LOOP ( 'NONE', ( #55442, #24762, #38685, #871, #45288 ) ) ;
#53166 = ADVANCED_FACE ( 'NONE', ( #3817 ), #47555, .F. ) ;
#53167 = LINE ( 'NONE', #10575, #2004 ) ;
#53168 = DIRECTION ( 'NONE',  ( -0.5449076811759708816, 0.6444004775717707689, 0.5364919789714475140 ) ) ;
#53169 = CARTESIAN_POINT ( 'NONE',  ( -56.72379438140767149, 4.325189740742904299, -2.436530593025232783 ) ) ;
#53170 = CARTESIAN_POINT ( 'NONE',  ( -17.73140113748535285, 0.000000000000000000, 13.85752530597602039 ) ) ;
#53172 = ADVANCED_FACE ( 'NONE', ( #8670 ), #16318, .F. ) ;
#53171 = DIRECTION ( 'NONE',  ( -0.005002170337468016433, -0.7660444431189770143, 0.6427681459581293666 ) ) ;
#53173 = VECTOR ( 'NONE', #47295, 1000.000000000000114 ) ;
#53174 = CARTESIAN_POINT ( 'NONE',  ( -66.50642983938375608, -11.33427795235789226, -1.381457631280774700 ) ) ;
#53175 = ORIENTED_EDGE ( 'NONE', *, *, #8635, .T. ) ;
#53176 = CARTESIAN_POINT ( 'NONE',  ( -15.10247214635037771, 0.000000000000000000, 8.596202949488523259 ) ) ;
#53177 = DIRECTION ( 'NONE',  ( 0.000000000000000000, -0.000000000000000000, -1.000000000000000000 ) ) ;
#53178 = LINE ( 'NONE', #1179, #3313 ) ;
#53179 = ORIENTED_EDGE ( 'NONE', *, *, #864, .T. ) ;
#53180 = CARTESIAN_POINT ( 'NONE',  ( -13.23374599935418772, 0.000000000000000000, 7.302743542824478240 ) ) ;
#53181 = LINE ( 'NONE', #40388, #4594 ) ;
#53182 = VECTOR ( 'NONE', #11168, 999.9999999999998863 ) ;
#53183 = EDGE_LOOP ( 'NONE', ( #43475, #34534, #44735, #52251 ) ) ;
#53184 = FACE_OUTER_BOUND ( 'NONE', #11963, .T. ) ;
#53185 = ADVANCED_FACE ( 'NONE', ( #3550 ), #4410, .F. ) ;
#53186 = VECTOR ( 'NONE', #36403, 1000.000000000000227 ) ;
#53187 = PLANE ( 'NONE',  #5808 ) ;
#53188 = FACE_OUTER_BOUND ( 'NONE', #22611, .T. ) ;
#53189 = ADVANCED_FACE ( 'NONE', ( #16066 ), #7523, .F. ) ;
#53190 = FACE_BOUND ( 'NONE', #366, .T. ) ;
#53191 = ORIENTED_EDGE ( 'NONE', *, *, #52757, .F. ) ;
#53192 = AXIS2_PLACEMENT_3D ( 'NONE', #54400, #37356, #12395 ) ;
#53193 = ORIENTED_EDGE ( 'NONE', *, *, #27186, .F. ) ;
#53194 = LINE ( 'NONE', #359, #26711 ) ;
#53195 = CARTESIAN_POINT ( 'NONE',  ( -15.92809671498787694, -0.1191753592594204797, 8.120442650271344931 ) ) ;
#53196 = CARTESIAN_POINT ( 'NONE',  ( -67.15282819338808906, 1.999999999999999556, -6.891906871564128068 ) ) ;
#53197 = VECTOR ( 'NONE', #48760, 1000.000000000000227 ) ;
#53198 = CARTESIAN_POINT ( 'NONE',  ( -23.33771345073609638, -0.1191753592594197858, 5.846786880686956955 ) ) ;
#53199 = ADVANCED_FACE ( 'NONE', ( #38181 ), #44677, .F. ) ;
#53201 = CARTESIAN_POINT ( 'NONE',  ( -15.99438324446388116, 0.000000000000000000, 3.787944983601566395 ) ) ;
#53200 = AXIS2_PLACEMENT_3D ( 'NONE', #19115, #36442, #29893 ) ;
#53202 = LINE ( 'NONE', #48922, #2261 ) ;
#53203 = ORIENTED_EDGE ( 'NONE', *, *, #13164, .T. ) ;
#53204 = PLANE ( 'NONE',  #30149 ) ;
#53205 = AXIS2_PLACEMENT_3D ( 'NONE', #3601, #51002, #11828 ) ;
#53206 = EDGE_CURVE ( 'NONE', #33376, #9694, #18576, .T. ) ;
#53207 = VECTOR ( 'NONE', #14611, 1000.000000000000000 ) ;
#53208 = LINE ( 'NONE', #31331, #28770 ) ;
#53209 = ORIENTED_EDGE ( 'NONE', *, *, #24998, .T. ) ;
#53210 = PLANE ( 'NONE',  #26550 ) ;
#53211 = CARTESIAN_POINT ( 'NONE',  ( 2.072287782118878319, 0.000000000000000000, -2.950529333540147015 ) ) ;
#53212 = CARTESIAN_POINT ( 'NONE',  ( -10.24305662083960300, 0.000000000000000000, 6.956685709290773900 ) ) ;
#53213 = ORIENTED_EDGE ( 'NONE', *, *, #49208, .F. ) ;
#53214 = LINE ( 'NONE', #27636, #27458 ) ;
#53215 = EDGE_LOOP ( 'NONE', ( #33880, #53125, #7769, #23201 ) ) ;
#53216 = VECTOR ( 'NONE', #54932, 1000.000000000000227 ) ;
#53217 = ORIENTED_EDGE ( 'NONE', *, *, #8715, .T. ) ;
#53218 = ORIENTED_EDGE ( 'NONE', *, *, #43946, .T. ) ;
#53219 = ORIENTED_EDGE ( 'NONE', *, *, #1036, .T. ) ;
#53220 = CARTESIAN_POINT ( 'NONE',  ( -8.941298941339892892, -0.1191753592594185784, 5.958823107244898942 ) ) ;
#53221 = PRODUCT ( 'Integrated Nail File & Cleaner Flip-Out', 'Integrated Nail File & Cleaner Flip-Out', '', ( #8776 ) ) ;
#53223 = EDGE_CURVE ( 'NONE', #11765, #51823, #30545, .T. ) ;
#53222 = ORIENTED_EDGE ( 'NONE', *, *, #37441, .T. ) ;
#53224 = FACE_OUTER_BOUND ( 'NONE', #16967, .T. ) ;
#53225 = PLANE ( 'NONE',  #477 ) ;
#53226 = ORIENTED_EDGE ( 'NONE', *, *, #30363, .F. ) ;
#53227 = DIRECTION ( 'NONE',  ( 0.9999697198139515519, 0.000000000000000000, 0.007781995580013368816 ) ) ;
#53228 = VECTOR ( 'NONE', #1581, 1000.000000000000227 ) ;
#53229 = ORIENTED_EDGE ( 'NONE', *, *, #19227, .T. ) ;
#53230 = DIRECTION ( 'NONE',  ( -0.005961354470445682716, -0.6427876096865404731, 0.7660212471507180654 ) ) ;
#53231 = EDGE_CURVE ( 'NONE', #9862, #15187, #5798, .T. ) ;
#53232 = ORIENTED_EDGE ( 'NONE', *, *, #40589, .F. ) ;
#53233 = VECTOR ( 'NONE', #37882, 1000.000000000000227 ) ;
#53234 = CARTESIAN_POINT ( 'NONE',  ( 2.072287782118878319, 0.000000000000000000, -2.950529333540147015 ) ) ;
#53235 = ADVANCED_FACE ( 'NONE', ( #48381 ), #14036, .F. ) ;
#53236 = DIRECTION ( 'NONE',  ( 0.007781995580012662783, 0.000000000000000000, -0.9999697198139514409 ) ) ;
#53237 = LINE ( 'NONE', #1788, #50416 ) ;
#53238 = EDGE_CURVE ( 'NONE', #35268, #35565, #13203, .T. ) ;
#53239 = SURFACE_STYLE_USAGE ( .BOTH. , #18575 ) ;
#53240 = CARTESIAN_POINT ( 'NONE',  ( -14.96640450444030535, 0.4483081953215045656, 2.481088123670064149 ) ) ;
#53241 = DIRECTION ( 'NONE',  ( 0.9999697198139515519, 0.000000000000000000, 0.007781995580013368816 ) ) ;
#53242 = EDGE_LOOP ( 'NONE', ( #55877, #26774, #28840, #9786 ) ) ;
#53243 = EDGE_CURVE ( 'NONE', #32666, #47865, #44405, .T. ) ;
#53244 = EDGE_CURVE ( 'NONE', #24728, #6162, #39873, .T. ) ;
#53245 = ADVANCED_FACE ( 'NONE', ( #9208 ), #18279, .F. ) ;
#53246 = ORIENTED_EDGE ( 'NONE', *, *, #31100, .F. ) ;
#53247 = VECTOR ( 'NONE', #52775, 999.9999999999998863 ) ;
#53248 = LINE ( 'NONE', #957, #55482 ) ;
#53249 = LINE ( 'NONE', #53496, #48418 ) ;
#53250 = CARTESIAN_POINT ( 'NONE',  ( -17.66575075627584113, 0.000000000000000000, 5.421592307971564217 ) ) ;
#53251 = VECTOR ( 'NONE', #24724, 1000.000000000000227 ) ;
#53252 = DIRECTION ( 'NONE',  ( 0.5364919789714477361, 0.6444004775717706579, 0.5449076811759711036 ) ) ;
#53253 = ORIENTED_EDGE ( 'NONE', *, *, #13491, .T. ) ;
#53254 = FACE_OUTER_BOUND ( 'NONE', #142, .T. ) ;
#53255 = CARTESIAN_POINT ( 'NONE',  ( -70.10219403106212610, -1.000000000000000666, -7.503912900124007912 ) ) ;
#53256 = ORIENTED_EDGE ( 'NONE', *, *, #23735, .T. ) ;
#53257 = DIRECTION ( 'NONE',  ( -0.2588190451025212946, -0.9659258262890680902, 0.000000000000000000 ) ) ;
#53258 = LINE ( 'NONE', #31664, #23140 ) ;
#53259 = ORIENTED_EDGE ( 'NONE', *, *, #7853, .T. ) ;
#53260 = CARTESIAN_POINT ( 'NONE',  ( -66.55938532089209048, -8.722345891443490373, 0.3404743498653450273 ) ) ;
#53261 = PLANE ( 'NONE',  #7911 ) ;
#53262 = EDGE_CURVE ( 'NONE', #37795, #9694, #39033, .T. ) ;
#53263 = LINE ( 'NONE', #14356, #8736 ) ;
#53264 = CARTESIAN_POINT ( 'NONE',  ( -17.90432093095618171, -0.8417996532631553119, 5.018114658037904796 ) ) ;
#53265 = EDGE_CURVE ( 'NONE', #6150, #55300, #13484, .T. ) ;
#53266 = ORIENTED_EDGE ( 'NONE', *, *, #53615, .F. ) ;
#53267 = ORIENTED_EDGE ( 'NONE', *, *, #40969, .F. ) ;
#53268 = EDGE_CURVE ( 'NONE', #35388, #21115, #40146, .T. ) ;
#53269 = DIRECTION ( 'NONE',  ( -0.5449076811759708816, 0.6444004775717707689, 0.5364919789714475140 ) ) ;
#53270 = DIRECTION ( 'NONE',  ( 0.007781995580012663651, -3.146120232559066537E-19, -0.9999697198139514409 ) ) ;
#53271 = DIRECTION ( 'NONE',  ( 0.9999697198139515519, 0.000000000000000000, 0.007781995580013368816 ) ) ;
#53272 = EDGE_CURVE ( 'NONE', #37046, #35002, #9496, .T. ) ;
#53273 = CARTESIAN_POINT ( 'NONE',  ( -10.22263688274503401, -0.03228989815065527735, 0.8511102278423342549 ) ) ;
#53274 = VECTOR ( 'NONE', #23378, 999.9999999999998863 ) ;
#53275 = FACE_OUTER_BOUND ( 'NONE', #21191, .T. ) ;
#53276 = ORIENTED_EDGE ( 'NONE', *, *, #35399, .F. ) ;
#53277 = CARTESIAN_POINT ( 'NONE',  ( -21.84802659409251291, 3.038739411681507185, 10.35492567590281254 ) ) ;
#53278 = LINE ( 'NONE', #48727, #25649 ) ;
#53280 = AXIS2_PLACEMENT_3D ( 'NONE', #14074, #48980, #37300 ) ;
#53279 = CARTESIAN_POINT ( 'NONE',  ( -12.26004374870349878, 0.000000000000000000, 1.601014058199056178 ) ) ;
#53281 = CARTESIAN_POINT ( 'NONE',  ( -28.92982233430281980, 0.000000000000000000, 7.919257187036034651 ) ) ;
#53282 = ORIENTED_EDGE ( 'NONE', *, *, #9583, .T. ) ;
#53283 = DIRECTION ( 'NONE',  ( -0.7660212471507179544, -0.6427876096865405842, -0.005961354470445141482 ) ) ;
#53284 = VERTEX_POINT ( 'NONE', #4958 ) ;
#53285 = LINE ( 'NONE', #992, #5083 ) ;
#53286 = LINE ( 'NONE', #17795, #13930 ) ;
#53287 = EDGE_LOOP ( 'NONE', ( #45685, #3734, #11376, #4144 ) ) ;
#53288 = VECTOR ( 'NONE', #16072, 999.9999999999998863 ) ;
#53289 = CARTESIAN_POINT ( 'NONE',  ( -20.54126990917373519, -0.1191753592594197858, 4.760553241521720658 ) ) ;
#53290 = VERTEX_POINT ( 'NONE', #952 ) ;
#53291 = ORIENTED_EDGE ( 'NONE', *, *, #35947, .T. ) ;
#53292 = ORIENTED_EDGE ( 'NONE', *, *, #33372, .T. ) ;
#53293 = DIRECTION ( 'NONE',  ( 0.007781995580012662783, 0.000000000000000000, -0.9999697198139514409 ) ) ;
#53294 = ORIENTED_EDGE ( 'NONE', *, *, #50780, .F. ) ;
#53295 = ORIENTED_EDGE ( 'NONE', *, *, #20859, .T. ) ;
#53296 = DIRECTION ( 'NONE',  ( 0.6427681459581294776, -0.7660444431189769032, 0.005002170337467562802 ) ) ;
#53297 = CARTESIAN_POINT ( 'NONE',  ( -14.50727508107736519, 4.333955019861511992, 2.178774186237679711 ) ) ;
#53298 = VERTEX_POINT ( 'NONE', #10047 ) ;
#53299 = ORIENTED_EDGE ( 'NONE', *, *, #50792, .F. ) ;
#53300 = LINE ( 'NONE', #14396, #30388 ) ;
#53301 = ORIENTED_EDGE ( 'NONE', *, *, #17936, .F. ) ;
#53302 = ORIENTED_EDGE ( 'NONE', *, *, #34777, .F. ) ;
#53303 = ADVANCED_FACE ( 'NONE', ( #1236 ), #103, .F. ) ;
#53304 = LINE ( 'NONE', #10409, #27593 ) ;
#53305 = DIRECTION ( 'NONE',  ( -0.6427681459581293666, -0.7660444431189770143, -0.005002170337467561935 ) ) ;
#53306 = CARTESIAN_POINT ( 'NONE',  ( -8.574563162532918170, 0.000000000000000000, 5.692348088178540877 ) ) ;
#53307 = ORIENTED_EDGE ( 'NONE', *, *, #36020, .T. ) ;
#53308 = DIRECTION ( 'NONE',  ( -0.9999697198139514409, -0.000000000000000000, -0.007781995580013368816 ) ) ;
#53309 = ORIENTED_EDGE ( 'NONE', *, *, #20834, .F. ) ;
#53310 = EDGE_CURVE ( 'NONE', #45704, #42498, #4669, .T. ) ;
#53311 = EDGE_CURVE ( 'NONE', #15384, #37968, #17747, .T. ) ;
#53312 = CARTESIAN_POINT ( 'NONE',  ( -12.60458797795435615, 0.000000000000000000, 11.86609696750642229 ) ) ;
#53313 = EDGE_CURVE ( 'NONE', #20000, #23956, #30802, .T. ) ;
#53314 = LINE ( 'NONE', #35411, #12421 ) ;
#53315 = VECTOR ( 'NONE', #28811, 999.9999999999998863 ) ;
#53316 = CARTESIAN_POINT ( 'NONE',  ( -67.62405810989892530, 0.1329463135932536511, -2.692672496485626787 ) ) ;
#53317 = LINE ( 'NONE', #35697, #4043 ) ;
#53318 = CARTESIAN_POINT ( 'NONE',  ( 2.072287782118878319, 0.000000000000000000, -2.950529333540147015 ) ) ;
#53319 = PLANE ( 'NONE',  #31368 ) ;
#53320 = ORIENTED_EDGE ( 'NONE', *, *, #47573, .F. ) ;
#53321 = DIRECTION ( 'NONE',  ( 0.000000000000000000, -0.000000000000000000, -1.000000000000000000 ) ) ;
#53322 = ORIENTED_EDGE ( 'NONE', *, *, #55513, .F. ) ;
#53323 = AXIS2_PLACEMENT_3D ( 'NONE', #33585, #25935, #24787 ) ;
#53324 = DIRECTION ( 'NONE',  ( 0.005961354470445682716, -0.6427876096865404731, -0.7660212471507180654 ) ) ;
#53325 = CARTESIAN_POINT ( 'NONE',  ( -25.20123094555300369, 0.000000000000000000, 6.470945668149052032 ) ) ;
#53326 = LINE ( 'NONE', #23749, #44442 ) ;
#53327 = CARTESIAN_POINT ( 'NONE',  ( -14.56888064431065821, -0.1191753592594197858, 12.58947452739191064 ) ) ;
#53328 = PLANE ( 'NONE',  #6906 ) ;
#53329 = CARTESIAN_POINT ( 'NONE',  ( -68.50955275228491814, 4.575831628609406792E-15, -7.038790429923466263 ) ) ;
#53330 = ORIENTED_EDGE ( 'NONE', *, *, #14297, .T. ) ;
#53331 = EDGE_CURVE ( 'NONE', #47842, #20661, #44147, .T. ) ;
#53332 = DIRECTION ( 'NONE',  ( 0.007781995580012663651, 0.000000000000000000, -0.9999697198139515519 ) ) ;
#53333 = LINE ( 'NONE', #53578, #40395 ) ;
#53334 = LINE ( 'NONE', #24048, #48159 ) ;
#53335 = EDGE_CURVE ( 'NONE', #7012, #19811, #45800, .T. ) ;
#53336 = FACE_OUTER_BOUND ( 'NONE', #2337, .T. ) ;
#53337 = LINE ( 'NONE', #53038, #44828 ) ;
#53338 = CARTESIAN_POINT ( 'NONE',  ( -58.00000000000000711, 2.000000000000000000, 7.102951435054649637E-15 ) ) ;
#53339 = CARTESIAN_POINT ( 'NONE',  ( -10.91749235849797373, 0.6102101463440048335, 2.123504717035824552 ) ) ;
#53340 = ADVANCED_FACE ( 'NONE', ( #54575 ), #49790, .F. ) ;
#53341 = DIRECTION ( 'NONE',  ( 0.007781995580012663651, -3.146120232559066537E-19, -0.9999697198139514409 ) ) ;
#53342 = CARTESIAN_POINT ( 'NONE',  ( -25.92429756520238016, 17.40220053346459750, 4.407440554554201917 ) ) ;
#53343 = ORIENTED_EDGE ( 'NONE', *, *, #25096, .T. ) ;
#53344 = EDGE_LOOP ( 'NONE', ( #999, #24241, #2883, #52897 ) ) ;
#53345 = ORIENTED_EDGE ( 'NONE', *, *, #48981, .F. ) ;
#53346 = ORIENTED_EDGE ( 'NONE', *, *, #47101, .F. ) ;
#53347 = VERTEX_POINT ( 'NONE', #14872 ) ;
#53348 = CARTESIAN_POINT ( 'NONE',  ( -31.72626587586518099, 0.000000000000000000, 9.005490826201270949 ) ) ;
#53349 = FACE_OUTER_BOUND ( 'NONE', #47958, .T. ) ;
#53350 = AXIS2_PLACEMENT_3D ( 'NONE', #16334, #5660, #36326 ) ;
#53351 = ORIENTED_EDGE ( 'NONE', *, *, #35615, .T. ) ;
#53352 = VERTEX_POINT ( 'NONE', #6625 ) ;
#53353 = ORIENTED_EDGE ( 'NONE', *, *, #471, .F. ) ;
#53354 = PLANE ( 'NONE',  #13082 ) ;
#53355 = DIRECTION ( 'NONE',  ( 0.000000000000000000, -1.000000000000000000, 0.000000000000000000 ) ) ;
#53356 = PLANE ( 'NONE',  #25011 ) ;
#53357 = ORIENTED_EDGE ( 'NONE', *, *, #17837, .T. ) ;
#53358 = DIRECTION ( 'NONE',  ( -0.005961354470445682716, -0.6427876096865404731, 0.7660212471507180654 ) ) ;
#53360 = ORIENTED_EDGE ( 'NONE', *, *, #52380, .F. ) ;
#53359 = EDGE_CURVE ( 'NONE', #40111, #12564, #6354, .T. ) ;
#53361 = DIRECTION ( 'NONE',  ( 0.9999697198139515519, 0.000000000000000000, 0.007781995580013368816 ) ) ;
#53362 = FACE_OUTER_BOUND ( 'NONE', #10526, .T. ) ;
#53363 = EDGE_CURVE ( 'NONE', #20696, #34483, #32487, .T. ) ;
#53364 = EDGE_CURVE ( 'NONE', #16744, #37607, #10882, .T. ) ;
#53365 = CARTESIAN_POINT ( 'NONE',  ( -21.47419595591918906, 0.000000000000000000, 5.222628093224860102 ) ) ;
#53366 = DIRECTION ( 'NONE',  ( -0.005961354470445682716, -0.6427876096865404731, 0.7660212471507180654 ) ) ;
#53367 = DIRECTION ( 'NONE',  ( -0.9999697198139514409, -0.000000000000000000, -0.007781995580013368816 ) ) ;
#53368 = LINE ( 'NONE', #40594, #38348 ) ;
#53369 = CARTESIAN_POINT ( 'NONE',  ( -13.08486533123210194, 0.000000000000000000, 1.963927175729152541 ) ) ;
#53370 = EDGE_LOOP ( 'NONE', ( #54641, #51785, #30356, #24286 ) ) ;
#53371 = LINE ( 'NONE', #40300, #14711 ) ;
#53372 = ORIENTED_EDGE ( 'NONE', *, *, #5182, .T. ) ;
#53373 = LINE ( 'NONE', #22982, #43765 ) ;
#53374 = CARTESIAN_POINT ( 'NONE',  ( -14.04368264607599137, -0.1191753592594188005, 4.811118968023500919 ) ) ;
#53375 = DIRECTION ( 'NONE',  ( 0.007781995580012663651, -3.146120232559066537E-19, -0.9999697198139514409 ) ) ;
#53376 = CARTESIAN_POINT ( 'NONE',  ( -18.65372086127329609, -5.536956232915662746, 13.01475887526525099 ) ) ;
#53377 = LINE ( 'NONE', #40605, #43170 ) ;
#53378 = CARTESIAN_POINT ( 'NONE',  ( 2.072287782118878319, 0.000000000000000000, -2.950529333540147015 ) ) ;
#53379 = FACE_OUTER_BOUND ( 'NONE', #7308, .T. ) ;
#53380 = CARTESIAN_POINT ( 'NONE',  ( -24.27063949748155380, 0.000000000000000000, 6.308861732390097288 ) ) ;
#53381 = CARTESIAN_POINT ( 'NONE',  ( -17.09340172029636662, 0.000000000000000000, 9.858031298192779346 ) ) ;
#53382 = ORIENTED_EDGE ( 'NONE', *, *, #39212, .T. ) ;
#53383 = PLANE ( 'NONE',  #35728 ) ;
#53384 = PLANE ( 'NONE',  #8805 ) ;
#53385 = CARTESIAN_POINT ( 'NONE',  ( 2.072287782118878319, 0.000000000000000000, -2.950529333540147015 ) ) ;
#53386 = DIRECTION ( 'NONE',  ( -0.9999697198139514409, -0.000000000000000000, -0.007781995580013368816 ) ) ;
#53387 = VECTOR ( 'NONE', #30999, 1000.000000000000000 ) ;
#53388 = CARTESIAN_POINT ( 'NONE',  ( -16.06709938707323460, 0.000000000000000000, 13.13181314741652628 ) ) ;
#53389 = ADVANCED_FACE ( 'NONE', ( #19396 ), #41271, .F. ) ;
#53390 = CARTESIAN_POINT ( 'NONE',  ( -14.59891615482461802, 0.000000000000000000, 3.598798774942804979 ) ) ;
#53391 = CARTESIAN_POINT ( 'NONE',  ( -24.83619032682412353, 18.20871928901600256, 4.561852666301203563 ) ) ;
#53392 = ORIENTED_EDGE ( 'NONE', *, *, #17293, .T. ) ;
#53393 = ORIENTED_EDGE ( 'NONE', *, *, #48428, .T. ) ;
#53394 = ADVANCED_FACE ( 'NONE', ( #24237 ), #27950, .F. ) ;
#53395 = LINE ( 'NONE', #9952, #34118 ) ;
#53396 = CARTESIAN_POINT ( 'NONE',  ( -12.83519780597105253, -4.727446477803161073, 9.426103502958849134 ) ) ;
#53397 = ORIENTED_EDGE ( 'NONE', *, *, #29946, .F. ) ;
#53398 = DIRECTION ( 'NONE',  ( 0.5449076811759707706, 0.6444004775717708799, -0.5364919789714476250 ) ) ;
#53399 = ADVANCED_FACE ( 'NONE', ( #53754 ), #6103, .F. ) ;
#53400 = ORIENTED_EDGE ( 'NONE', *, *, #22834, .F. ) ;
#53401 = CARTESIAN_POINT ( 'NONE',  ( -11.83055794499902902, -2.460819163488157546, 5.315945687937546182 ) ) ;
#53402 = VERTEX_POINT ( 'NONE', #15170 ) ;
#53403 = VERTEX_POINT ( 'NONE', #37272 ) ;
#53404 = ORIENTED_EDGE ( 'NONE', *, *, #22595, .T. ) ;
#53405 = CARTESIAN_POINT ( 'NONE',  ( -36.91819796696599099, 0.000000000000000000, 21.84982018086542155 ) ) ;
#53406 = LINE ( 'NONE', #36644, #55870 ) ;
#53407 = CARTESIAN_POINT ( 'NONE',  ( -70.10169143752739274, -0.9999999999999995559, 7.503902134509972122 ) ) ;
#53408 = CARTESIAN_POINT ( 'NONE',  ( -16.89925026227929195, -0.1191753592594197858, 13.49466922669627422 ) ) ;
#53409 = EDGE_LOOP ( 'NONE', ( #22350, #39197, #28859, #5363 ) ) ;
#53410 = ORIENTED_EDGE ( 'NONE', *, *, #43473, .F. ) ;
#53411 = DIRECTION ( 'NONE',  ( 0.5364919789714477361, 0.6444004775717706579, 0.5449076811759711036 ) ) ;
#53412 = ORIENTED_EDGE ( 'NONE', *, *, #27188, .F. ) ;
#53413 = FACE_OUTER_BOUND ( 'NONE', #32703, .T. ) ;
#53414 = ADVANCED_FACE ( 'NONE', ( #15415 ), #32729, .F. ) ;
#53415 = EDGE_LOOP ( 'NONE', ( #18460, #2077, #38893, #18656 ) ) ;
#53416 = CARTESIAN_POINT ( 'NONE',  ( -26.13493519185646008, 0.000000000000000000, 7.033017491833586377 ) ) ;
#53417 = CARTESIAN_POINT ( 'NONE',  ( -14.89385604187174295, 0.000000000000000000, 7.489830238831231668 ) ) ;
#53418 = PRESENTATION_LAYER_ASSIGNMENT (  '', '', ( #20778 ) ) ;
#53419 = EDGE_LOOP ( 'NONE', ( #42003, #26512, #43898, #9516 ) ) ;
#53420 = ADVANCED_FACE ( 'NONE', ( #40721 ), #28477, .F. ) ;
#53421 = CARTESIAN_POINT ( 'NONE',  ( -10.41143597624427919, 0.000000000000000000, 2.892722574339361863 ) ) ;
#53422 = ORIENTED_EDGE ( 'NONE', *, *, #16222, .F. ) ;
#53423 = EDGE_CURVE ( 'NONE', #44308, #14388, #32200, .T. ) ;
#53424 = DIRECTION ( 'NONE',  ( 0.005002170337468016433, -0.7660444431189770143, -0.6427681459581293666 ) ) ;
#53425 = VERTEX_POINT ( 'NONE', #23121 ) ;
#53426 = FACE_OUTER_BOUND ( 'NONE', #26552, .T. ) ;
#53427 = LINE ( 'NONE', #40369, #43893 ) ;
#53428 = DIRECTION ( 'NONE',  ( -0.9999697198139514409, -0.000000000000000000, -0.007781995580013368816 ) ) ;
#53429 = ORIENTED_EDGE ( 'NONE', *, *, #45563, .T. ) ;
#53430 = CARTESIAN_POINT ( 'NONE',  ( -11.20636620717317378, 0.000000000000000000, 11.32298014792380414 ) ) ;
#53431 = FACE_OUTER_BOUND ( 'NONE', #26197, .T. ) ;
#53432 = CARTESIAN_POINT ( 'NONE',  ( -13.23087194584890369, 0.000000000000000000, 6.933433839566713885 ) ) ;
#53433 = FACE_OUTER_BOUND ( 'NONE', #54707, .T. ) ;
#53434 = CARTESIAN_POINT ( 'NONE',  ( -14.86224145331363466, 0.000000000000000000, 3.427423502995822879 ) ) ;
#53435 = CARTESIAN_POINT ( 'NONE',  ( -14.98732670728457173, -0.1191753592594181482, 6.650435660776302882 ) ) ;
#53436 = EDGE_CURVE ( 'NONE', #31087, #13272, #40450, .T. ) ;
#53437 = CARTESIAN_POINT ( 'NONE',  ( -64.93003644718953637, -11.15350629512717795, -3.167379070703715271 ) ) ;
#53438 = VERTEX_POINT ( 'NONE', #18869 ) ;
#53439 = CARTESIAN_POINT ( 'NONE',  ( -20.08396230501010393, -0.1191753592594199662, 4.764112115039379702 ) ) ;
#53440 = LINE ( 'NONE', #22514, #33169 ) ;
#53441 = CARTESIAN_POINT ( 'NONE',  ( -65.72105987057051379, -5.204170427930421283E-15, -1.901374313756482026 ) ) ;
#53442 = ORIENTED_EDGE ( 'NONE', *, *, #3618, .T. ) ;
#53443 = DIRECTION ( 'NONE',  ( 0.007781995580012663651, -3.146120232559066537E-19, -0.9999697198139514409 ) ) ;
#53444 = LINE ( 'NONE', #10840, #37216 ) ;
#53445 = ORIENTED_EDGE ( 'NONE', *, *, #42777, .T. ) ;
#53446 = DIRECTION ( 'NONE',  ( 0.000000000000000000, -1.000000000000000000, 0.000000000000000000 ) ) ;
#53447 = LINE ( 'NONE', #23616, #14253 ) ;
#53448 = FACE_OUTER_BOUND ( 'NONE', #29095, .T. ) ;
#53449 = ORIENTED_EDGE ( 'NONE', *, *, #8411, .F. ) ;
#53450 = VERTEX_POINT ( 'NONE', #36186 ) ;
#53451 = DIRECTION ( 'NONE',  ( 0.005002170337468016433, -0.7660444431189770143, -0.6427681459581293666 ) ) ;
#53452 = DIRECTION ( 'NONE',  ( -0.005002170337468016433, -0.7660444431189770143, 0.6427681459581293666 ) ) ;
#53453 = CARTESIAN_POINT ( 'NONE',  ( -17.69095614226269930, 3.686347215771511365, 3.436086108215560486 ) ) ;
#53454 = AXIS2_PLACEMENT_3D ( 'NONE', #41961, #41441, #2230 ) ;
#53455 = PLANE ( 'NONE',  #44607 ) ;
#53456 = ORIENTED_EDGE ( 'NONE', *, *, #3280, .T. ) ;
#53457 = LINE ( 'NONE', #14556, #34961 ) ;
#53458 = EDGE_CURVE ( 'NONE', #55644, #607, #7729, .T. ) ;
#53459 = VERTEX_POINT ( 'NONE', #14590 ) ;
#53460 = CARTESIAN_POINT ( 'NONE',  ( -19.63455492762453858, 0.4483081953215047322, 5.243799167625045499 ) ) ;
#53461 = PLANE ( 'NONE',  #8728 ) ;
#53462 = ORIENTED_EDGE ( 'NONE', *, *, #36851, .F. ) ;
#53463 = CARTESIAN_POINT ( 'NONE',  ( -12.06292385824599123, 0.000000000000000000, 1.971880160572822893 ) ) ;
#53464 = DIRECTION ( 'NONE',  ( -0.5364919789714478471, 0.6444004775717705469, -0.5449076811759709926 ) ) ;
#53465 = DIRECTION ( 'NONE',  ( -0.005961354470445682716, -0.6427876096865404731, 0.7660212471507180654 ) ) ;
#53466 = ADVANCED_FACE ( 'NONE', ( #23403 ), #1790, .F. ) ;
#53467 = VERTEX_POINT ( 'NONE', #16531 ) ;
#53468 = CARTESIAN_POINT ( 'NONE',  ( -63.00984630926863161, 1.788483511016180305, 2.999999999999993339 ) ) ;
#53469 = ORIENTED_EDGE ( 'NONE', *, *, #281, .F. ) ;
#53470 = EDGE_CURVE ( 'NONE', #9106, #38880, #50629, .T. ) ;
#53471 = EDGE_CURVE ( 'NONE', #33893, #52782, #34169, .T. ) ;
#53472 = EDGE_LOOP ( 'NONE', ( #53520, #29614, #13902, #27052 ) ) ;
#53473 = ORIENTED_EDGE ( 'NONE', *, *, #7074, .F. ) ;
#53474 = LINE ( 'NONE', #49775, #19530 ) ;
#53475 = ORIENTED_EDGE ( 'NONE', *, *, #40726, .F. ) ;
#53476 = DIRECTION ( 'NONE',  ( 0.007781995580012662783, 0.000000000000000000, -0.9999697198139514409 ) ) ;
#53477 = ADVANCED_FACE ( 'NONE', ( #3200 ), #33577, .F. ) ;
#53478 = EDGE_LOOP ( 'NONE', ( #16508, #9014, #44120, #36452 ) ) ;
#53479 = CARTESIAN_POINT ( 'NONE',  ( -16.92940514515661832, 0.000000000000000000, 4.519332566581076627 ) ) ;
#53480 = FACE_OUTER_BOUND ( 'NONE', #24163, .T. ) ;
#53481 = EDGE_LOOP ( 'NONE', ( #47306, #13670, #43423, #46378 ) ) ;
#53482 = EDGE_CURVE ( 'NONE', #8005, #1853, #50884, .T. ) ;
#53483 = DIRECTION ( 'NONE',  ( 0.007781995580012662783, 0.000000000000000000, -0.9999697198139514409 ) ) ;
#53484 = ORIENTED_EDGE ( 'NONE', *, *, #22662, .F. ) ;
#53485 = EDGE_CURVE ( 'NONE', #32862, #39389, #24489, .T. ) ;
#53486 = CARTESIAN_POINT ( 'NONE',  ( -20.54204810873173415, 0.000000000000000000, 4.860550213503115558 ) ) ;
#53487 = PLANE ( 'NONE',  #16591 ) ;
#53488 = CARTESIAN_POINT ( 'NONE',  ( -56.75000000000000711, 0.000000000000000000, -2.749999999999994671 ) ) ;
#53489 = CARTESIAN_POINT ( 'NONE',  ( -9.646137801466288408, 0.000000000000000000, 2.160014162080004851 ) ) ;
#53490 = DIRECTION ( 'NONE',  ( 0.9999697198139515519, 0.000000000000000000, 0.007781995580013368816 ) ) ;
#53491 = LINE ( 'NONE', #45251, #25565 ) ;
#53492 = ORIENTED_EDGE ( 'NONE', *, *, #41769, .F. ) ;
#53493 = ADVANCED_FACE ( 'NONE', ( #9072 ), #11987, .F. ) ;
#53494 = ORIENTED_EDGE ( 'NONE', *, *, #1156, .F. ) ;
#53495 = LINE ( 'NONE', #24493, #11012 ) ;
#53496 = CARTESIAN_POINT ( 'NONE',  ( 1.086233639165236964, -1.000000000000000000, 2.796443541562362078 ) ) ;
#53497 = DIRECTION ( 'NONE',  ( -0.6427681459581293666, -0.7660444431189770143, -0.005002170337467561935 ) ) ;
#53498 = EDGE_CURVE ( 'NONE', #12870, #9978, #7755, .T. ) ;
#53499 = CARTESIAN_POINT ( 'NONE',  ( -9.110551994824897193, 0.000000000000000000, 3.538847790438064411 ) ) ;
#53500 = ORIENTED_EDGE ( 'NONE', *, *, #52272, .F. ) ;
#53501 = PLANE ( 'NONE',  #17729 ) ;
#53502 = DIRECTION ( 'NONE',  ( 0.6427681459581294776, -0.7660444431189769032, 0.005002170337467562802 ) ) ;
#53503 = EDGE_LOOP ( 'NONE', ( #44484, #21682, #46318, #7680 ) ) ;
#53504 = DIRECTION ( 'NONE',  ( 0.000000000000000000, -1.000000000000000000, 0.000000000000000000 ) ) ;
#53505 = CARTESIAN_POINT ( 'NONE',  ( -26.55142373434009073, 17.32880420549185985, -4.634472827760601099 ) ) ;
#53506 = ORIENTED_EDGE ( 'NONE', *, *, #25043, .T. ) ;
#53507 = CARTESIAN_POINT ( 'NONE',  ( -68.62489455609114941, -8.958878114863663811, 6.810182420670462200 ) ) ;
#53508 = CARTESIAN_POINT ( 'NONE',  ( 0.000000000000000000, -1.000000000000000000, 0.000000000000000000 ) ) ;
#53509 = DIRECTION ( 'NONE',  ( -0.005961354470445682716, -0.6427876096865404731, 0.7660212471507180654 ) ) ;
#53510 = DIRECTION ( 'NONE',  ( 0.5364919789714477361, 0.6444004775717706579, 0.5449076811759711036 ) ) ;
#53511 = CARTESIAN_POINT ( 'NONE',  ( -19.60912206198628027, -0.1191753592594197858, 4.398475361799976113 ) ) ;
#53512 = ORIENTED_EDGE ( 'NONE', *, *, #12944, .F. ) ;
#53513 = ORIENTED_EDGE ( 'NONE', *, *, #11932, .F. ) ;
#53514 = DIRECTION ( 'NONE',  ( 0.5364919789714477361, 0.6444004775717706579, 0.5449076811759711036 ) ) ;
#53515 = DIRECTION ( 'NONE',  ( 0.007781995580012662783, 0.000000000000000000, -0.9999697198139514409 ) ) ;
#53516 = PLANE ( 'NONE',  #51474 ) ;
#53517 = CARTESIAN_POINT ( 'NONE',  ( 6.001673238768763241, 0.0004827855012993410204, 0.7726390298733384343 ) ) ;
#53518 = CARTESIAN_POINT ( 'NONE',  ( -16.92112509763774142, -1.327505506330658003, 5.433334058757370855 ) ) ;
#53519 = EDGE_CURVE ( 'NONE', #32268, #14885, #25083, .T. ) ;
#53520 = ORIENTED_EDGE ( 'NONE', *, *, #37507, .F. ) ;
#53521 = PLANE ( 'NONE',  #12017 ) ;
#53522 = DIRECTION ( 'NONE',  ( 0.005961354470445682716, -0.6427876096865404731, -0.7660212471507180654 ) ) ;
#53523 = VECTOR ( 'NONE', #779, 1000.000000000000227 ) ;
#53524 = CARTESIAN_POINT ( 'NONE',  ( -11.12921961194253306, 0.000000000000000000, 1.409808336888289437 ) ) ;
#53525 = LINE ( 'NONE', #45292, #35118 ) ;
#53526 = ORIENTED_EDGE ( 'NONE', *, *, #47907, .F. ) ;
#53527 = CARTESIAN_POINT ( 'NONE',  ( -67.02814355662815160, -11.39410505754381475, 7.454431982338129536 ) ) ;
#53528 = ORIENTED_EDGE ( 'NONE', *, *, #3546, .T. ) ;
#53529 = DIRECTION ( 'NONE',  ( 0.005002170337468016433, -0.7660444431189770143, -0.6427681459581293666 ) ) ;
#53530 = ADVANCED_FACE ( 'NONE', ( #55430 ), #26377, .F. ) ;
#53531 = EDGE_CURVE ( 'NONE', #6183, #2815, #8039, .T. ) ;
#53532 = DIRECTION ( 'NONE',  ( 0.007781995580012662783, 0.000000000000000000, -0.9999697198139514409 ) ) ;
#53533 = ORIENTED_EDGE ( 'NONE', *, *, #24447, .F. ) ;
#53534 = CARTESIAN_POINT ( 'NONE',  ( -18.70240708043708366, 0.4483081953215047322, 4.881721287903300066 ) ) ;
#53535 = ORIENTED_EDGE ( 'NONE', *, *, #29406, .F. ) ;
#53536 = ADVANCED_FACE ( 'NONE', ( #12577 ), #3749, .F. ) ;
#53537 = ORIENTED_EDGE ( 'NONE', *, *, #36755, .F. ) ;
#53538 = ORIENTED_EDGE ( 'NONE', *, *, #10886, .T. ) ;
#53539 = CARTESIAN_POINT ( 'NONE',  ( -27.56460882755735398, 16.74384151918395247, 4.673983433494172779 ) ) ;
#53540 = ORIENTED_EDGE ( 'NONE', *, *, #30342, .T. ) ;
#53541 = ORIENTED_EDGE ( 'NONE', *, *, #13260, .T. ) ;
#53542 = PLANE ( 'NONE',  #10271 ) ;
#53543 = DIRECTION ( 'NONE',  ( 0.005002170337468016433, -0.7660444431189770143, -0.6427681459581293666 ) ) ;
#53544 = ORIENTED_EDGE ( 'NONE', *, *, #37865, .F. ) ;
#53545 = ORIENTED_EDGE ( 'NONE', *, *, #16301, .T. ) ;
#53546 = CARTESIAN_POINT ( 'NONE',  ( -16.96521144160929140, 0.000000000000000000, 9.120364764969224325 ) ) ;
#53547 = ADVANCED_FACE ( 'NONE', ( #38398 ), #55723, .F. ) ;
#53548 = ORIENTED_EDGE ( 'NONE', *, *, #13506, .F. ) ;
#53549 = VERTEX_POINT ( 'NONE', #55168 ) ;
#53550 = EDGE_CURVE ( 'NONE', #36925, #16114, #16055, .T. ) ;
#53551 = CARTESIAN_POINT ( 'NONE',  ( -13.14499926216616643, 2.714935509636507316, 1.701275193964931765 ) ) ;
#53552 = CARTESIAN_POINT ( 'NONE',  ( 4.930947970565944694, -1.129146301979397693, 1.967953638241001446 ) ) ;
#53553 = DIRECTION ( 'NONE',  ( -0.005961354470445682716, -0.6427876096865404731, 0.7660212471507180654 ) ) ;
#53554 = CARTESIAN_POINT ( 'NONE',  ( -28.93137873341882127, 0.000000000000000000, 8.119251130998824451 ) ) ;
#53555 = ORIENTED_EDGE ( 'NONE', *, *, #47332, .T. ) ;
#53556 = CARTESIAN_POINT ( 'NONE',  ( -19.60834386242827776, 0.000000000000000000, 4.298478389818581213 ) ) ;
#53557 = EDGE_LOOP ( 'NONE', ( #39950, #16110, #41365, #28363 ) ) ;
#53558 = ADVANCED_FACE ( 'NONE', ( #16256 ), #46337, .F. ) ;
#53559 = PLANE ( 'NONE',  #2154 ) ;
#53560 = VECTOR ( 'NONE', #1483, 999.9999999999998863 ) ;
#53561 = LINE ( 'NONE', #23478, #16955 ) ;
#53562 = CARTESIAN_POINT ( 'NONE',  ( -68.48130668646780350, 0.1328705276719804873, -5.273316683197703192 ) ) ;
#53563 = DIRECTION ( 'NONE',  ( -0.9999697198139514409, -0.000000000000000000, -0.007781995580013368816 ) ) ;
#53564 = LINE ( 'NONE', #44480, #55675 ) ;
#53565 = DIRECTION ( 'NONE',  ( -0.9999697198139514409, -0.000000000000000000, -0.007781995580013368816 ) ) ;
#53566 = ORIENTED_EDGE ( 'NONE', *, *, #56086, .T. ) ;
#53567 = CARTESIAN_POINT ( 'NONE',  ( -14.12853115097296985, 0.000000000000000000, 2.863795280195287507 ) ) ;
#53568 = ORIENTED_EDGE ( 'NONE', *, *, #51679, .T. ) ;
#53569 = CARTESIAN_POINT ( 'NONE',  ( -29.86197018149027116, 0.000000000000000000, 8.281335066757780083 ) ) ;
#53570 = CARTESIAN_POINT ( 'NONE',  ( -19.79569077582305070, 0.000000000000000000, 14.58012466630350445 ) ) ;
#53571 = CARTESIAN_POINT ( 'NONE',  ( 2.072287782118878319, 0.000000000000000000, -2.950529333540147015 ) ) ;
#53572 = LINE ( 'NONE', #14678, #24074 ) ;
#53573 = DIRECTION ( 'NONE',  ( 0.5364919789714477361, 0.6444004775717706579, 0.5449076811759711036 ) ) ;
#53574 = CARTESIAN_POINT ( 'NONE',  ( -67.92731540425158698, 5.350669522624571327E-13, 6.206396125462542379 ) ) ;
#53575 = SHAPE_REPRESENTATION ( 'Curved Precision Cutting Blades', ( #2610 ), #47980 ) ;
#53576 = VERTEX_POINT ( 'NONE', #20224 ) ;
#53577 = PLANE ( 'NONE',  #3021 ) ;
#53578 = CARTESIAN_POINT ( 'NONE',  ( -25.20123094555300369, 0.000000000000000000, 6.470945668149052032 ) ) ;
#53579 = CARTESIAN_POINT ( 'NONE',  ( -12.55474489102389946, 0.000000000000000000, 5.461367337419668289 ) ) ;
#53580 = EDGE_CURVE ( 'NONE', #8803, #5010, #13604, .T. ) ;
#53581 = VECTOR ( 'NONE', #3409, 1000.000000000000114 ) ;
#53582 = DIRECTION ( 'NONE',  ( 0.5364919789714477361, 0.6444004775717706579, 0.5449076811759711036 ) ) ;
#53583 = CARTESIAN_POINT ( 'NONE',  ( -16.92078298464076624, 0.000000000000000000, 3.411403456807782231 ) ) ;
#53584 = EDGE_CURVE ( 'NONE', #27927, #31885, #33324, .T. ) ;
#53585 = FACE_OUTER_BOUND ( 'NONE', #25065, .T. ) ;
#53586 = LINE ( 'NONE', #6460, #24150 ) ;
#53587 = EDGE_CURVE ( 'NONE', #5924, #47914, #44283, .T. ) ;
#53588 = CARTESIAN_POINT ( 'NONE',  ( -13.97352483423203573, 0.000000000000000000, 8.646165164180368734 ) ) ;
#53589 = EDGE_CURVE ( 'NONE', #33995, #33216, #1384, .T. ) ;
#53590 = ADVANCED_FACE ( 'NONE', ( #6229 ), #18423, .F. ) ;
#53591 = EDGE_CURVE ( 'NONE', #15384, #37808, #53079, .T. ) ;
#53592 = ORIENTED_EDGE ( 'NONE', *, *, #45850, .F. ) ;
#53593 = VECTOR ( 'NONE', #22752, 1000.000000000000227 ) ;
#53594 = ADVANCED_FACE ( 'NONE', ( #23530 ), #5644, .F. ) ;
#53595 = VECTOR ( 'NONE', #45148, 1000.000000000000114 ) ;
#53596 = VERTEX_POINT ( 'NONE', #22438 ) ;
#53597 = ORIENTED_EDGE ( 'NONE', *, *, #45565, .F. ) ;
#53598 = ORIENTED_EDGE ( 'NONE', *, *, #339, .F. ) ;
#53599 = ORIENTED_EDGE ( 'NONE', *, *, #8278, .T. ) ;
#53600 = CARTESIAN_POINT ( 'NONE',  ( -6.110905869600904872, 1.712176620043476140E-14, -3.600000000000000089 ) ) ;
#53601 = PLANE ( 'NONE',  #7653 ) ;
#53602 = EDGE_LOOP ( 'NONE', ( #745, #32298, #14200, #23626 ) ) ;
#53603 = VERTEX_POINT ( 'NONE', #40001 ) ;
#53604 = EDGE_CURVE ( 'NONE', #22884, #8997, #14727, .T. ) ;
#53605 = ORIENTED_EDGE ( 'NONE', *, *, #26141, .T. ) ;
#53606 = ADVANCED_FACE ( 'NONE', ( #39746 ), #1087, .F. ) ;
#53607 = CARTESIAN_POINT ( 'NONE',  ( -67.15568563940774993, -9.395623621142684456, -5.540714948658321148 ) ) ;
#53608 = ADVANCED_FACE ( 'NONE', ( #15019 ), #22687, .F. ) ;
#53609 = CARTESIAN_POINT ( 'NONE',  ( -18.67775241435682432, 0.000000000000000000, 4.136394454059623804 ) ) ;
#53610 = LINE ( 'NONE', #49360, #45012 ) ;
#53611 = EDGE_LOOP ( 'NONE', ( #28386, #10791, #38454, #16162 ) ) ;
#53612 = CARTESIAN_POINT ( 'NONE',  ( -15.35495738922491604, -4.403642575758162536, 9.873446328589366772 ) ) ;
#53613 = ORIENTED_EDGE ( 'NONE', *, *, #26310, .T. ) ;
#53614 = VECTOR ( 'NONE', #47663, 1000.000000000000114 ) ;
#53615 = EDGE_CURVE ( 'NONE', #14805, #55847, #32051, .T. ) ;
#53616 = VECTOR ( 'NONE', #2207, 1000.000000000000114 ) ;
#53617 = DIRECTION ( 'NONE',  ( 0.9999697198139515519, 0.000000000000000000, 0.007781995580013368816 ) ) ;
#53618 = CARTESIAN_POINT ( 'NONE',  ( -9.036326005868723144, 0.000000000000000000, 5.319422473152766173 ) ) ;
#53619 = ADVANCED_FACE ( 'NONE', ( #27507 ), #48824, .F. ) ;
#53620 = CARTESIAN_POINT ( 'NONE',  ( -23.33693525117809386, 0.000000000000000000, 5.746789908705562944 ) ) ;
#53621 = CARTESIAN_POINT ( 'NONE',  ( -13.70281334881656043, 0.000000000000000000, 7.868431278277022045 ) ) ;
#53622 = DIRECTION ( 'NONE',  ( -0.5449076811759708816, 0.6444004775717707689, 0.5364919789714475140 ) ) ;
#53623 = PLANE ( 'NONE',  #19295 ) ;
#53624 = PLANE ( 'NONE',  #43930 ) ;
#53625 = ORIENTED_EDGE ( 'NONE', *, *, #4556, .T. ) ;
#53626 = DIRECTION ( 'NONE',  ( 0.005961354470445682716, -0.6427876096865404731, -0.7660212471507180654 ) ) ;
#53627 = ORIENTED_EDGE ( 'NONE', *, *, #53519, .F. ) ;
#53628 = DIRECTION ( 'NONE',  ( -0.9999697198139514409, -0.000000000000000000, -0.007781995580013368816 ) ) ;
#53629 = FACE_OUTER_BOUND ( 'NONE', #29157, .T. ) ;
#53630 = CARTESIAN_POINT ( 'NONE',  ( -24.26986129792355129, -0.1191753592594197858, 6.208864760408702388 ) ) ;
#53631 = FACE_OUTER_BOUND ( 'NONE', #287, .T. ) ;
#53632 = FACE_OUTER_BOUND ( 'NONE', #19802, .T. ) ;
#53633 = LINE ( 'NONE', #49095, #29470 ) ;
#53634 = DIRECTION ( 'NONE',  ( -0.05705673239519650636, 0.9983709377222390602, 2.351258244848514932E-16 ) ) ;
#53635 = VECTOR ( 'NONE', #24158, 1000.000000000000227 ) ;
#53636 = LINE ( 'NONE', #53380, #50964 ) ;
#53637 = PRESENTATION_STYLE_ASSIGNMENT (( #48247 ) ) ;
#53638 = PLANE ( 'NONE',  #7867 ) ;
#53639 = EDGE_LOOP ( 'NONE', ( #24492, #17420, #29575, #49489 ) ) ;
#53640 = LINE ( 'NONE', #27532, #7577 ) ;
#53641 = DIRECTION ( 'NONE',  ( -0.5449076811759708816, 0.6444004775717707689, 0.5364919789714475140 ) ) ;
#53642 = CARTESIAN_POINT ( 'NONE',  ( -67.50725361308181505, -1.000000000000000444, 2.158836163547857900 ) ) ;
#53643 = DIRECTION ( 'NONE',  ( -0.9999697198139514409, -0.000000000000000000, -0.007781995580013368816 ) ) ;
#53644 = CARTESIAN_POINT ( 'NONE',  ( -11.36082814446342759, 0.000000000000000000, 5.470658673607694311 ) ) ;
#53645 = CARTESIAN_POINT ( 'NONE',  ( 4.912750499197527709, -1.131233082521084565, -2.029539223447461627 ) ) ;
#53646 = CARTESIAN_POINT ( 'NONE',  ( -13.17065887352947762, -0.1191753592594197858, 12.04635770780929427 ) ) ;
#53647 = EDGE_LOOP ( 'NONE', ( #1773, #14706, #39379, #17623 ) ) ;
#53648 = VERTEX_POINT ( 'NONE', #53621 ) ;
#53649 = LINE ( 'NONE', #27258, #6918 ) ;
#53650 = PRODUCT_DEFINITION_SHAPE ( 'NONE', 'NONE',  #25667 ) ;
#53651 = LINE ( 'NONE', #10528, #4167 ) ;
#53652 = EDGE_CURVE ( 'NONE', #29145, #26892, #48533, .T. ) ;
#53653 = ADVANCED_FACE ( 'NONE', ( #36588 ), #23268, .F. ) ;
#53654 = VECTOR ( 'NONE', #49258, 999.9999999999998863 ) ;
#53655 = AXIS2_PLACEMENT_3D ( 'NONE', #40979, #36443, #35155 ) ;
#53656 = ORIENTED_EDGE ( 'NONE', *, *, #35419, .T. ) ;
#53657 = DIRECTION ( 'NONE',  ( 0.007781995580012663651, -3.146120232559066537E-19, -0.9999697198139514409 ) ) ;
#53658 = ORIENTED_EDGE ( 'NONE', *, *, #32419, .T. ) ;
#53659 = LINE ( 'NONE', #11050, #23854 ) ;
#53660 = ADVANCED_FACE ( 'NONE', ( #26666 ), #36310, .F. ) ;
#53661 = ORIENTED_EDGE ( 'NONE', *, *, #15438, .F. ) ;
#53662 = ORIENTED_EDGE ( 'NONE', *, *, #17618, .F. ) ;
#53663 = VECTOR ( 'NONE', #21487, 1000.000000000000227 ) ;
#53664 = ORIENTED_EDGE ( 'NONE', *, *, #3415, .T. ) ;
#53665 = CARTESIAN_POINT ( 'NONE',  ( -23.32622135384906770, 18.90220053346460460, -4.407437592157546824 ) ) ;
#53666 = DIRECTION ( 'NONE',  ( 0.2426528472758542054, 0.7422098413412800966, 0.6246952433987894571 ) ) ;
#53667 = LINE ( 'NONE', #36939, #27555 ) ;
#53668 = ORIENTED_EDGE ( 'NONE', *, *, #17035, .T. ) ;
#53669 = VECTOR ( 'NONE', #51021, 1000.000000000000227 ) ;
#53670 = ORIENTED_EDGE ( 'NONE', *, *, #14710, .T. ) ;
#53671 = VECTOR ( 'NONE', #7053, 1000.000000000000227 ) ;
#53672 = PLANE ( 'NONE',  #13696 ) ;
#53673 = ORIENTED_EDGE ( 'NONE', *, *, #38203, .T. ) ;
#53674 = PLANE ( 'NONE',  #55456 ) ;
#53675 = ORIENTED_EDGE ( 'NONE', *, *, #10469, .F. ) ;
#53676 = CARTESIAN_POINT ( 'NONE',  ( -19.60834386242827776, 0.000000000000000000, 4.298478389818581213 ) ) ;
#53677 = DIRECTION ( 'NONE',  ( 0.005961354470445682716, -0.6427876096865404731, -0.7660212471507180654 ) ) ;
#53678 = EDGE_LOOP ( 'NONE', ( #28792, #7506, #31415, #95 ) ) ;
#53679 = CARTESIAN_POINT ( 'NONE',  ( -16.48635313129300783, 3.362543313726510164, 2.978508430039266575 ) ) ;
#53680 = EDGE_CURVE ( 'NONE', #23095, #21318, #18142, .T. ) ;
#53681 = FACE_OUTER_BOUND ( 'NONE', #18375, .T. ) ;
#53683 = EDGE_CURVE ( 'NONE', #8893, #43254, #5109, .T. ) ;
#53682 = ORIENTED_EDGE ( 'NONE', *, *, #48786, .T. ) ;
#53684 = CARTESIAN_POINT ( 'NONE',  ( -17.21704052607717728, 0.000000000000000000, 7.471750679991184363 ) ) ;
#53685 = CARTESIAN_POINT ( 'NONE',  ( -18.33481204970100364, 0.000000000000000000, 5.985723644308105662 ) ) ;
#53686 = FACE_OUTER_BOUND ( 'NONE', #41704, .T. ) ;
#53687 = EDGE_LOOP ( 'NONE', ( #28817, #2646, #17952, #55935 ) ) ;
#53688 = VECTOR ( 'NONE', #46375, 999.9999999999998863 ) ;
#53689 = AXIS2_PLACEMENT_3D ( 'NONE', #44911, #6028, #19628 ) ;
#53690 = LINE ( 'NONE', #14806, #50037 ) ;
#53691 = DIRECTION ( 'NONE',  ( 0.6427681459581294776, -0.7660444431189769032, 0.005002170337467562802 ) ) ;
#53692 = EDGE_CURVE ( 'NONE', #23668, #29674, #13880, .T. ) ;
#53693 = LINE ( 'NONE', #39815, #45726 ) ;
#53694 = PLANE ( 'NONE',  #5071 ) ;
#53695 = LINE ( 'NONE', #35847, #34910 ) ;
#53696 = DIRECTION ( 'NONE',  ( -0.005961354470445682716, -0.6427876096865404731, 0.7660212471507180654 ) ) ;
#53697 = AXIS2_PLACEMENT_3D ( 'NONE', #25196, #46446, #28595 ) ;
#53698 = CARTESIAN_POINT ( 'NONE',  ( -68.68338454767959433, -9.704603335163470845, 6.496570960383161619 ) ) ;
#53699 = VECTOR ( 'NONE', #32066, 1000.000000000000114 ) ;
#53700 = ORIENTED_EDGE ( 'NONE', *, *, #32645, .F. ) ;
#53701 = LINE ( 'NONE', #32143, #5357 ) ;
#53702 = DIRECTION ( 'NONE',  ( 0.9999697198139515519, 0.000000000000000000, 0.007781995580013368816 ) ) ;
#53703 = CARTESIAN_POINT ( 'NONE',  ( -67.09538265911608335, -0.6008884158751092164, 1.362417606695038641 ) ) ;
#53704 = ORIENTED_EDGE ( 'NONE', *, *, #49108, .F. ) ;
#53705 = FACE_OUTER_BOUND ( 'NONE', #4040, .T. ) ;
#53706 = DIRECTION ( 'NONE',  ( -0.5364919789714478471, 0.6444004775717705469, -0.5449076811759709926 ) ) ;
#53707 = CARTESIAN_POINT ( 'NONE',  ( -14.94838282604900748, -0.1191753592594197858, 2.588085963191248506 ) ) ;
#53708 = VECTOR ( 'NONE', #50422, 1000.000000000000114 ) ;
#53709 = DIRECTION ( 'NONE',  ( 0.000000000000000000, -0.000000000000000000, -1.000000000000000000 ) ) ;
#53710 = CARTESIAN_POINT ( 'NONE',  ( 2.072287782118878319, 0.000000000000000000, -2.950529333540147015 ) ) ;
#53711 = ORIENTED_EDGE ( 'NONE', *, *, #34376, .T. ) ;
#53712 = EDGE_LOOP ( 'NONE', ( #43482, #23839, #4972, #29698 ) ) ;
#53713 = CARTESIAN_POINT ( 'NONE',  ( -13.27065584551087163, 0.000000000000000000, 12.04557950825129176 ) ) ;
#53714 = FACE_OUTER_BOUND ( 'NONE', #9753, .T. ) ;
#53715 = CARTESIAN_POINT ( 'NONE',  ( -14.10280672071693431, -0.1191753592594197858, 12.40843558753103792 ) ) ;
#53716 = EDGE_CURVE ( 'NONE', #3230, #1428, #3358, .T. ) ;
#53717 = VERTEX_POINT ( 'NONE', #37147 ) ;
#53718 = CARTESIAN_POINT ( 'NONE',  ( -15.18036940317838557, -3.108426967578159061, 7.679960954172225129 ) ) ;
#53719 = VECTOR ( 'NONE', #54754, 1000.000000000000000 ) ;
#53720 = EDGE_LOOP ( 'NONE', ( #30125, #46519, #23994, #28112 ) ) ;
#53721 = PLANE ( 'NONE',  #51905 ) ;
#53722 = ADVANCED_FACE ( 'NONE', ( #50194 ), #11302, .F. ) ;
#53723 = EDGE_CURVE ( 'NONE', #46605, #12378, #33449, .T. ) ;
#53724 = ORIENTED_EDGE ( 'NONE', *, *, #9954, .F. ) ;
#53725 = DIRECTION ( 'NONE',  ( 0.5364919789714477361, 0.6444004775717706579, 0.5449076811759711036 ) ) ;
#53726 = VECTOR ( 'NONE', #8634, 999.9999999999998863 ) ;
#53727 = CARTESIAN_POINT ( 'NONE',  ( -15.13495153988577968, 0.000000000000000000, 12.76973526769478084 ) ) ;
#53728 = PLANE ( 'NONE',  #55681 ) ;
#53729 = ORIENTED_EDGE ( 'NONE', *, *, #24138, .T. ) ;
#53730 = AXIS2_PLACEMENT_3D ( 'NONE', #48796, #19217, #5908 ) ;
#53731 = VECTOR ( 'NONE', #55889, 999.9999999999998863 ) ;
#53732 = LINE ( 'NONE', #22544, #41942 ) ;
#53733 = EDGE_LOOP ( 'NONE', ( #32361, #15055, #38392, #25742 ) ) ;
#53734 = EDGE_CURVE ( 'NONE', #21318, #30192, #28911, .T. ) ;
#53735 = ORIENTED_EDGE ( 'NONE', *, *, #12638, .F. ) ;
#53736 = VECTOR ( 'NONE', #49827, 1000.000000000000000 ) ;
#53737 = EDGE_LOOP ( 'NONE', ( #37449, #22554, #7575, #33514 ) ) ;
#53738 = DIRECTION ( 'NONE',  ( 0.007781995580012662783, 0.000000000000000000, -0.9999697198139514409 ) ) ;
#53739 = VECTOR ( 'NONE', #8454, 999.9999999999998863 ) ;
#53740 = VERTEX_POINT ( 'NONE', #15545 ) ;
#53741 = FACE_OUTER_BOUND ( 'NONE', #7117, .T. ) ;
#53742 = ORIENTED_EDGE ( 'NONE', *, *, #11624, .F. ) ;
#53743 = CARTESIAN_POINT ( 'NONE',  ( -12.60458797795435615, 0.000000000000000000, 11.86609696750642229 ) ) ;
#53744 = DIRECTION ( 'NONE',  ( -0.005961354470445682716, -0.6427876096865404731, 0.7660212471507180654 ) ) ;
#53745 = ORIENTED_EDGE ( 'NONE', *, *, #23595, .T. ) ;
#53747 = VECTOR ( 'NONE', #40849, 999.9999999999998863 ) ;
#53746 = DIRECTION ( 'NONE',  ( -0.7660212471507179544, -0.6427876096865405842, -0.005961354470445141482 ) ) ;
#53748 = VERTEX_POINT ( 'NONE', #24361 ) ;
#53749 = AXIS2_PLACEMENT_3D ( 'NONE', #28452, #14849, #10618 ) ;
#53750 = FACE_OUTER_BOUND ( 'NONE', #23905, .T. ) ;
#53751 = CARTESIAN_POINT ( 'NONE',  ( -10.21299843139749441, 0.000000000000000000, 3.094272917418156243 ) ) ;
#53752 = DIRECTION ( 'NONE',  ( -0.005961354470445682716, -0.6427876096865404731, 0.7660212471507180654 ) ) ;
#53753 = CARTESIAN_POINT ( 'NONE',  ( -20.14739655590154754, -0.1941918491731548790, 4.826566670133699333 ) ) ;
#53754 = FACE_OUTER_BOUND ( 'NONE', #7529, .T. ) ;
#53755 = DIRECTION ( 'NONE',  ( 0.000000000000000000, -1.000000000000000000, 0.000000000000000000 ) ) ;
#53756 = VERTEX_POINT ( 'NONE', #11011 ) ;
#53757 = VECTOR ( 'NONE', #52232, 1000.000000000000227 ) ;
#53758 = ORIENTED_EDGE ( 'NONE', *, *, #12443, .F. ) ;
#53759 = CARTESIAN_POINT ( 'NONE',  ( -28.92982233430281980, 0.000000000000000000, 7.919257187036034651 ) ) ;
#53760 = EDGE_CURVE ( 'NONE', #37629, #16305, #10760, .T. ) ;
#53761 = CARTESIAN_POINT ( 'NONE',  ( -12.30984162412481631, 0.000000000000000000, 7.999934106455091509 ) ) ;
#53762 = VECTOR ( 'NONE', #36339, 999.9999999999998863 ) ;
#53763 = LINE ( 'NONE', #45807, #39698 ) ;
#53764 = CARTESIAN_POINT ( 'NONE',  ( -10.41718408325484724, 0.000000000000000000, 3.631341980854890572 ) ) ;
#53765 = VERTEX_POINT ( 'NONE', #20677 ) ;
#53766 = CARTESIAN_POINT ( 'NONE',  ( -18.67775241435682432, 0.000000000000000000, 4.136394454059623804 ) ) ;
#53767 = PLANE ( 'NONE',  #32311 ) ;
#53768 = ORIENTED_EDGE ( 'NONE', *, *, #26651, .F. ) ;
#53770 = PLANE ( 'NONE',  #38376 ) ;
#53769 = VECTOR ( 'NONE', #12548, 999.9999999999998863 ) ;
#53771 = PLANE ( 'NONE',  #52150 ) ;
#53772 = ORIENTED_EDGE ( 'NONE', *, *, #19211, .T. ) ;
#53773 = EDGE_CURVE ( 'NONE', #16343, #12677, #46206, .T. ) ;
#53774 = VECTOR ( 'NONE', #33454, 999.9999999999998863 ) ;
#53775 = VECTOR ( 'NONE', #25557, 999.9999999999998863 ) ;
#53776 = CARTESIAN_POINT ( 'NONE',  ( -67.50725361308181505, -1.000000000000000000, 2.158836163547857900 ) ) ;
#53777 = DIRECTION ( 'NONE',  ( 0.6427681459581294776, -0.7660444431189769032, 0.005002170337467562802 ) ) ;
#53778 = LINE ( 'NONE', #19420, #54923 ) ;
#53779 = EDGE_CURVE ( 'NONE', #25423, #43329, #19826, .T. ) ;
#53780 = EDGE_CURVE ( 'NONE', #37968, #40926, #15838, .T. ) ;
#53781 = DIRECTION ( 'NONE',  ( 0.005961354470445682716, -0.6427876096865404731, -0.7660212471507180654 ) ) ;
#53782 = DIRECTION ( 'NONE',  ( 0.9999697198139515519, 0.000000000000000000, 0.007781995580013368816 ) ) ;
#53783 = ORIENTED_EDGE ( 'NONE', *, *, #47852, .F. ) ;
#53784 = VECTOR ( 'NONE', #44038, 1000.000000000000000 ) ;
#53785 = VECTOR ( 'NONE', #54001, 1000.000000000000227 ) ;
#53786 = EDGE_LOOP ( 'NONE', ( #49379, #2190, #24196, #14959 ) ) ;
#53787 = DIRECTION ( 'NONE',  ( 0.007781995580012663651, 0.000000000000000000, -0.9999697198139515519 ) ) ;
#53788 = DIRECTION ( 'NONE',  ( -0.7660212471507179544, -0.6427876096865405842, -0.005961354470445141482 ) ) ;
#53789 = CARTESIAN_POINT ( 'NONE',  ( -17.41260401741867625, 0.000000000000000000, 6.900890633654627848 ) ) ;
#53790 = ADVANCED_FACE ( 'NONE', ( #6488 ), #2211, .F. ) ;
#53791 = DIRECTION ( 'NONE',  ( 0.9999697198139515519, 0.000000000000000000, 0.007781995580013368816 ) ) ;
#53792 = EDGE_CURVE ( 'NONE', #1003, #18912, #45373, .T. ) ;
#53793 = VECTOR ( 'NONE', #48818, 1000.000000000000227 ) ;
#53794 = DIRECTION ( 'NONE',  ( 0.005002170337468016433, -0.7660444431189770143, -0.6427681459581293666 ) ) ;
#53795 = ORIENTED_EDGE ( 'NONE', *, *, #7854, .F. ) ;
#53797 = AXIS2_PLACEMENT_3D ( 'NONE', #3873, #21200, #55857 ) ;
#53796 = CARTESIAN_POINT ( 'NONE',  ( 5.282355347525632183, -1.069580340602398705, -2.393146392891059460 ) ) ;
#53798 = EDGE_CURVE ( 'NONE', #44163, #20837, #23794, .T. ) ;
#53799 = CARTESIAN_POINT ( 'NONE',  ( -14.42921914503065750, 0.000000000000000000, 7.493446150599242017 ) ) ;
#53800 = LINE ( 'NONE', #22865, #31465 ) ;
#53801 = ORIENTED_EDGE ( 'NONE', *, *, #25576, .T. ) ;
#53802 = CARTESIAN_POINT ( 'NONE',  ( -67.72739005747112628, -11.31115511663740136, 7.469119143268238226 ) ) ;
#53803 = ORIENTED_EDGE ( 'NONE', *, *, #42452, .T. ) ;
#53804 = DIRECTION ( 'NONE',  ( -0.6427681459581293666, -0.7660444431189770143, -0.005002170337467561935 ) ) ;
#53805 = VECTOR ( 'NONE', #50036, 999.9999999999998863 ) ;
#53806 = CARTESIAN_POINT ( 'NONE',  ( -11.67244013076689946, 0.000000000000000000, 11.50401908778467863 ) ) ;
#53807 = EDGE_CURVE ( 'NONE', #37343, #8607, #41943, .T. ) ;
#53808 = EDGE_LOOP ( 'NONE', ( #48055, #56229, #56208, #6410 ) ) ;
#53809 = PLANE ( 'NONE',  #19947 ) ;
#53810 = VECTOR ( 'NONE', #918, 999.9999999999998863 ) ;
#53811 = ORIENTED_EDGE ( 'NONE', *, *, #26952, .F. ) ;
#53812 = EDGE_CURVE ( 'NONE', #20216, #43832, #7313, .T. ) ;
#53813 = ORIENTED_EDGE ( 'NONE', *, *, #3453, .F. ) ;
#53814 = ORIENTED_EDGE ( 'NONE', *, *, #37251, .F. ) ;
#53815 = PLANE ( 'NONE',  #16653 ) ;
#53816 = ORIENTED_EDGE ( 'NONE', *, *, #15748, .T. ) ;
#53817 = ORIENTED_EDGE ( 'NONE', *, *, #49477, .T. ) ;
#53818 = VECTOR ( 'NONE', #50928, 999.9999999999998863 ) ;
#53819 = LINE ( 'NONE', #5859, #51027 ) ;
#53820 = PLANE ( 'NONE',  #48511 ) ;
#53821 = ORIENTED_EDGE ( 'NONE', *, *, #46679, .F. ) ;
#53822 = VECTOR ( 'NONE', #8593, 1000.000000000000000 ) ;
#53823 = AXIS2_PLACEMENT_3D ( 'NONE', #24644, #11030, #37160 ) ;
#53824 = EDGE_LOOP ( 'NONE', ( #50402, #22184, #23181, #22772 ) ) ;
#53825 = LINE ( 'NONE', #41863, #35870 ) ;
#53826 = VERTEX_POINT ( 'NONE', #29172 ) ;
#53827 = ORIENTED_EDGE ( 'NONE', *, *, #52400, .T. ) ;
#53828 = VECTOR ( 'NONE', #2775, 1000.000000000000114 ) ;
#53829 = LINE ( 'NONE', #53551, #3091 ) ;
#53830 = CARTESIAN_POINT ( 'NONE',  ( 2.072287782118878319, 0.000000000000000000, -2.950529333540147015 ) ) ;
#53831 = LINE ( 'NONE', #40786, #28701 ) ;
#53832 = FACE_OUTER_BOUND ( 'NONE', #17740, .T. ) ;
#53833 = ORIENTED_EDGE ( 'NONE', *, *, #23294, .T. ) ;
#53834 = PLANE ( 'NONE',  #54633 ) ;
#53835 = ORIENTED_EDGE ( 'NONE', *, *, #5487, .F. ) ;
#53836 = ADVANCED_FACE ( 'NONE', ( #45954 ), #24092, .F. ) ;
#53837 = CARTESIAN_POINT ( 'NONE',  ( -13.47407886980094283, 0.000000000000000000, 4.176890644815381748 ) ) ;
#53838 = CARTESIAN_POINT ( 'NONE',  ( -39.69590723381624997, 9.739833118710683024, -4.961795781091632662 ) ) ;
#53839 = DIRECTION ( 'NONE',  ( 0.000000000000000000, -0.000000000000000000, -1.000000000000000000 ) ) ;
#53840 = VECTOR ( 'NONE', #8655, 1000.000000000000000 ) ;
#53841 = CARTESIAN_POINT ( 'NONE',  ( 5.204999356530673360, -6.244963811491317074, 2.061810099490656079 ) ) ;
#53842 = LINE ( 'NONE', #14958, #4126 ) ;
#53843 = ORIENTED_EDGE ( 'NONE', *, *, #21017, .F. ) ;
#53844 = DIRECTION ( 'NONE',  ( -0.7660212471507179544, -0.6427876096865405842, -0.005961354470445141482 ) ) ;
#53845 = VECTOR ( 'NONE', #9648, 1000.000000000000000 ) ;
#53846 = EDGE_LOOP ( 'NONE', ( #36574, #16408, #41537, #20281 ) ) ;
#53847 = PLANE ( 'NONE',  #46471 ) ;
#53848 = CARTESIAN_POINT ( 'NONE',  ( -19.30918475015224800, -5.213152330870663320, 12.73794594145227776 ) ) ;
#53849 = DIRECTION ( 'NONE',  ( 0.007781995580012662783, 0.000000000000000000, -0.9999697198139514409 ) ) ;
#53850 = AXIS2_PLACEMENT_3D ( 'NONE', #5050, #39693, #51612 ) ;
#53851 = DIRECTION ( 'NONE',  ( -0.7660212471507179544, -0.6427876096865405842, -0.005961354470445141482 ) ) ;
#53852 = EDGE_CURVE ( 'NONE', #36594, #48082, #45652, .T. ) ;
#53853 = DIRECTION ( 'NONE',  ( 0.007781995580012662783, 0.000000000000000000, -0.9999697198139514409 ) ) ;
#53854 = VERTEX_POINT ( 'NONE', #37992 ) ;
#53855 = VECTOR ( 'NONE', #42372, 999.9999999999998863 ) ;
#53856 = DIRECTION ( 'NONE',  ( -1.000000000000000000, 0.000000000000000000, 0.000000000000000000 ) ) ;
#53857 = DIRECTION ( 'NONE',  ( 0.7660212471507180654, -0.6427876096865404731, 0.005961354470445141482 ) ) ;
#53858 = LINE ( 'NONE', #35720, #30937 ) ;
#53859 = LINE ( 'NONE', #1052, #5592 ) ;
#53860 = EDGE_CURVE ( 'NONE', #25200, #15209, #7063, .T. ) ;
#53861 = DIRECTION ( 'NONE',  ( -0.5449076811759708816, 0.6444004775717707689, 0.5364919789714475140 ) ) ;
#53862 = DIRECTION ( 'NONE',  ( 0.6427681459581294776, -0.7660444431189769032, 0.005002170337467562802 ) ) ;
#53863 = CARTESIAN_POINT ( 'NONE',  ( -12.06867196525655572, 0.000000000000000000, 2.710499567088351824 ) ) ;
#53864 = EDGE_CURVE ( 'NONE', #53290, #26301, #55041, .T. ) ;
#53865 = VECTOR ( 'NONE', #30830, 999.9999999999998863 ) ;
#53866 = AXIS2_PLACEMENT_3D ( 'NONE', #19143, #6128, #36467 ) ;
#53867 = DIRECTION ( 'NONE',  ( -0.5449076811759708816, 0.6444004775717707689, 0.5364919789714475140 ) ) ;
#53868 = LINE ( 'NONE', #40822, #5679 ) ;
#53869 = ORIENTED_EDGE ( 'NONE', *, *, #27602, .T. ) ;
#53870 = EDGE_CURVE ( 'NONE', #32666, #15482, #39398, .T. ) ;
#53871 = ORIENTED_EDGE ( 'NONE', *, *, #40083, .T. ) ;
#53872 = AXIS2_PLACEMENT_3D ( 'NONE', #2969, #54129, #15233 ) ;
#53873 = ADVANCED_FACE ( 'NONE', ( #16386 ), #34559, .F. ) ;
#53874 = ORIENTED_EDGE ( 'NONE', *, *, #1630, .F. ) ;
#53875 = ORIENTED_EDGE ( 'NONE', *, *, #51483, .T. ) ;
#53876 = EDGE_LOOP ( 'NONE', ( #41806, #10929, #30892 ) ) ;
#53877 = VECTOR ( 'NONE', #41781, 1000.000000000000114 ) ;
#53878 = ORIENTED_EDGE ( 'NONE', *, *, #30429, .T. ) ;
#53879 = CARTESIAN_POINT ( 'NONE',  ( -14.01701317841955508, 0.000000000000000000, 2.326005055450897085 ) ) ;
#53880 = DIRECTION ( 'NONE',  ( 0.9999697198139515519, 0.000000000000000000, 0.007781995580013368816 ) ) ;
#53881 = AXIS2_PLACEMENT_3D ( 'NONE', #12649, #25698, #38780 ) ;
#53882 = ORIENTED_EDGE ( 'NONE', *, *, #49936, .F. ) ;
#53883 = LINE ( 'NONE', #24346, #38571 ) ;
#53884 = ORIENTED_EDGE ( 'NONE', *, *, #53335, .F. ) ;
#53885 = DIRECTION ( 'NONE',  ( 0.000000000000000000, -1.000000000000000000, 0.000000000000000000 ) ) ;
#53886 = VECTOR ( 'NONE', #32590, 1000.000000000000227 ) ;
#53887 = CARTESIAN_POINT ( 'NONE',  ( -13.29153558808963531, -0.3560938001956556742, 2.032843665462120697 ) ) ;
#53888 = DIRECTION ( 'NONE',  ( -0.7660212471507179544, -0.6427876096865405842, -0.005961354470445141482 ) ) ;
#53889 = VERTEX_POINT ( 'NONE', #30616 ) ;
#53890 = LINE ( 'NONE', #45121, #40985 ) ;
#53891 = EDGE_CURVE ( 'NONE', #22114, #349, #16684, .T. ) ;
#53892 = VECTOR ( 'NONE', #16136, 1000.000000000000227 ) ;
#53893 = CARTESIAN_POINT ( 'NONE',  ( -11.84139170794692930, 0.000000000000000000, 7.513585222091296423 ) ) ;
#53894 = ADVANCED_FACE ( 'NONE', ( #25770 ), #55576, .F. ) ;
#53895 = CARTESIAN_POINT ( 'NONE',  ( -27.06630483948590893, -0.1191753592594197858, 7.295098399573937797 ) ) ;
#53896 = VECTOR ( 'NONE', #16095, 999.9999999999998863 ) ;
#53897 = DIRECTION ( 'NONE',  ( 0.005002170337468016433, -0.7660444431189770143, -0.6427681459581293666 ) ) ;
#53898 = CARTESIAN_POINT ( 'NONE',  ( -22.40556560354864146, -0.1191753592594197858, 5.484709000965211523 ) ) ;
#53899 = VECTOR ( 'NONE', #16159, 999.9999999999998863 ) ;
#53900 = ADVANCED_FACE ( 'NONE', ( #8443 ), #17526, .F. ) ;
#53901 = CARTESIAN_POINT ( 'NONE',  ( -21.47341775636118655, -0.1191753592594197858, 5.122631121243466090 ) ) ;
#53902 = LINE ( 'NONE', #24363, #52855 ) ;
#53903 = FACE_OUTER_BOUND ( 'NONE', #23562, .T. ) ;
#53904 = EDGE_CURVE ( 'NONE', #13033, #14383, #33712, .T. ) ;
#53905 = DIRECTION ( 'NONE',  ( 0.007781995580012662783, 0.000000000000000000, -0.9999697198139514409 ) ) ;
#53906 = ORIENTED_EDGE ( 'NONE', *, *, #28600, .F. ) ;
#53907 = CARTESIAN_POINT ( 'NONE',  ( 4.866417447938704122, 0.000000000000000000, 1.967953638241001002 ) ) ;
#53908 = EDGE_LOOP ( 'NONE', ( #30909, #26661, #32735, #42444 ) ) ;
#53909 = EDGE_CURVE ( 'NONE', #5827, #31801, #34017, .T. ) ;
#53910 = ADVANCED_FACE ( 'NONE', ( #51339 ), #56154, .F. ) ;
#53911 = EDGE_CURVE ( 'NONE', #24424, #15522, #4211, .T. ) ;
#53912 = FACE_OUTER_BOUND ( 'NONE', #49101, .T. ) ;
#53913 = CARTESIAN_POINT ( 'NONE',  ( -15.93792926431930645, -1.813211359398158473, 5.848553459476834249 ) ) ;
#53914 = DIRECTION ( 'NONE',  ( 0.007781995580012662783, 0.000000000000000000, -0.9999697198139514409 ) ) ;
#53915 = CARTESIAN_POINT ( 'NONE',  ( -10.44460696391839427, 0.000000000000000000, 7.155123254137559563 ) ) ;
#53916 = CARTESIAN_POINT ( 'NONE',  ( -31.72626587586518099, 0.000000000000000000, 9.005490826201270949 ) ) ;
#53917 = LINE ( 'NONE', #16146, #47677 ) ;
#53918 = CARTESIAN_POINT ( 'NONE',  ( -16.79925329029790149, 0.000000000000000000, 13.49544742625427496 ) ) ;
#53919 = VECTOR ( 'NONE', #36542, 1000.000000000000000 ) ;
#53920 = DIRECTION ( 'NONE',  ( 0.5364919789714477361, 0.6444004775717706579, 0.5449076811759711036 ) ) ;
#53921 = VECTOR ( 'NONE', #2817, 1000.000000000000227 ) ;
#53922 = CARTESIAN_POINT ( 'NONE',  ( -26.13415699229845757, -0.1191753592594197858, 6.933020519852192365 ) ) ;
#53923 = DIRECTION ( 'NONE',  ( -0.6427681459581293666, -0.7660444431189770143, -0.005002170337467561935 ) ) ;
#53924 = CARTESIAN_POINT ( 'NONE',  ( -31.72782227498118601, 0.000000000000000000, 9.205484770164058972 ) ) ;
#53925 = PLANE ( 'NONE',  #4639 ) ;
#53926 = VECTOR ( 'NONE', #27889, 1000.000000000000114 ) ;
#53927 = FACE_OUTER_BOUND ( 'NONE', #35755, .T. ) ;
#53928 = DIRECTION ( 'NONE',  ( -0.6427681459581293666, -0.7660444431189770143, -0.005002170337467561935 ) ) ;
#53929 = EDGE_CURVE ( 'NONE', #36681, #5037, #38843, .T. ) ;
#53930 = VECTOR ( 'NONE', #37410, 1000.000000000000227 ) ;
#53931 = CARTESIAN_POINT ( 'NONE',  ( -10.00813838035478298, 0.000000000000000000, 10.77830692922518452 ) ) ;
#53932 = CARTESIAN_POINT ( 'NONE',  ( -12.60458797795435615, 0.000000000000000000, 11.86609696750642229 ) ) ;
#53933 = CARTESIAN_POINT ( 'NONE',  ( -19.63737892770141613, -0.1191753592594169270, 7.087566515900918240 ) ) ;
#53934 = VERTEX_POINT ( 'NONE', #51608 ) ;
#53935 = EDGE_CURVE ( 'NONE', #6267, #53765, #26072, .T. ) ;
#53936 = VECTOR ( 'NONE', #54043, 999.9999999999998863 ) ;
#53937 =( GEOMETRIC_REPRESENTATION_CONTEXT ( 3 ) GLOBAL_UNCERTAINTY_ASSIGNED_CONTEXT ( ( #28019 ) ) GLOBAL_UNIT_ASSIGNED_CONTEXT ( ( #43780, #52587, #31300 ) ) REPRESENTATION_CONTEXT ( 'NONE', 'WORKASPACE' ) );
#53938 = ORIENTED_EDGE ( 'NONE', *, *, #49432, .F. ) ;
#53939 = ADVANCED_FACE ( 'NONE', ( #47920 ), #179, .F. ) ;
#53940 = LINE ( 'NONE', #23564, #19546 ) ;
#53941 = VECTOR ( 'NONE', #18335, 999.9999999999998863 ) ;
#53942 = LINE ( 'NONE', #32914, #49391 ) ;
#53943 = VECTOR ( 'NONE', #49460, 999.9999999999998863 ) ;
#53944 = EDGE_CURVE ( 'NONE', #37711, #7759, #42530, .T. ) ;
#53945 = EDGE_LOOP ( 'NONE', ( #44471, #51975, #52922 ) ) ;
#53946 = FACE_OUTER_BOUND ( 'NONE', #27363, .T. ) ;
#53947 = ORIENTED_EDGE ( 'NONE', *, *, #14977, .F. ) ;
#53948 = CARTESIAN_POINT ( 'NONE',  ( 5.592545315101208558, -1.053278153209864065, -2.323295808888600433 ) ) ;
#53949 = AXIS2_PLACEMENT_3D ( 'NONE', #26487, #22791, #39278 ) ;
#53950 = ORIENTED_EDGE ( 'NONE', *, *, #27450, .T. ) ;
#53951 = VECTOR ( 'NONE', #42723, 1000.000000000000000 ) ;
#53952 = ORIENTED_EDGE ( 'NONE', *, *, #13492, .T. ) ;
#53953 = ORIENTED_EDGE ( 'NONE', *, *, #42840, .F. ) ;
#53954 = B_SPLINE_CURVE_WITH_KNOTS ( 'NONE', 3,
 ( #46438, #20638, #7556, #29733 ),
 .UNSPECIFIED., .F., .F.,
 ( 4, 4 ),
 ( 0.0003023226855361189165, 0.0003536700609687475679 ),
 .UNSPECIFIED. ) ;
#53955 = PLANE ( 'NONE',  #21154 ) ;
#53956 = ADVANCED_FACE ( 'NONE', ( #17238 ), #43382, .F. ) ;
#53957 = DIRECTION ( 'NONE',  ( 0.5364919789714477361, 0.6444004775717706579, 0.5449076811759711036 ) ) ;
#53958 = CARTESIAN_POINT ( 'NONE',  ( -17.65581094137071361, 0.000000000000000000, 4.144347438903294822 ) ) ;
#53959 = VERTEX_POINT ( 'NONE', #38251 ) ;
#53960 = ORIENTED_EDGE ( 'NONE', *, *, #16904, .F. ) ;
#53961 = VECTOR ( 'NONE', #6958, 1000.000000000000227 ) ;
#53962 = CARTESIAN_POINT ( 'NONE',  ( -11.67244013076689946, 0.000000000000000000, 11.50401908778467863 ) ) ;
#53963 = VECTOR ( 'NONE', #38528, 1000.000000000000227 ) ;
#53964 = ORIENTED_EDGE ( 'NONE', *, *, #376, .F. ) ;
#53965 = PLANE ( 'NONE',  #36411 ) ;
#53966 = ORIENTED_EDGE ( 'NONE', *, *, #14700, .F. ) ;
#53967 = VECTOR ( 'NONE', #22448, 1000.000000000000227 ) ;
#53968 = FACE_OUTER_BOUND ( 'NONE', #5145, .T. ) ;
#53969 = CARTESIAN_POINT ( 'NONE',  ( -14.61328642235102926, 0.000000000000000000, 5.445347291231628084 ) ) ;
#53970 = ORIENTED_EDGE ( 'NONE', *, *, #29442, .T. ) ;
#53971 = DIRECTION ( 'NONE',  ( 0.000000000000000000, -0.000000000000000000, -1.000000000000000000 ) ) ;
#53972 = VECTOR ( 'NONE', #14411, 999.9999999999998863 ) ;
#53973 = LINE ( 'NONE', #49970, #49056 ) ;
#53974 = AXIS2_PLACEMENT_3D ( 'NONE', #29945, #47245, #21439 ) ;
#53975 = AXIS2_PLACEMENT_3D ( 'NONE', #49512, #15674, #23646 ) ;
#53976 = VERTEX_POINT ( 'NONE', #29770 ) ;
#53977 = CARTESIAN_POINT ( 'NONE',  ( -14.94838282604900748, -0.1191753592594197858, 2.588085963191248506 ) ) ;
#53978 = DIRECTION ( 'NONE',  ( -0.5449076811759708816, 0.6444004775717707689, 0.5364919789714475140 ) ) ;
#53979 = VECTOR ( 'NONE', #21021, 999.9999999999998863 ) ;
#53980 = LINE ( 'NONE', #14270, #1994 ) ;
#53981 = ORIENTED_EDGE ( 'NONE', *, *, #20319, .F. ) ;
#53982 = AXIS2_PLACEMENT_3D ( 'NONE', #54403, #15253, #28867 ) ;
#53983 = ADVANCED_FACE ( 'NONE', ( #52171 ), #43634, .F. ) ;
#53984 = EDGE_CURVE ( 'NONE', #27552, #11704, #31455, .T. ) ;
#53985 = VECTOR ( 'NONE', #42378, 1000.000000000000227 ) ;
#53986 = CARTESIAN_POINT ( 'NONE',  ( -14.49682332889594427, -0.1191753592594190780, 3.330264243224434040 ) ) ;
#53987 = DIRECTION ( 'NONE',  ( -0.005961354470445682716, -0.6427876096865404731, 0.7660212471507180654 ) ) ;
#53988 = CARTESIAN_POINT ( 'NONE',  ( -17.36532418587302473, -0.1191753592594177458, 13.67570816655714516 ) ) ;
#53989 = LINE ( 'NONE', #28138, #11416 ) ;
#53990 = EDGE_CURVE ( 'NONE', #47502, #47959, #53314, .T. ) ;
#53991 = DIRECTION ( 'NONE',  ( 0.5449076811759707706, 0.6444004775717708799, -0.5364919789714476250 ) ) ;
#53992 = FACE_OUTER_BOUND ( 'NONE', #23719, .T. ) ;
#53993 = VECTOR ( 'NONE', #37524, 1000.000000000000227 ) ;
#53994 = VECTOR ( 'NONE', #22839, 999.9999999999998863 ) ;
#53995 = CARTESIAN_POINT ( 'NONE',  ( -64.58775654058000271, -11.11425561933479855, -0.8023217398921337340 ) ) ;
#53996 = ORIENTED_EDGE ( 'NONE', *, *, #49750, .F. ) ;
#53997 = CARTESIAN_POINT ( 'NONE',  ( -16.54234516706728186, -1.975113310420658852, 6.349037806105066295 ) ) ;
#53998 = DIRECTION ( 'NONE',  ( -0.9999697198139514409, -0.000000000000000000, -0.007781995580013368816 ) ) ;
#53999 = CARTESIAN_POINT ( 'NONE',  ( -67.93758966355230200, -0.6009655799177398006, 4.644600239861888191 ) ) ;
#54000 = ORIENTED_EDGE ( 'NONE', *, *, #46890, .T. ) ;
#54001 = DIRECTION ( 'NONE',  ( -0.5449076811759708816, 0.6444004775717707689, 0.5364919789714475140 ) ) ;
#54002 = CARTESIAN_POINT ( 'NONE',  ( -22.40634380310664397, 0.000000000000000000, 5.584705972946605534 ) ) ;
#54003 = DIRECTION ( 'NONE',  ( 0.000000000000000000, -0.000000000000000000, -1.000000000000000000 ) ) ;
#54004 = DIRECTION ( 'NONE',  ( -0.5449076811759708816, 0.6444004775717707689, 0.5364919789714475140 ) ) ;
#54005 = EDGE_CURVE ( 'NONE', #30844, #23916, #53561, .T. ) ;
#54006 = CARTESIAN_POINT ( 'NONE',  ( -56.26331385538585295, 6.756938025167550599, 2.134183571387440637 ) ) ;
#54007 = VECTOR ( 'NONE', #22165, 1000.000000000000000 ) ;
#54008 = EDGE_LOOP ( 'NONE', ( #8394, #31863, #44773, #10191 ) ) ;
#54009 = ORIENTED_EDGE ( 'NONE', *, *, #38351, .T. ) ;
#54010 = VECTOR ( 'NONE', #50686, 999.9999999999998863 ) ;
#54011 = EDGE_CURVE ( 'NONE', #49949, #14352, #49307, .T. ) ;
#54012 = CARTESIAN_POINT ( 'NONE',  ( -13.53673582514181106, 0.000000000000000000, 12.22817484722816772 ) ) ;
#54013 = VECTOR ( 'NONE', #19970, 1000.000000000000227 ) ;
#54014 = CARTESIAN_POINT ( 'NONE',  ( -24.57312748012714820, 18.34675972927921350, -4.549864808573585329 ) ) ;
#54015 = EDGE_CURVE ( 'NONE', #2677, #1529, #18664, .T. ) ;
#54016 = ORIENTED_EDGE ( 'NONE', *, *, #26611, .F. ) ;
#54017 = CARTESIAN_POINT ( 'NONE',  ( -69.48696977452702583, -9.539949144137821690, -7.502262482362485052 ) ) ;
#54018 = AXIS2_PLACEMENT_3D ( 'NONE', #40376, #31846, #49157 ) ;
#54019 = VERTEX_POINT ( 'NONE', #39688 ) ;
#54020 = FACE_OUTER_BOUND ( 'NONE', #23372, .T. ) ;
#54021 = EDGE_CURVE ( 'NONE', #11430, #10050, #13553, .T. ) ;
#54022 = AXIS2_PLACEMENT_3D ( 'NONE', #54568, #33015, #46330 ) ;
#54023 = EDGE_LOOP ( 'NONE', ( #51069, #55329, #36141, #40440 ) ) ;
#54025 = ORIENTED_EDGE ( 'NONE', *, *, #49833, .F. ) ;
#54024 = AXIS2_PLACEMENT_3D ( 'NONE', #50932, #15738, #11507 ) ;
#54026 = CARTESIAN_POINT ( 'NONE',  ( -10.27421835998572064, 0.000000000000000000, 10.96090226820206048 ) ) ;
#54027 = PLANE ( 'NONE',  #27787 ) ;
#54028 = LINE ( 'NONE', #19673, #4902 ) ;
#54029 = VECTOR ( 'NONE', #50973, 1000.000000000000227 ) ;
#54030 = ORIENTED_EDGE ( 'NONE', *, *, #33306, .F. ) ;
#54031 = VECTOR ( 'NONE', #33101, 999.9999999999998863 ) ;
#54032 = DIRECTION ( 'NONE',  ( 0.005002170337468016433, -0.7660444431189770143, -0.6427681459581293666 ) ) ;
#54033 = VECTOR ( 'NONE', #11190, 1000.000000000000227 ) ;
#54034 = ORIENTED_EDGE ( 'NONE', *, *, #47928, .T. ) ;
#54035 = VECTOR ( 'NONE', #22256, 1000.000000000000227 ) ;
#54036 = VERTEX_POINT ( 'NONE', #14664 ) ;
#54037 = VECTOR ( 'NONE', #39960, 1000.000000000000227 ) ;
#54038 = EDGE_LOOP ( 'NONE', ( #21284, #28544, #55225, #43640 ) ) ;
#54039 = LINE ( 'NONE', #14854, #15000 ) ;
#54040 = EDGE_LOOP ( 'NONE', ( #36882, #39573, #43900, #30003 ) ) ;
#54041 = DIRECTION ( 'NONE',  ( -0.7660212471507179544, -0.6427876096865405842, -0.005961354470445141482 ) ) ;
#54042 = ORIENTED_EDGE ( 'NONE', *, *, #39299, .F. ) ;
#54043 = DIRECTION ( 'NONE',  ( 0.9999697198139515519, 0.000000000000000000, 0.007781995580013368816 ) ) ;
#54044 = DIRECTION ( 'NONE',  ( 0.007781995580012662783, 0.000000000000000000, -0.9999697198139514409 ) ) ;
#54045 = ORIENTED_EDGE ( 'NONE', *, *, #8424, .T. ) ;
#54046 = FACE_OUTER_BOUND ( 'NONE', #7299, .T. ) ;
#54047 = ORIENTED_EDGE ( 'NONE', *, *, #44454, .F. ) ;
#54048 = AXIS2_PLACEMENT_3D ( 'NONE', #54356, #40493, #23693 ) ;
#54049 = DIRECTION ( 'NONE',  ( 0.007781995580012663651, 0.000000000000000000, -0.9999697198139515519 ) ) ;
#54050 = CARTESIAN_POINT ( 'NONE',  ( -9.201257701905497299, -2.398698010759394705, 3.305331372236061327 ) ) ;
#54051 = CARTESIAN_POINT ( 'NONE',  ( -10.00813838035478298, 0.000000000000000000, 10.77830692922518452 ) ) ;
#54052 = CARTESIAN_POINT ( 'NONE',  ( -19.00053506639916989, 3.524445264749008100, 10.04598931717878507 ) ) ;
#54053 = CARTESIAN_POINT ( 'NONE',  ( -18.66354898467281132, 0.000000000000000000, 14.21960318569776582 ) ) ;
#54054 = PLANE ( 'NONE',  #41851 ) ;
#54055 = SURFACE_STYLE_FILL_AREA ( #1540 ) ;
#54056 = VECTOR ( 'NONE', #40465, 1000.000000000000227 ) ;
#54057 = ORIENTED_EDGE ( 'NONE', *, *, #6611, .T. ) ;
#54058 = EDGE_CURVE ( 'NONE', #15058, #36955, #30865, .T. ) ;
#54059 = ORIENTED_EDGE ( 'NONE', *, *, #55848, .F. ) ;
#54060 = CARTESIAN_POINT ( 'NONE',  ( -24.26986129792355129, -0.1191753592594197858, 6.208864760408702388 ) ) ;
#54061 = CARTESIAN_POINT ( 'NONE',  ( -16.39796932385352335, -0.1117717739994045917, 9.587901738430785414 ) ) ;
#54062 = VECTOR ( 'NONE', #23282, 1000.000000000000000 ) ;
#54063 = EDGE_CURVE ( 'NONE', #30544, #23505, #18357, .T. ) ;
#54064 = EDGE_CURVE ( 'NONE', #32478, #3340, #40536, .T. ) ;
#54065 = CARTESIAN_POINT ( 'NONE',  ( 5.618093201498282063, -1.050357395465043364, -2.260480044901387764 ) ) ;
#54066 = FACE_OUTER_BOUND ( 'NONE', #47828, .T. ) ;
#54067 = VECTOR ( 'NONE', #1678, 999.9999999999998863 ) ;
#54068 = AXIS2_PLACEMENT_3D ( 'NONE', #53488, #10333, #48099 ) ;
#54069 = LINE ( 'NONE', #36196, #43962 ) ;
#54070 = ORIENTED_EDGE ( 'NONE', *, *, #45423, .F. ) ;
#54071 = CARTESIAN_POINT ( 'NONE',  ( 2.072287782118878319, 0.000000000000000000, -2.950529333540147015 ) ) ;
#54072 = LINE ( 'NONE', #41562, #25946 ) ;
#54073 = ORIENTED_EDGE ( 'NONE', *, *, #56174, .F. ) ;
#54074 = CARTESIAN_POINT ( 'NONE',  ( -20.54049170961573267, 0.000000000000000000, 4.660556269540326646 ) ) ;
#54075 = DIRECTION ( 'NONE',  ( -0.000000000000000000, -0.000000000000000000, -1.000000000000000000 ) ) ;
#54076 = VERTEX_POINT ( 'NONE', #9868 ) ;
#54077 = VECTOR ( 'NONE', #2778, 1000.000000000000227 ) ;
#54078 = LINE ( 'NONE', #42119, #12567 ) ;
#54079 = CARTESIAN_POINT ( 'NONE',  ( -10.47421230394850866, 0.000000000000000000, 10.95934586908605723 ) ) ;
#54080 = VECTOR ( 'NONE', #11781, 1000.000000000000000 ) ;
#54081 = LINE ( 'NONE', #45530, #30502 ) ;
#54082 = DIRECTION ( 'NONE',  ( 0.5449076811759707706, 0.6444004775717708799, -0.5364919789714476250 ) ) ;
#54083 = AXIS2_PLACEMENT_3D ( 'NONE', #27556, #41175, #41469 ) ;
#54084 = LINE ( 'NONE', #19140, #31974 ) ;
#54085 = ORIENTED_EDGE ( 'NONE', *, *, #39608, .F. ) ;
#54086 = AXIS2_PLACEMENT_3D ( 'NONE', #32509, #23146, #1260 ) ;
#54087 = VERTEX_POINT ( 'NONE', #53012 ) ;
#54088 = LINE ( 'NONE', #32513, #12157 ) ;
#54089 = DIRECTION ( 'NONE',  ( 0.005961354470445682716, -0.6427876096865404731, -0.7660212471507180654 ) ) ;
#54090 = DIRECTION ( 'NONE',  ( -0.5449076811759708816, 0.6444004775717707689, 0.5364919789714475140 ) ) ;
#54091 = DIRECTION ( 'NONE',  ( -0.9934890585767658377, -0.1139275668495182969, 0.000000000000000000 ) ) ;
#54092 = CARTESIAN_POINT ( 'NONE',  ( -11.33809474571162568, 2.229229656569007734, 1.014908676700488677 ) ) ;
#54093 = VERTEX_POINT ( 'NONE', #52712 ) ;
#54094 = DIRECTION ( 'NONE',  ( -0.7660212471507179544, -0.6427876096865405842, -0.005961354470445141482 ) ) ;
#54095 = ADVANCED_FACE ( 'NONE', ( #27170 ), #22634, .F. ) ;
#54096 = VECTOR ( 'NONE', #28413, 1000.000000000000114 ) ;
#54097 = PLANE ( 'NONE',  #37767 ) ;
#54098 = DIRECTION ( 'NONE',  ( -0.9999697198139514409, -0.000000000000000000, -0.007781995580013368816 ) ) ;
#54099 = ORIENTED_EDGE ( 'NONE', *, *, #54626, .F. ) ;
#54100 = EDGE_CURVE ( 'NONE', #3254, #50665, #44477, .T. ) ;
#54101 = CARTESIAN_POINT ( 'NONE',  ( -16.25678841961153509, 5.305366725996514710, 2.827351461323074133 ) ) ;
#54102 = PLANE ( 'NONE',  #7803 ) ;
#54103 = ADVANCED_FACE ( 'NONE', ( #1614 ), #5044, .F. ) ;
#54104 = VECTOR ( 'NONE', #50, 1000.000000000000227 ) ;
#54105 = CARTESIAN_POINT ( 'NONE',  ( 2.072287782118878319, 0.000000000000000000, -2.950529333540147015 ) ) ;
#54106 = ORIENTED_EDGE ( 'NONE', *, *, #20117, .F. ) ;
#54107 = CARTESIAN_POINT ( 'NONE',  ( -16.99924723426068951, 0.000000000000000000, 13.49389102713827171 ) ) ;
#54108 = VECTOR ( 'NONE', #27620, 999.9999999999998863 ) ;
#54109 = ADVANCED_FACE ( 'NONE', ( #22373 ), #13817, .F. ) ;
#54110 = ORIENTED_EDGE ( 'NONE', *, *, #23636, .T. ) ;
#54111 = ORIENTED_EDGE ( 'NONE', *, *, #33536, .F. ) ;
#54112 = VECTOR ( 'NONE', #25493, 999.9999999999998863 ) ;
#54113 = VERTEX_POINT ( 'NONE', #43921 ) ;
#54114 = CARTESIAN_POINT ( 'NONE',  ( -29.54997447658847776, 15.59759012727598915, 4.743609536075380717 ) ) ;
#54115 = ORIENTED_EDGE ( 'NONE', *, *, #3606, .F. ) ;
#54116 = ORIENTED_EDGE ( 'NONE', *, *, #33811, .F. ) ;
#54117 = CARTESIAN_POINT ( 'NONE',  ( -8.839206115411215592, 0.000000000000000000, 5.690288575526534665 ) ) ;
#54118 = VERTEX_POINT ( 'NONE', #36260 ) ;
#54119 = AXIS2_PLACEMENT_3D ( 'NONE', #9018, #25225, #30028 ) ;
#54120 = ORIENTED_EDGE ( 'NONE', *, *, #21161, .T. ) ;
#54121 = DIRECTION ( 'NONE',  ( 0.005961354470445682716, -0.6427876096865404731, -0.7660212471507180654 ) ) ;
#54122 = VERTEX_POINT ( 'NONE', #35695 ) ;
#54123 = VERTEX_POINT ( 'NONE', #10423 ) ;
#54124 = EDGE_CURVE ( 'NONE', #39606, #55191, #27750, .T. ) ;
#54125 = VECTOR ( 'NONE', #41998, 999.9999999999998863 ) ;
#54126 = ORIENTED_EDGE ( 'NONE', *, *, #13964, .T. ) ;
#54127 = VECTOR ( 'NONE', #10843, 1000.000000000000227 ) ;
#54128 = DIRECTION ( 'NONE',  ( 0.2426528472758541499, 0.7422098413412800966, 0.6246952433987894571 ) ) ;
#54129 = DIRECTION ( 'NONE',  ( -0.7660212471507179544, -0.6427876096865405842, -0.005961354470445141482 ) ) ;
#54130 = CARTESIAN_POINT ( 'NONE',  ( -15.88130887279446490, 0.000000000000000000, 3.050160814894388839 ) ) ;
#54131 = CARTESIAN_POINT ( 'NONE',  ( -13.21805807743849392, 0.000000000000000000, 5.286879267240680136 ) ) ;
#54132 = ADVANCED_FACE ( 'NONE', ( #6176 ), #44225, .F. ) ;
#54133 = EDGE_LOOP ( 'NONE', ( #18365, #2533, #21430, #31492 ) ) ;
#54134 = CARTESIAN_POINT ( 'NONE',  ( 0.4518049228021099872, -3.655895688227116747, -5.998622290806042479 ) ) ;
#54135 = EDGE_LOOP ( 'NONE', ( #43664, #31508, #14183, #29600 ) ) ;
#54136 = ORIENTED_EDGE ( 'NONE', *, *, #16749, .T. ) ;
#54137 = EDGE_CURVE ( 'NONE', #46078, #46605, #49024, .T. ) ;
#54138 = LINE ( 'NONE', #45888, #27588 ) ;
#54139 = UNCERTAINTY_MEASURE_WITH_UNIT (LENGTH_MEASURE( 1.000000000000000082E-05 ), #15629, 'distance_accuracy_value', 'NONE');
#54140 = EDGE_CURVE ( 'NONE', #34394, #28247, #23736, .T. ) ;
#54141 = AXIS2_PLACEMENT_3D ( 'NONE', #17356, #38388, #46325 ) ;
#54142 = DIRECTION ( 'NONE',  ( 0.5449076811759707706, 0.6444004775717708799, -0.5364919789714476250 ) ) ;
#54143 = LINE ( 'NONE', #32557, #1317 ) ;
#54144 = CARTESIAN_POINT ( 'NONE',  ( -10.20569392527092667, 0.000000000000000000, 2.155659566939837735 ) ) ;
#54145 = DIRECTION ( 'NONE',  ( 0.007781995580012663651, 0.000000000000000000, -0.9999697198139515519 ) ) ;
#54146 = ORIENTED_EDGE ( 'NONE', *, *, #48311, .F. ) ;
#54147 = DIRECTION ( 'NONE',  ( 0.005002170337468016433, -0.7660444431189770143, -0.6427681459581293666 ) ) ;
#54148 = ORIENTED_EDGE ( 'NONE', *, *, #36821, .T. ) ;
#54149 = DIRECTION ( 'NONE',  ( 0.7660212471507180654, -0.6427876096865404731, 0.005961354470445141482 ) ) ;
#54150 = CARTESIAN_POINT ( 'NONE',  ( -14.49293978885484613, 2.067327705546506245, 5.903708077246431429 ) ) ;
#54152 = CARTESIAN_POINT ( 'NONE',  ( -11.20636620717317378, 0.000000000000000000, 11.32298014792380414 ) ) ;
#54151 = AXIS2_PLACEMENT_3D ( 'NONE', #20049, #50989, #15804 ) ;
#54153 = DIRECTION ( 'NONE',  ( 0.9999697198139515519, 0.000000000000000000, 0.007781995580013368816 ) ) ;
#54154 = CARTESIAN_POINT ( 'NONE',  ( -9.110551994824897193, -1.000000000000000000, 3.538847790438064411 ) ) ;
#54155 = EDGE_CURVE ( 'NONE', #37866, #19153, #28020, .T. ) ;
#54156 = VECTOR ( 'NONE', #10663, 999.9999999999998863 ) ;
#54157 = ORIENTED_EDGE ( 'NONE', *, *, #43739, .T. ) ;
#54158 = CARTESIAN_POINT ( 'NONE',  ( -11.63696731136285756, 0.000000000000000000, 6.945837973986745517 ) ) ;
#54159 = CARTESIAN_POINT ( 'NONE',  ( -26.13493519185646008, 0.000000000000000000, 7.033017491833586377 ) ) ;
#54160 = DIRECTION ( 'NONE',  ( 0.000000000000000000, -0.000000000000000000, -1.000000000000000000 ) ) ;
#54161 = AXIS2_PLACEMENT_3D ( 'NONE', #27107, #5807, #52394 ) ;
#54162 = CARTESIAN_POINT ( 'NONE',  ( -9.542064456761055524, 0.000000000000000000, 10.59726798936431180 ) ) ;
#54163 = PLANE ( 'NONE',  #30333 ) ;
#54164 = FACE_OUTER_BOUND ( 'NONE', #48436, .T. ) ;
#54165 = FACE_OUTER_BOUND ( 'NONE', #36224, .T. ) ;
#54166 = DIRECTION ( 'NONE',  ( 0.000000000000000000, -1.000000000000000000, 0.000000000000000000 ) ) ;
#54167 = DIRECTION ( 'NONE',  ( -0.6246952433987893460, -0.7422098413412802076, 0.2426528472758542054 ) ) ;
#54168 = ORIENTED_EDGE ( 'NONE', *, *, #40954, .T. ) ;
#54169 = EDGE_CURVE ( 'NONE', #9690, #34711, #41520, .T. ) ;
#54170 = EDGE_LOOP ( 'NONE', ( #20317, #10459, #36391, #14931 ) ) ;
#54171 = ORIENTED_EDGE ( 'NONE', *, *, #29003, .F. ) ;
#54172 = ORIENTED_EDGE ( 'NONE', *, *, #30008, .F. ) ;
#54173 = ORIENTED_EDGE ( 'NONE', *, *, #18101, .T. ) ;
#54174 = DIRECTION ( 'NONE',  ( -0.2588190451025212946, -0.9659258262890680902, 0.000000000000000000 ) ) ;
#54175 = PLANE ( 'NONE',  #32147 ) ;
#54176 = EDGE_CURVE ( 'NONE', #42837, #3166, #19771, .T. ) ;
#54177 = ORIENTED_EDGE ( 'NONE', *, *, #55833, .F. ) ;
#54178 = ORIENTED_EDGE ( 'NONE', *, *, #25472, .T. ) ;
#54179 = ORIENTED_EDGE ( 'NONE', *, *, #44636, .T. ) ;
#54180 = ADVANCED_FACE ( 'NONE', ( #7005 ), #41618, .F. ) ;
#54181 = ORIENTED_EDGE ( 'NONE', *, *, #45857, .F. ) ;
#54182 = ADVANCED_FACE ( 'NONE', ( #2699 ), #2147, .F. ) ;
#54183 = VECTOR ( 'NONE', #19430, 999.9999999999998863 ) ;
#54184 = CARTESIAN_POINT ( 'NONE',  ( -67.54131694805309394, -9.439845584445631488, 7.854170068343406363 ) ) ;
#54185 = DIRECTION ( 'NONE',  ( 0.5364919789714477361, 0.6444004775717706579, 0.5449076811759711036 ) ) ;
#54186 = DIRECTION ( 'NONE',  ( -0.5364919789714478471, 0.6444004775717705469, -0.5449076811759709926 ) ) ;
#54187 = ORIENTED_EDGE ( 'NONE', *, *, #22186, .T. ) ;
#54188 = FACE_OUTER_BOUND ( 'NONE', #4217, .T. ) ;
#54189 = AXIS2_PLACEMENT_3D ( 'NONE', #21080, #47492, #38410 ) ;
#54190 = CARTESIAN_POINT ( 'NONE',  ( -17.45025494856319170, -1.975113310420660184, 3.596576296900105163 ) ) ;
#54191 = ADVANCED_FACE ( 'NONE', ( #37346 ), #19190, .F. ) ;
#54192 = DIRECTION ( 'NONE',  ( -0.005002170337468016433, -0.7660444431189770143, 0.6427681459581293666 ) ) ;
#54193 = EDGE_CURVE ( 'NONE', #9210, #40095, #33394, .T. ) ;
#54194 = LINE ( 'NONE', #6228, #48084 ) ;
#54195 = CARTESIAN_POINT ( 'NONE',  ( -16.81190032086591302, 0.000000000000000000, 3.212244750653343583 ) ) ;
#54196 = PLANE ( 'NONE',  #21305 ) ;
#54197 = LINE ( 'NONE', #49910, #25669 ) ;
#54198 = PLANE ( 'NONE',  #45746 ) ;
#54199 = CARTESIAN_POINT ( 'NONE',  ( -17.36532418587302473, -0.1191753592594177458, 13.67570816655714516 ) ) ;
#54200 = ORIENTED_EDGE ( 'NONE', *, *, #3393, .T. ) ;
#54201 = DIRECTION ( 'NONE',  ( 0.7660212471507180654, -0.6427876096865404731, 0.005961354470445141482 ) ) ;
#54202 = ORIENTED_EDGE ( 'NONE', *, *, #20200, .T. ) ;
#54203 = ADVANCED_FACE ( 'NONE', ( #29111 ), #49608, .F. ) ;
#54204 = CARTESIAN_POINT ( 'NONE',  ( -14.43209319853593975, 0.000000000000000000, 7.862755853857006372 ) ) ;
#54205 = LINE ( 'NONE', #6783, #42271 ) ;
#54206 = DIRECTION ( 'NONE',  ( -0.6427681459581293666, -0.7660444431189770143, -0.005002170337467561935 ) ) ;
#54207 = FACE_OUTER_BOUND ( 'NONE', #25591, .T. ) ;
#54208 = FACE_OUTER_BOUND ( 'NONE', #54298, .T. ) ;
#54209 = PLANE ( 'NONE',  #53111 ) ;
#54210 = EDGE_CURVE ( 'NONE', #24728, #19918, #33112, .T. ) ;
#54211 = CARTESIAN_POINT ( 'NONE',  ( -27.99923088623136636, 0.000000000000000000, 7.757173251277078130 ) ) ;
#54212 = CARTESIAN_POINT ( 'NONE',  ( -16.43317633868556626, -0.1191753592594197858, 13.31363028683540151 ) ) ;
#54213 = DIRECTION ( 'NONE',  ( 0.000000000000000000, -0.000000000000000000, -1.000000000000000000 ) ) ;
#54214 = FACE_OUTER_BOUND ( 'NONE', #17823, .T. ) ;
#54215 = LINE ( 'NONE', #15568, #26394 ) ;
#54216 = LINE ( 'NONE', #37746, #51363 ) ;
#54217 = CARTESIAN_POINT ( 'NONE',  ( -19.99425259750860207, -1.651309408375657428, 7.158458511457326701 ) ) ;
#54218 = CARTESIAN_POINT ( 'NONE',  ( -7.113423781937636470, -8.942689712534805935, 5.981468945456855479 ) ) ;
#54219 = DIRECTION ( 'NONE',  ( 0.9321478471874540261, 0.000000000000000000, -0.3620778797217456546 ) ) ;
#54220 = LINE ( 'NONE', #6514, #41957 ) ;
#54221 = ORIENTED_EDGE ( 'NONE', *, *, #20598, .F. ) ;
#54222 = DIRECTION ( 'NONE',  ( -0.005002170337468016433, -0.7660444431189770143, 0.6427681459581293666 ) ) ;
#54223 = ORIENTED_EDGE ( 'NONE', *, *, #21905, .T. ) ;
#54224 = CARTESIAN_POINT ( 'NONE',  ( -11.22056963685719211, 0.000000000000000000, 1.239771416285661010 ) ) ;
#54225 = FACE_OUTER_BOUND ( 'NONE', #52108, .T. ) ;
#54226 = AXIS2_PLACEMENT_3D ( 'NONE', #20546, #25095, #42408 ) ;
#54227 = VERTEX_POINT ( 'NONE', #37094 ) ;
#54228 = FACE_OUTER_BOUND ( 'NONE', #4652, .T. ) ;
#54229 = EDGE_CURVE ( 'NONE', #43270, #27291, #54662, .T. ) ;
#54230 = ADVANCED_FACE ( 'NONE', ( #8375 ), #51809, .T. ) ;
#54231 = ORIENTED_EDGE ( 'NONE', *, *, #31837, .T. ) ;
#54232 = DIRECTION ( 'NONE',  ( -0.9999697198139514409, -0.000000000000000000, -0.007781995580013368816 ) ) ;
#54233 = ORIENTED_EDGE ( 'NONE', *, *, #35323, .T. ) ;
#54234 = VERTEX_POINT ( 'NONE', #37929 ) ;
#54235 = ORIENTED_EDGE ( 'NONE', *, *, #48483, .F. ) ;
#54236 = PLANE ( 'NONE',  #37482 ) ;
#54237 = CARTESIAN_POINT ( 'NONE',  ( -18.67280312195969216, 3.686347215771509145, 10.18439578408527346 ) ) ;
#54238 = CARTESIAN_POINT ( 'NONE',  ( -11.79959855975697103, 0.000000000000000000, 2.143255432519805659 ) ) ;
#54239 = EDGE_CURVE ( 'NONE', #27973, #5087, #12650, .T. ) ;
#54240 = EDGE_CURVE ( 'NONE', #37866, #30714, #30249, .T. ) ;
#54241 = EDGE_CURVE ( 'NONE', #31, #30596, #29711, .T. ) ;
#54242 = ORIENTED_EDGE ( 'NONE', *, *, #17153, .F. ) ;
#54243 = ORIENTED_EDGE ( 'NONE', *, *, #42139, .F. ) ;
#54244 = EDGE_CURVE ( 'NONE', #156, #38273, #4418, .T. ) ;
#54245 = CARTESIAN_POINT ( 'NONE',  ( -27.06708303904391144, 0.000000000000000000, 7.395095371555332697 ) ) ;
#54246 = EDGE_LOOP ( 'NONE', ( #17785, #43339, #16360, #33505 ) ) ;
#54247 = PLANE ( 'NONE',  #16454 ) ;
#54248 = ORIENTED_EDGE ( 'NONE', *, *, #54402, .T. ) ;
#54249 = DIRECTION ( 'NONE',  ( 0.9999697198139515519, 0.000000000000000000, 0.007781995580013368816 ) ) ;
#54250 = CARTESIAN_POINT ( 'NONE',  ( -11.25298721152418935, -0.1191753592594192307, 4.463504735373795995 ) ) ;
#54251 = ORIENTED_EDGE ( 'NONE', *, *, #36134, .F. ) ;
#54252 = DIRECTION ( 'NONE',  ( 0.6427681459581294776, -0.7660444431189769032, 0.005002170337467562802 ) ) ;
#54253 = ADVANCED_FACE ( 'NONE', ( #20868 ), #47858, .F. ) ;
#54254 = EDGE_CURVE ( 'NONE', #8862, #21764, #25699, .T. ) ;
#54255 = DIRECTION ( 'NONE',  ( -0.005961354470445682716, -0.6427876096865404731, 0.7660212471507180654 ) ) ;
#54256 = EDGE_LOOP ( 'NONE', ( #43557, #39922, #55499, #26577 ) ) ;
#54257 = DIRECTION ( 'NONE',  ( 0.7660212471507180654, -0.6427876096865404731, 0.005961354470445141482 ) ) ;
#54258 = FACE_OUTER_BOUND ( 'NONE', #30653, .T. ) ;
#54259 = EDGE_CURVE ( 'NONE', #23248, #24915, #39040, .T. ) ;
#54260 = DIRECTION ( 'NONE',  ( 0.007781995580012662783, 0.000000000000000000, -0.9999697198139514409 ) ) ;
#54261 = ORIENTED_EDGE ( 'NONE', *, *, #47919, .F. ) ;
#54262 = EDGE_CURVE ( 'NONE', #34537, #39978, #16325, .T. ) ;
#54263 = AXIS2_PLACEMENT_3D ( 'NONE', #22005, #422, #38792 ) ;
#54264 = CARTESIAN_POINT ( 'NONE',  ( -16.00144900586372287, 0.000000000000000000, 4.695880149412071880 ) ) ;
#54265 = CARTESIAN_POINT ( 'NONE',  ( -13.66102020062660038, 0.000000000000000000, 2.498101488705531725 ) ) ;
#54266 = CARTESIAN_POINT ( 'NONE',  ( -18.66354898467281132, 0.000000000000000000, 14.21960318569776582 ) ) ;
#54267 = DIRECTION ( 'NONE',  ( 0.000000000000000000, -0.000000000000000000, -1.000000000000000000 ) ) ;
#54268 = CARTESIAN_POINT ( 'NONE',  ( -14.59503576111680800, 1.095915999411503750, 4.349113516364012000 ) ) ;
#54269 = PLANE ( 'NONE',  #5245 ) ;
#54270 = CARTESIAN_POINT ( 'NONE',  ( -68.17821258402990736, -9.646719645199189230, 5.608481661906881577 ) ) ;
#54271 = ORIENTED_EDGE ( 'NONE', *, *, #5060, .F. ) ;
#54272 = LINE ( 'NONE', #15366, #3248 ) ;
#54273 = CARTESIAN_POINT ( 'NONE',  ( -67.02334604683971975, -0.6009592863103402349, 0.3393403235780959037 ) ) ;
#54274 = ORIENTED_EDGE ( 'NONE', *, *, #4977, .F. ) ;
#54275 = FACE_OUTER_BOUND ( 'NONE', #22551, .T. ) ;
#54276 = CARTESIAN_POINT ( 'NONE',  ( -9.908141408373387193, -0.1191753592594197858, 10.77908512878318703 ) ) ;
#54277 = LINE ( 'NONE', #44932, #34950 ) ;
#54278 = LINE ( 'NONE', #32689, #17863 ) ;
#54279 = DIRECTION ( 'NONE',  ( 0.000000000000000000, 0.000000000000000000, 1.000000000000000000 ) ) ;
#54280 = ORIENTED_EDGE ( 'NONE', *, *, #51883, .F. ) ;
#54281 = ORIENTED_EDGE ( 'NONE', *, *, #53683, .T. ) ;
#54282 = DIRECTION ( 'NONE',  ( 0.000000000000000000, -1.000000000000000000, 0.000000000000000000 ) ) ;
#54283 = EDGE_CURVE ( 'NONE', #53425, #32666, #4135, .T. ) ;
#54284 = FACE_OUTER_BOUND ( 'NONE', #24996, .T. ) ;
#54285 = EDGE_LOOP ( 'NONE', ( #55926, #24865, #4951, #11067 ) ) ;
#54286 = CARTESIAN_POINT ( 'NONE',  ( -19.07558811344151906, 0.000000000000000000, 7.457287032919146519 ) ) ;
#54287 = EDGE_CURVE ( 'NONE', #36870, #34792, #16920, .T. ) ;
#54288 = EDGE_LOOP ( 'NONE', ( #6404, #55649, #30603, #24543 ) ) ;
#54289 = CARTESIAN_POINT ( 'NONE',  ( -17.46532115785441519, 0.000000000000000000, 13.67492996699914265 ) ) ;
#54290 = ORIENTED_EDGE ( 'NONE', *, *, #21168, .F. ) ;
#54291 = VERTEX_POINT ( 'NONE', #47267 ) ;
#54292 = LINE ( 'NONE', #7166, #29301 ) ;
#54293 = FACE_OUTER_BOUND ( 'NONE', #40900, .T. ) ;
#54294 = CARTESIAN_POINT ( 'NONE',  ( -61.52150108290046404, 8.525944197083212828, -5.000000000000000000 ) ) ;
#54295 = EDGE_CURVE ( 'NONE', #6407, #49583, #8113, .T. ) ;
#54296 = ADVANCED_FACE ( 'NONE', ( #42180 ), #56096, .F. ) ;
#54297 = EDGE_CURVE ( 'NONE', #9050, #35406, #7844, .T. ) ;
#54298 = EDGE_LOOP ( 'NONE', ( #55432, #29594, #18711, #21342 ) ) ;
#54299 = VECTOR ( 'NONE', #1177, 1000.000000000000227 ) ;
#54300 = LINE ( 'NONE', #32710, #53877 ) ;
#54301 = ORIENTED_EDGE ( 'NONE', *, *, #44059, .T. ) ;
#54302 = ADVANCED_FACE ( 'NONE', ( #33943 ), #38782, .F. ) ;
#54303 = ORIENTED_EDGE ( 'NONE', *, *, #23792, .T. ) ;
#54304 = VERTEX_POINT ( 'NONE', #16614 ) ;
#54305 = LINE ( 'NONE', #40958, #50382 ) ;
#54306 = VERTEX_POINT ( 'NONE', #25418 ) ;
#54307 = DIRECTION ( 'NONE',  ( 0.000000000000000000, -1.000000000000000000, 0.000000000000000000 ) ) ;
#54308 = ORIENTED_EDGE ( 'NONE', *, *, #20159, .T. ) ;
#54309 = DIRECTION ( 'NONE',  ( -0.5449076811759708816, 0.6444004775717707689, 0.5364919789714475140 ) ) ;
#54310 = DIRECTION ( 'NONE',  ( -0.5364919789714478471, 0.6444004775717705469, -0.5449076811759709926 ) ) ;
#54311 = ORIENTED_EDGE ( 'NONE', *, *, #54776, .T. ) ;
#54312 = CARTESIAN_POINT ( 'NONE',  ( 2.072287782118878319, 0.000000000000000000, -2.950529333540147015 ) ) ;
#54313 = VERTEX_POINT ( 'NONE', #42727 ) ;
#54314 = EDGE_CURVE ( 'NONE', #14066, #24768, #3825, .T. ) ;
#54315 = EDGE_CURVE ( 'NONE', #22478, #34831, #38478, .T. ) ;
#54316 = DIRECTION ( 'NONE',  ( 0.007781995580012663651, 0.000000000000000000, -0.9999697198139515519 ) ) ;
#54317 = LINE ( 'NONE', #33322, #10283 ) ;
#54318 = DIRECTION ( 'NONE',  ( -0.9999697198139514409, -0.000000000000000000, -0.007781995580013368816 ) ) ;
#54319 = LINE ( 'NONE', #54052, #45662 ) ;
#54320 = EDGE_CURVE ( 'NONE', #6114, #50554, #27369, .T. ) ;
#54321 = DIRECTION ( 'NONE',  ( -0.6427681459581293666, -0.7660444431189770143, -0.005002170337467561935 ) ) ;
#54322 = CARTESIAN_POINT ( 'NONE',  ( -18.19747506107908563, 0.000000000000000000, 14.03856424583689311 ) ) ;
#54323 = DIRECTION ( 'NONE',  ( -0.5449076811759708816, 0.6444004775717707689, 0.5364919789714475140 ) ) ;
#54324 = EDGE_LOOP ( 'NONE', ( #30979, #2899, #42588, #44125, #12963, #32930, #24291, #6391 ) ) ;
#54326 = EDGE_LOOP ( 'NONE', ( #11398, #7639, #24301, #34110 ) ) ;
#54325 = EDGE_CURVE ( 'NONE', #32862, #8418, #48392, .T. ) ;
#54327 = CARTESIAN_POINT ( 'NONE',  ( -56.75000000000000711, 4.550000000000001599, 2.449489742783185875 ) ) ;
#54328 = CARTESIAN_POINT ( 'NONE',  ( -14.20280369269832832, 0.000000000000000000, 12.40765738797303719 ) ) ;
#54329 = LINE ( 'NONE', #6932, #42097 ) ;
#54330 = EDGE_CURVE ( 'NONE', #23038, #52596, #26530, .T. ) ;
#54331 = CARTESIAN_POINT ( 'NONE',  ( -8.276713462897552276, 0.000000000000000000, 6.433330163025533288 ) ) ;
#54332 = DIRECTION ( 'NONE',  ( 0.000000000000000000, 1.000000000000000000, 0.000000000000000000 ) ) ;
#54333 = ORIENTED_EDGE ( 'NONE', *, *, #40083, .F. ) ;
#54334 = CARTESIAN_POINT ( 'NONE',  ( -21.47263955680318404, 0.000000000000000000, 5.022634149262071190 ) ) ;
#54335 = CARTESIAN_POINT ( 'NONE',  ( -12.33850799832341849, 0.000000000000000000, 11.68350162852954632 ) ) ;
#54336 = ORIENTED_EDGE ( 'NONE', *, *, #21970, .F. ) ;
#54337 = LINE ( 'NONE', #23419, #18433 ) ;
#54338 = CARTESIAN_POINT ( 'NONE',  ( -14.94760462649100496, 0.000000000000000000, 2.488088991209854051 ) ) ;
#54339 = ORIENTED_EDGE ( 'NONE', *, *, #44107, .F. ) ;
#54340 = MECHANICAL_DESIGN_GEOMETRIC_PRESENTATION_REPRESENTATION (  '', ( #10817 ), #25325 ) ;
#54341 = CARTESIAN_POINT ( 'NONE',  ( -71.02048890987401819, -0.9999999999999995559, 8.554889286408840832 ) ) ;
#54342 = CARTESIAN_POINT ( 'NONE',  ( -63.56784591066751489, 8.775889882925216767, 3.000000000000000000 ) ) ;
#54343 = LINE ( 'NONE', #45823, #37698 ) ;
#54344 = FACE_OUTER_BOUND ( 'NONE', #37191, .T. ) ;
#54345 = CARTESIAN_POINT ( 'NONE',  ( -68.02073773998908734, 2.000000000000048850, 8.237893588744196194 ) ) ;
#54346 = ORIENTED_EDGE ( 'NONE', *, *, #11911, .F. ) ;
#54347 = ORIENTED_EDGE ( 'NONE', *, *, #14530, .F. ) ;
#54348 = CARTESIAN_POINT ( 'NONE',  ( -10.87762927220137144, 0.000000000000000000, 3.089100606534142202 ) ) ;
#54349 = FACE_OUTER_BOUND ( 'NONE', #38838, .T. ) ;
#54350 = LINE ( 'NONE', #29357, #27893 ) ;
#54351 = LINE ( 'NONE', #6660, #8697 ) ;
#54352 = CARTESIAN_POINT ( 'NONE',  ( -22.76109218059357175, -4.889348428825661230, 13.54736664680453551 ) ) ;
#54353 = LINE ( 'NONE', #23158, #44872 ) ;
#54354 = ORIENTED_EDGE ( 'NONE', *, *, #41777, .T. ) ;
#54355 = CARTESIAN_POINT ( 'NONE',  ( -19.59569683186026268, 0.000000000000000000, 14.58168106541950948 ) ) ;
#54356 = CARTESIAN_POINT ( 'NONE',  ( -14.20280369269832832, 0.000000000000000000, 12.40765738797303719 ) ) ;
#54357 = DIRECTION ( 'NONE',  ( 0.007781995580012663651, 0.000000000000000000, -0.9999697198139515519 ) ) ;
#54358 = ORIENTED_EDGE ( 'NONE', *, *, #34591, .F. ) ;
#54359 = CARTESIAN_POINT ( 'NONE',  ( -61.70068505767309830, 8.059153983834628221, 3.000000000000000000 ) ) ;
#54360 = DIRECTION ( 'NONE',  ( -0.6427681459581293666, -0.7660444431189770143, -0.005002170337467561935 ) ) ;
#54361 = DIRECTION ( 'NONE',  ( -0.6427681459581293666, -0.7660444431189770143, -0.005002170337467561935 ) ) ;
#54362 = EDGE_CURVE ( 'NONE', #14416, #33688, #43854, .T. ) ;
#54363 = VERTEX_POINT ( 'NONE', #43572 ) ;
#54364 = CARTESIAN_POINT ( 'NONE',  ( -18.78795273252095654, 0.000000000000000000, 4.504868919509038783 ) ) ;
#54365 = ORIENTED_EDGE ( 'NONE', *, *, #7102, .F. ) ;
#54366 = ADVANCED_FACE ( 'NONE', ( #40153 ), #31916, .F. ) ;
#54367 = EDGE_CURVE ( 'NONE', #45853, #38452, #52646, .T. ) ;
#54368 = ORIENTED_EDGE ( 'NONE', *, *, #41910, .F. ) ;
#54369 = ORIENTED_EDGE ( 'NONE', *, *, #54470, .T. ) ;
#54370 = ORIENTED_EDGE ( 'NONE', *, *, #12795, .T. ) ;
#54371 = VERTEX_POINT ( 'NONE', #14344 ) ;
#54372 = CARTESIAN_POINT ( 'NONE',  ( -23.95239534612751697, 18.82935394505787130, 4.517658012124546651 ) ) ;
#54373 = VERTEX_POINT ( 'NONE', #53250 ) ;
#54374 = ORIENTED_EDGE ( 'NONE', *, *, #19125, .T. ) ;
#54375 = PLANE ( 'NONE',  #46757 ) ;
#54376 = VERTEX_POINT ( 'NONE', #13752 ) ;
#54377 = ORIENTED_EDGE ( 'NONE', *, *, #24391, .T. ) ;
#54378 = EDGE_LOOP ( 'NONE', ( #15998, #39486, #15437 ) ) ;
#54379 = CARTESIAN_POINT ( 'NONE',  ( -15.89073401941919883, -0.1191753592594213818, 3.319416507920406989 ) ) ;
#54380 = LINE ( 'NONE', #15758, #3082 ) ;
#54381 = LINE ( 'NONE', #28551, #2384 ) ;
#54382 = PLANE ( 'NONE',  #29560 ) ;
#54383 = ORIENTED_EDGE ( 'NONE', *, *, #21987, .T. ) ;
#54384 = CARTESIAN_POINT ( 'NONE',  ( -11.29627228906843150, -0.03739765774599676518, 1.207800969688126891 ) ) ;
#54385 = EDGE_LOOP ( 'NONE', ( #32971, #53412, #53795 ) ) ;
#54386 = ORIENTED_EDGE ( 'NONE', *, *, #28161, .T. ) ;
#54387 = LINE ( 'NONE', #32807, #14085 ) ;
#54388 = DIRECTION ( 'NONE',  ( 0.005961354470445682716, -0.6427876096865404731, -0.7660212471507180654 ) ) ;
#54389 = EDGE_CURVE ( 'NONE', #50804, #30507, #22296, .T. ) ;
#54390 = CARTESIAN_POINT ( 'NONE',  ( -14.56888064431065821, -0.1191753592594197858, 12.58947452739191064 ) ) ;
#54391 = DIRECTION ( 'NONE',  ( 0.5449076811759707706, 0.6444004775717708799, -0.5364919789714476250 ) ) ;
#54392 = ADVANCED_FACE ( 'NONE', ( #31656 ), #4677, .F. ) ;
#54393 = DIRECTION ( 'NONE',  ( -0.7660212471507179544, -0.6427876096865405842, -0.005961354470445141482 ) ) ;
#54394 = CARTESIAN_POINT ( 'NONE',  ( -11.70248683415050550, 9.283552190907606416, 1.327269728845983821 ) ) ;
#54395 = EDGE_LOOP ( 'NONE', ( #2195, #22479, #50809, #10132 ) ) ;
#54396 = CARTESIAN_POINT ( 'NONE',  ( -18.67619601524082285, 0.000000000000000000, 3.936400510096834893 ) ) ;
#54397 = ADVANCED_FACE ( 'NONE', ( #4966 ), #35092, .F. ) ;
#54398 = EDGE_LOOP ( 'NONE', ( #28062, #31015, #48439, #1094 ) ) ;
#54399 = PLANE ( 'NONE',  #37395 ) ;
#54400 = CARTESIAN_POINT ( 'NONE',  ( 2.072287782118878319, 0.000000000000000000, -2.950529333540147015 ) ) ;
#54401 = CARTESIAN_POINT ( 'NONE',  ( -16.99924723426068951, 0.000000000000000000, 13.49389102713827171 ) ) ;
#54402 = EDGE_CURVE ( 'NONE', #15599, #29943, #23130, .T. ) ;
#54403 = CARTESIAN_POINT ( 'NONE',  ( -10.28686539055373395, 0.000000000000000000, 0.6776995926011265547 ) ) ;
#54404 = DIRECTION ( 'NONE',  ( -0.3620778797217457656, 0.000000000000000000, -0.9321478471874539151 ) ) ;
#54405 = AXIS2_PLACEMENT_3D ( 'NONE', #4225, #21541, #38854 ) ;
#54406 = ORIENTED_EDGE ( 'NONE', *, *, #25614, .T. ) ;
#54407 = CARTESIAN_POINT ( 'NONE',  ( -11.74614849678306427, -0.1159828484229813300, 7.780976552696367676 ) ) ;
#54408 = DIRECTION ( 'NONE',  ( -0.6427681459581293666, -0.7660444431189770143, -0.005002170337467561935 ) ) ;
#54409 = CARTESIAN_POINT ( 'NONE',  ( -17.77025923324963230, 0.4483081953215036219, 4.519643408181552857 ) ) ;
#54410 = LINE ( 'NONE', #15509, #44571 ) ;
#54411 = LINE ( 'NONE', #23759, #28490 ) ;
#54412 = FACE_OUTER_BOUND ( 'NONE', #22, .T. ) ;
#54413 = DIRECTION ( 'NONE',  ( -0.7660212471507179544, -0.6427876096865405842, -0.005961354470445141482 ) ) ;
#54414 = CARTESIAN_POINT ( 'NONE',  ( -25.20123094555300369, 0.000000000000000000, 6.470945668149052032 ) ) ;
#54415 = CARTESIAN_POINT ( 'NONE',  ( -18.29747203306047609, -0.1191753592594177458, 14.03778604627889059 ) ) ;
#54416 = EDGE_CURVE ( 'NONE', #50902, #4591, #961, .T. ) ;
#54417 = ORIENTED_EDGE ( 'NONE', *, *, #6384, .T. ) ;
#54418 = EDGE_CURVE ( 'NONE', #428, #11634, #52937, .T. ) ;
#54419 = ORIENTED_EDGE ( 'NONE', *, *, #18748, .T. ) ;
#54420 = EDGE_CURVE ( 'NONE', #54876, #9595, #21994, .T. ) ;
#54421 = ADVANCED_FACE ( 'NONE', ( #48961 ), #18879, .F. ) ;
#54422 = VERTEX_POINT ( 'NONE', #39324 ) ;
#54423 = VERTEX_POINT ( 'NONE', #14597 ) ;
#54424 = EDGE_LOOP ( 'NONE', ( #39916, #15213, #9502, #9818 ) ) ;
#54425 = ORIENTED_EDGE ( 'NONE', *, *, #47101, .T. ) ;
#54426 = CARTESIAN_POINT ( 'NONE',  ( -22.02718324817240969, 19.65220053346460816, -4.657437592157546824 ) ) ;
#54427 = CARTESIAN_POINT ( 'NONE',  ( -9.167413235801063820, -10.93230953041516429, 6.779308203112875297 ) ) ;
#54428 = LINE ( 'NONE', #28611, #34006 ) ;
#54429 = ORIENTED_EDGE ( 'NONE', *, *, #7430, .F. ) ;
#54430 = DIRECTION ( 'NONE',  ( 0.9999697198139515519, 0.000000000000000000, 0.007781995580013368816 ) ) ;
#54431 = ORIENTED_EDGE ( 'NONE', *, *, #23120, .F. ) ;
#54432 = ORIENTED_EDGE ( 'NONE', *, *, #45423, .T. ) ;
#54433 = ADVANCED_FACE ( 'NONE', ( #18026 ), #26262, .F. ) ;
#54434 = AXIS2_PLACEMENT_3D ( 'NONE', #54675, #15782, #16083 ) ;
#54435 = CARTESIAN_POINT ( 'NONE',  ( -65.57510285225123425, -9.214371548364283626, 3.765673540395807706 ) ) ;
#54436 = PLANE ( 'NONE',  #17350 ) ;
#54437 = CARTESIAN_POINT ( 'NONE',  ( -18.19747506107908563, 0.000000000000000000, 14.03856424583689311 ) ) ;
#54438 = EDGE_LOOP ( 'NONE', ( #52028, #49601, #32848, #11169 ) ) ;
#54439 = DIRECTION ( 'NONE',  ( 0.007781995580012663651, 0.000000000000000000, -0.9999697198139515519 ) ) ;
#54440 = ORIENTED_EDGE ( 'NONE', *, *, #9721, .F. ) ;
#54441 = CARTESIAN_POINT ( 'NONE',  ( -17.66287670277056066, 0.000000000000000000, 5.052282604713799863 ) ) ;
#54442 = PLANE ( 'NONE',  #20279 ) ;
#54443 = FACE_OUTER_BOUND ( 'NONE', #45659, .T. ) ;
#54444 = CARTESIAN_POINT ( 'NONE',  ( -18.22472998780914466, -0.6798977022406571535, 3.938732862525397671 ) ) ;
#54445 = CARTESIAN_POINT ( 'NONE',  ( -9.838958146463953724, -0.1191753592594204242, 1.889184547873473452 ) ) ;
#54446 = FACE_OUTER_BOUND ( 'NONE', #45840, .T. ) ;
#54447 = DIRECTION ( 'NONE',  ( -0.3620778797217457101, 0.000000000000000000, -0.9321478471874540261 ) ) ;
#54448 = DIRECTION ( 'NONE',  ( 0.007781995580012663651, -3.146120232559066537E-19, -0.9999697198139514409 ) ) ;
#54449 = ORIENTED_EDGE ( 'NONE', *, *, #9774, .F. ) ;
#54450 = CARTESIAN_POINT ( 'NONE',  ( -15.93384482199843788, -0.1191753592594196193, 8.859062056786873640 ) ) ;
#54451 = EDGE_LOOP ( 'NONE', ( #22193, #39623, #8214, #17733 ) ) ;
#54452 = AXIS2_PLACEMENT_3D ( 'NONE', #16181, #33504, #46258 ) ;
#54453 = DIRECTION ( 'NONE',  ( 0.3535533905932752297, -0.6123724356957952475, 0.7071067811865462405 ) ) ;
#54454 = DIRECTION ( 'NONE',  ( -0.5449076811759708816, 0.6444004775717707689, 0.5364919789714475140 ) ) ;
#54455 = DIRECTION ( 'NONE',  ( -0.005961354470445682716, -0.6427876096865404731, 0.7660212471507180654 ) ) ;
#54456 = ADVANCED_FACE ( 'NONE', ( #410 ), #30808, .F. ) ;
#54457 = DIRECTION ( 'NONE',  ( -0.005002170337468016433, -0.7660444431189770143, 0.6427681459581293666 ) ) ;
#54458 = CARTESIAN_POINT ( 'NONE',  ( -22.40478740399063895, 0.000000000000000000, 5.384712028983816623 ) ) ;
#54459 = FACE_OUTER_BOUND ( 'NONE', #39590, .T. ) ;
#54460 = ORIENTED_EDGE ( 'NONE', *, *, #38642, .F. ) ;
#54461 = DIRECTION ( 'NONE',  ( 0.5449076811759707706, 0.6444004775717708799, -0.5364919789714476250 ) ) ;
#54462 = DIRECTION ( 'NONE',  ( 0.000000000000000000, -1.000000000000000000, 0.000000000000000000 ) ) ;
#54463 = DIRECTION ( 'NONE',  ( 0.007781995580012662783, 0.000000000000000000, -0.9999697198139514409 ) ) ;
#54464 = DIRECTION ( 'NONE',  ( 0.000000000000000000, -0.000000000000000000, -1.000000000000000000 ) ) ;
#54465 = CARTESIAN_POINT ( 'NONE',  ( -26.13493519185646008, 0.000000000000000000, 7.033017491833586377 ) ) ;
#54466 = EDGE_CURVE ( 'NONE', #50886, #34260, #10652, .T. ) ;
#54467 = VECTOR ( 'NONE', #30737, 1000.000000000000114 ) ;
#54468 = CARTESIAN_POINT ( 'NONE',  ( -15.88405162580815855, 3.200641362704010007, 2.749719590951118953 ) ) ;
#54469 = DIRECTION ( 'NONE',  ( -0.005961354470445682716, -0.6427876096865404731, 0.7660212471507180654 ) ) ;
#54470 = EDGE_CURVE ( 'NONE', #51326, #33913, #50353, .T. ) ;
#54471 = CARTESIAN_POINT ( 'NONE',  ( -13.01363368085442040, 0.000000000000000000, 4.719132019136131007 ) ) ;
#54472 = ADVANCED_FACE ( 'NONE', ( #11465 ), #27668, .F. ) ;
#54473 = DIRECTION ( 'NONE',  ( 0.007781995580012662783, 0.000000000000000000, -0.9999697198139514409 ) ) ;
#54474 = ORIENTED_EDGE ( 'NONE', *, *, #49130, .T. ) ;
#54475 = VECTOR ( 'NONE', #38014, 999.9999999999998863 ) ;
#54476 = DIRECTION ( 'NONE',  ( 0.007781995580012663651, -3.146120232559066537E-19, -0.9999697198139514409 ) ) ;
#54477 = ORIENTED_EDGE ( 'NONE', *, *, #45037, .T. ) ;
#54478 = LINE ( 'NONE', #20418, #52101 ) ;
#54479 = CARTESIAN_POINT ( 'NONE',  ( -11.40636015113596180, 0.000000000000000000, 11.32142374880780089 ) ) ;
#54480 = ADVANCED_FACE ( 'NONE', ( #54066 ), #1799, .F. ) ;
#54481 = ORIENTED_EDGE ( 'NONE', *, *, #37837, .T. ) ;
#54482 = EDGE_CURVE ( 'NONE', #18846, #21097, #45518, .T. ) ;
#54483 = VERTEX_POINT ( 'NONE', #40731 ) ;
#54484 = CARTESIAN_POINT ( 'NONE',  ( -14.01701317841955508, 0.000000000000000000, 2.326005055450897085 ) ) ;
#54485 = EDGE_CURVE ( 'NONE', #18056, #17655, #49533, .T. ) ;
#54486 = VERTEX_POINT ( 'NONE', #37281 ) ;
#54487 = ORIENTED_EDGE ( 'NONE', *, *, #12708, .T. ) ;
#54488 = ORIENTED_EDGE ( 'NONE', *, *, #48807, .T. ) ;
#54489 = DIRECTION ( 'NONE',  ( -0.7660212471507179544, -0.6427876096865405842, -0.005961354470445141482 ) ) ;
#54490 = CARTESIAN_POINT ( 'NONE',  ( -65.30888085680906840, -9.183842752983270685, 2.627585852360244445 ) ) ;
#54491 = DIRECTION ( 'NONE',  ( 0.3313982828793700097, 0.4028455766673915694, 0.8531650599175529814 ) ) ;
#54492 = EDGE_CURVE ( 'NONE', #38597, #10075, #24497, .T. ) ;
#54493 = AXIS2_PLACEMENT_3D ( 'NONE', #20956, #55603, #37438 ) ;
#54494 = VECTOR ( 'NONE', #27502, 1000.000000000000227 ) ;
#54495 = VERTEX_POINT ( 'NONE', #14881 ) ;
#54496 = ORIENTED_EDGE ( 'NONE', *, *, #45925, .F. ) ;
#54497 = EDGE_CURVE ( 'NONE', #48860, #3819, #23949, .T. ) ;
#54498 = LINE ( 'NONE', #11901, #52964 ) ;
#54499 = DIRECTION ( 'NONE',  ( -0.2588190451025176864, -0.9659258262890692004, 0.000000000000000000 ) ) ;
#54500 = VERTEX_POINT ( 'NONE', #10892 ) ;
#54501 = DIRECTION ( 'NONE',  ( 0.005002170337468016433, -0.7660444431189770143, -0.6427681459581293666 ) ) ;
#54502 = EDGE_LOOP ( 'NONE', ( #49412, #44438, #17933, #6042 ) ) ;
#54503 = DIRECTION ( 'NONE',  ( 0.005961354470445682716, -0.6427876096865404731, -0.7660212471507180654 ) ) ;
#54504 = DIRECTION ( 'NONE',  ( 0.005961354470445682716, -0.6427876096865404731, -0.7660212471507180654 ) ) ;
#54505 = ORIENTED_EDGE ( 'NONE', *, *, #30032, .F. ) ;
#54506 = CARTESIAN_POINT ( 'NONE',  ( 5.283025405476269754, -1.075926357871029415, -2.393287282172987140 ) ) ;
#54507 = VECTOR ( 'NONE', #7964, 1000.000000000000000 ) ;
#54508 = DIRECTION ( 'NONE',  ( 0.6427681459581294776, -0.7660444431189769032, 0.005002170337467562802 ) ) ;
#54509 = ORIENTED_EDGE ( 'NONE', *, *, #1849, .T. ) ;
#54510 = PLANE ( 'NONE',  #14951 ) ;
#54511 = LINE ( 'NONE', #3121, #4906 ) ;
#54512 = DIRECTION ( 'NONE',  ( -0.005961354470445682716, -0.6427876096865404731, 0.7660212471507180654 ) ) ;
#54513 = EDGE_LOOP ( 'NONE', ( #48885, #53538, #34120, #26510 ) ) ;
#54514 = PLANE ( 'NONE',  #45550 ) ;
#54515 = CARTESIAN_POINT ( 'NONE',  ( -17.74404816805336793, 0.000000000000000000, 3.574322630375089460 ) ) ;
#54516 = DIRECTION ( 'NONE',  ( 0.007781995580012662783, 0.000000000000000000, -0.9999697198139514409 ) ) ;
#54517 = EDGE_CURVE ( 'NONE', #3951, #20306, #2072, .T. ) ;
#54518 = CARTESIAN_POINT ( 'NONE',  ( -6.264213140240936006, -6.015707657378981388, -0.7851404584205251558 ) ) ;
#54519 = FACE_OUTER_BOUND ( 'NONE', #46603, .T. ) ;
#54520 = CARTESIAN_POINT ( 'NONE',  ( -25.20123094555300369, 0.000000000000000000, 6.470945668149052032 ) ) ;
#54521 = DIRECTION ( 'NONE',  ( 0.000000000000000000, -0.000000000000000000, -1.000000000000000000 ) ) ;
#54522 = EDGE_LOOP ( 'NONE', ( #47116, #13794, #7331, #9551 ) ) ;
#54523 = CARTESIAN_POINT ( 'NONE',  ( -27.06708303904391144, 0.000000000000000000, 7.395095371555332697 ) ) ;
#54524 = CARTESIAN_POINT ( 'NONE',  ( -66.51057813521288153, 4.515102018714843381E-12, 1.428098984229650759 ) ) ;
#54525 = ORIENTED_EDGE ( 'NONE', *, *, #21878, .T. ) ;
#54526 = DIRECTION ( 'NONE',  ( -0.5364919789714478471, 0.6444004775717705469, -0.5449076811759709926 ) ) ;
#54527 = CARTESIAN_POINT ( 'NONE',  ( -28.92982233430281980, 0.000000000000000000, 7.919257187036034651 ) ) ;
#54528 = VECTOR ( 'NONE', #18903, 999.9999999999998863 ) ;
#54529 = VECTOR ( 'NONE', #556, 1000.000000000000227 ) ;
#54530 = CARTESIAN_POINT ( 'NONE',  ( -13.48401868470607035, 0.000000000000000000, 5.454135513883649367 ) ) ;
#54531 = DIRECTION ( 'NONE',  ( 0.005002170337468016433, -0.7660444431189770143, -0.6427681459581293666 ) ) ;
#54532 = EDGE_CURVE ( 'NONE', #18137, #40042, #20236, .T. ) ;
#54533 = CARTESIAN_POINT ( 'NONE',  ( -14.10280672071693431, -0.1191753592594197858, 12.40843558753103792 ) ) ;
#54534 = VERTEX_POINT ( 'NONE', #19706 ) ;
#54535 = VECTOR ( 'NONE', #439, 1000.000000000000227 ) ;
#54536 = EDGE_LOOP ( 'NONE', ( #6181, #757 ) ) ;
#54537 = FACE_OUTER_BOUND ( 'NONE', #51752, .T. ) ;
#54538 = DIRECTION ( 'NONE',  ( 0.9999697198139515519, 0.000000000000000000, 0.007781995580013368816 ) ) ;
#54539 = PLANE ( 'NONE',  #37435 ) ;
#54540 = VERTEX_POINT ( 'NONE', #23666 ) ;
#54541 = EDGE_CURVE ( 'NONE', #3706, #21619, #53763, .T. ) ;
#54542 = DIRECTION ( 'NONE',  ( 0.005961354470445682716, -0.6427876096865404731, -0.7660212471507180654 ) ) ;
#54543 = ORIENTED_EDGE ( 'NONE', *, *, #10531, .T. ) ;
#54544 = DIRECTION ( 'NONE',  ( 0.9999697198139515519, 0.000000000000000000, 0.007781995580013368816 ) ) ;
#54545 = AXIS2_PLACEMENT_3D ( 'NONE', #53486, #31901, #19691 ) ;
#54546 = EDGE_CURVE ( 'NONE', #21903, #5703, #24246, .T. ) ;
#54547 = ORIENTED_EDGE ( 'NONE', *, *, #10054, .T. ) ;
#54548 = ORIENTED_EDGE ( 'NONE', *, *, #32410, .F. ) ;
#54549 = DIRECTION ( 'NONE',  ( 0.007781995580012663651, 0.000000000000000000, -0.9999697198139515519 ) ) ;
#54550 = DIRECTION ( 'NONE',  ( 0.005961354470445682716, -0.6427876096865404731, -0.7660212471507180654 ) ) ;
#54551 = DIRECTION ( 'NONE',  ( -0.9999697198139514409, -0.000000000000000000, -0.007781995580013368816 ) ) ;
#54552 = ORIENTED_EDGE ( 'NONE', *, *, #24359, .F. ) ;
#54553 = EDGE_CURVE ( 'NONE', #34361, #51735, #28206, .T. ) ;
#54554 = PLANE ( 'NONE',  #17477 ) ;
#54555 = VERTEX_POINT ( 'NONE', #2637 ) ;
#54556 = ORIENTED_EDGE ( 'NONE', *, *, #39039, .T. ) ;
#54557 = ADVANCED_FACE ( 'NONE', ( #2906 ), #46091, .F. ) ;
#54558 = EDGE_LOOP ( 'NONE', ( #28904, #45106, #40426, #3741 ) ) ;
#54559 = FACE_OUTER_BOUND ( 'NONE', #52780, .T. ) ;
#54560 = ORIENTED_EDGE ( 'NONE', *, *, #8334, .F. ) ;
#54561 = FACE_OUTER_BOUND ( 'NONE', #15716, .T. ) ;
#54562 = EDGE_LOOP ( 'NONE', ( #24877, #21633, #20782, #35739 ) ) ;
#54563 = FACE_OUTER_BOUND ( 'NONE', #9684, .T. ) ;
#54564 = DIRECTION ( 'NONE',  ( -0.7660212471507179544, -0.6427876096865405842, -0.005961354470445141482 ) ) ;
#54565 = VECTOR ( 'NONE', #13996, 1000.000000000000227 ) ;
#54566 = AXIS2_PLACEMENT_3D ( 'NONE', #22210, #22501, #39237 ) ;
#54567 = ORIENTED_EDGE ( 'NONE', *, *, #40485, .F. ) ;
#54568 = CARTESIAN_POINT ( 'NONE',  ( 0.4518049228021103203, -3.655895688227122076, 5.998622290806040702 ) ) ;
#54569 = ORIENTED_EDGE ( 'NONE', *, *, #42886, .T. ) ;
#54570 = LINE ( 'NONE', #33019, #31915 ) ;
#54571 = CARTESIAN_POINT ( 'NONE',  ( -22.40634380310664397, 0.000000000000000000, 5.584705972946605534 ) ) ;
#54572 = AXIS2_PLACEMENT_3D ( 'NONE', #55958, #13065, #21004 ) ;
#54573 = CARTESIAN_POINT ( 'NONE',  ( -8.875996589204540044, 0.000000000000000000, 10.41778544861944233 ) ) ;
#54574 = CARTESIAN_POINT ( 'NONE',  ( -19.88509817834021476, 3.524445264749009876, 4.293530908292650494 ) ) ;
#54575 = FACE_OUTER_BOUND ( 'NONE', #35253, .T. ) ;
#54576 = FACE_OUTER_BOUND ( 'NONE', #6820, .T. ) ;
#54577 = VERTEX_POINT ( 'NONE', #54331 ) ;
#54578 = ADVANCED_FACE ( 'NONE', ( #15423 ), #10347, .F. ) ;
#54579 = ORIENTED_EDGE ( 'NONE', *, *, #35191, .T. ) ;
#54580 = CARTESIAN_POINT ( 'NONE',  ( -10.89906530112762972, 0.000000000000000000, 5.843584288633468127 ) ) ;
#54581 = DIRECTION ( 'NONE',  ( -0.005961354470445682716, -0.6427876096865404731, 0.7660212471507180654 ) ) ;
#54582 = AXIS2_PLACEMENT_3D ( 'NONE', #20671, #24618, #8166 ) ;
#54583 = EDGE_CURVE ( 'NONE', #44507, #14930, #6111, .T. ) ;
#54584 = LINE ( 'NONE', #50636, #29502 ) ;
#54585 = CARTESIAN_POINT ( 'NONE',  ( -24.83619454210204580, 18.20872041849631984, -4.561852789702152577 ) ) ;
#54586 = DIRECTION ( 'NONE',  ( -0.005002170337468016433, -0.7660444431189770143, 0.6427681459581293666 ) ) ;
#54587 = FACE_OUTER_BOUND ( 'NONE', #7718, .T. ) ;
#54588 = ORIENTED_EDGE ( 'NONE', *, *, #45461, .T. ) ;
#54589 = ADVANCED_FACE ( 'NONE', ( #55440 ), #30174, .F. ) ;
#54590 = CARTESIAN_POINT ( 'NONE',  ( -9.121988873521557295, -2.596375463177813536, 3.509404230218840404 ) ) ;
#54591 = DIRECTION ( 'NONE',  ( 0.007781995580012663651, 0.000000000000000000, -0.9999697198139515519 ) ) ;
#54592 = ORIENTED_EDGE ( 'NONE', *, *, #41247, .F. ) ;
#54593 = CARTESIAN_POINT ( 'NONE',  ( -9.905246062020005127, 7.542634850262289525, 0.6291603783969644814 ) ) ;
#54594 = DIRECTION ( 'NONE',  ( 0.005002170337468016433, -0.7660444431189770143, -0.6427681459581293666 ) ) ;
#54595 = ORIENTED_EDGE ( 'NONE', *, *, #34476, .T. ) ;
#54596 = EDGE_CURVE ( 'NONE', #23008, #52604, #4058, .T. ) ;
#54597 = EDGE_CURVE ( 'NONE', #44414, #2010, #29903, .T. ) ;
#54598 = EDGE_CURVE ( 'NONE', #13325, #1875, #42951, .T. ) ;
#54599 = CARTESIAN_POINT ( 'NONE',  ( -68.92435787895500710, 2.000000000000635048, 6.355103916287438537 ) ) ;
#54600 = DIRECTION ( 'NONE',  ( 0.007781995580012663651, 0.000000000000000000, -0.9999697198139515519 ) ) ;
#54601 = DIRECTION ( 'NONE',  ( -0.005002170337468016433, -0.7660444431189770143, 0.6427681459581293666 ) ) ;
#54602 = AXIS2_PLACEMENT_3D ( 'NONE', #30567, #46502, #55314 ) ;
#54603 = DIRECTION ( 'NONE',  ( 0.005961354470445682716, -0.6427876096865404731, -0.7660212471507180654 ) ) ;
#54604 = PLANE ( 'NONE',  #28345 ) ;
#54605 = EDGE_LOOP ( 'NONE', ( #28642, #8918, #13085, #1078 ) ) ;
#54606 = ORIENTED_EDGE ( 'NONE', *, *, #746, .F. ) ;
#54607 = FACE_OUTER_BOUND ( 'NONE', #39897, .T. ) ;
#54608 = CARTESIAN_POINT ( 'NONE',  ( -10.74029228357944987, 0.000000000000000000, 11.14194120806293320 ) ) ;
#54609 = AXIS2_PLACEMENT_3D ( 'NONE', #39844, #44109, #18246 ) ;
#54610 = LINE ( 'NONE', #20569, #42391 ) ;
#54611 = VECTOR ( 'NONE', #520, 1000.000000000000227 ) ;
#54612 = CARTESIAN_POINT ( 'NONE',  ( -17.34579682753419050, -0.1191753592594159833, 9.956070129217877707 ) ) ;
#54613 = AXIS2_PLACEMENT_3D ( 'NONE', #5445, #22757, #19053 ) ;
#54614 = LINE ( 'NONE', #29069, #53688 ) ;
#54615 = ADVANCED_FACE ( 'NONE', ( #38126 ), #51743, .F. ) ;
#54616 = CARTESIAN_POINT ( 'NONE',  ( -11.87243407472968926, 0.000000000000000000, 11.50246268866867361 ) ) ;
#54617 = ORIENTED_EDGE ( 'NONE', *, *, #16421, .F. ) ;
#54618 = LINE ( 'NONE', #50387, #36514 ) ;
#54619 = EDGE_CURVE ( 'NONE', #25102, #46963, #29335, .T. ) ;
#54620 = LINE ( 'NONE', #3247, #7861 ) ;
#54621 = VECTOR ( 'NONE', #50160, 1000.000000000000227 ) ;
#54622 = CARTESIAN_POINT ( 'NONE',  ( -20.54762051412559742, -2.298917212465657833, 8.436240138526766685 ) ) ;
#54623 = VECTOR ( 'NONE', #40855, 999.9999999999998863 ) ;
#54624 = EDGE_LOOP ( 'NONE', ( #8220, #30302, #34977, #5603 ) ) ;
#54625 = B_SPLINE_CURVE_WITH_KNOTS ( 'NONE', 3,
 ( #22334, #27407, #8991, #31418 ),
 .UNSPECIFIED., .F., .F.,
 ( 4, 4 ),
 ( 0.2710609481134873544, 0.2986749355271498541 ),
 .UNSPECIFIED. ) ;
#54626 = EDGE_CURVE ( 'NONE', #46096, #50687, #37872, .T. ) ;
#54627 = DIRECTION ( 'NONE',  ( 0.000000000000000000, -1.000000000000000000, 0.000000000000000000 ) ) ;
#54628 = DIRECTION ( 'NONE',  ( -0.3620778797217456546, 0.000000000000000000, -0.9321478471874540261 ) ) ;
#54629 = LINE ( 'NONE', #37611, #50199 ) ;
#54630 = ORIENTED_EDGE ( 'NONE', *, *, #38784, .T. ) ;
#54631 = ADVANCED_FACE ( 'NONE', ( #16543 ), #51194, .F. ) ;
#54632 = CARTESIAN_POINT ( 'NONE',  ( -17.63855930251027360, 4.657758921906509642, 11.37691246524594568 ) ) ;
#54633 = AXIS2_PLACEMENT_3D ( 'NONE', #18657, #32282, #49602 ) ;
#54634 = ORIENTED_EDGE ( 'NONE', *, *, #10925, .T. ) ;
#54635 = EDGE_CURVE ( 'NONE', #52808, #29873, #12305, .T. ) ;
#54636 = VERTEX_POINT ( 'NONE', #4359 ) ;
#54637 = ORIENTED_EDGE ( 'NONE', *, *, #42598, .F. ) ;
#54638 = ORIENTED_EDGE ( 'NONE', *, *, #1674, .T. ) ;
#54639 = EDGE_LOOP ( 'NONE', ( #9222, #45725, #11232, #46367 ) ) ;
#54640 = DIRECTION ( 'NONE',  ( 0.005961354470445682716, -0.6427876096865404731, -0.7660212471507180654 ) ) ;
#54641 = ORIENTED_EDGE ( 'NONE', *, *, #8715, .F. ) ;
#54642 = AXIS2_PLACEMENT_3D ( 'NONE', #40280, #45117, #36300 ) ;
#54643 = ORIENTED_EDGE ( 'NONE', *, *, #7427, .F. ) ;
#54644 = DIRECTION ( 'NONE',  ( 0.005961354470445682716, -0.6427876096865404731, -0.7660212471507180654 ) ) ;
#54645 = ORIENTED_EDGE ( 'NONE', *, *, #11076, .F. ) ;
#54646 = VECTOR ( 'NONE', #9682, 1000.000000000000000 ) ;
#54647 = VERTEX_POINT ( 'NONE', #34178 ) ;
#54648 = DIRECTION ( 'NONE',  ( 0.5364919789714477361, 0.6444004775717706579, 0.5449076811759711036 ) ) ;
#54649 = LINE ( 'NONE', #24298, #7634 ) ;
#54650 = LINE ( 'NONE', #55230, #39577 ) ;
#54651 = PLANE ( 'NONE',  #24164 ) ;
#54652 = AXIS2_PLACEMENT_3D ( 'NONE', #34824, #150, #11346 ) ;
#54653 = ORIENTED_EDGE ( 'NONE', *, *, #555, .F. ) ;
#54654 = LINE ( 'NONE', #51256, #41903 ) ;
#54655 = ORIENTED_EDGE ( 'NONE', *, *, #4877, .F. ) ;
#54656 = VECTOR ( 'NONE', #43771, 999.9999999999998863 ) ;
#54657 = VECTOR ( 'NONE', #6780, 1000.000000000000227 ) ;
#54658 = ORIENTED_EDGE ( 'NONE', *, *, #39483, .T. ) ;
#54659 = LINE ( 'NONE', #25162, #34877 ) ;
#54660 = CARTESIAN_POINT ( 'NONE',  ( -10.85057559606751276, 1.095915999411505526, 0.8616983219704370534 ) ) ;
#54661 = UNCERTAINTY_MEASURE_WITH_UNIT (LENGTH_MEASURE( 1.000000000000000082E-05 ), #46273, 'distance_accuracy_value', 'NONE');
#54662 = LINE ( 'NONE', #54390, #9749 ) ;
#54663 = VECTOR ( 'NONE', #39591, 1000.000000000000114 ) ;
#54664 = VECTOR ( 'NONE', #1747, 1000.000000000000000 ) ;
#54665 = LINE ( 'NONE', #45072, #54820 ) ;
#54666 = DIRECTION ( 'NONE',  ( 0.6427681459581294776, -0.7660444431189769032, 0.005002170337467562802 ) ) ;
#54667 = DIRECTION ( 'NONE',  ( -0.5449076811759708816, 0.6444004775717707689, 0.5364919789714475140 ) ) ;
#54668 = ORIENTED_EDGE ( 'NONE', *, *, #41357, .F. ) ;
#54669 = CARTESIAN_POINT ( 'NONE',  ( -9.110551994824897193, 0.000000000000000000, 3.538847790438064411 ) ) ;
#54670 = ORIENTED_EDGE ( 'NONE', *, *, #10531, .F. ) ;
#54671 = ADVANCED_FACE ( 'NONE', ( #33873 ), #42104, .F. ) ;
#54672 = EDGE_CURVE ( 'NONE', #21642, #37323, #3210, .T. ) ;
#54673 = CARTESIAN_POINT ( 'NONE',  ( -18.42572312212858776, 0.1245042932765033361, 4.242830474368576965 ) ) ;
#54674 = PLANE ( 'NONE',  #50459 ) ;
#54675 = CARTESIAN_POINT ( 'NONE',  ( 2.072287782118878319, 0.000000000000000000, -2.950529333540147015 ) ) ;
#54676 = AXIS2_PLACEMENT_3D ( 'NONE', #20083, #7066, #11014 ) ;
#54677 = DIRECTION ( 'NONE',  ( 0.9999697198139515519, 0.000000000000000000, 0.007781995580013368816 ) ) ;
#54678 = EDGE_CURVE ( 'NONE', #9132, #11534, #55732, .T. ) ;
#54679 = VECTOR ( 'NONE', #30005, 1000.000000000000114 ) ;
#54680 = CARTESIAN_POINT ( 'NONE',  ( -20.62011252791016247, -4.565544526780660917, 12.18432007382632598 ) ) ;
#54681 = EDGE_LOOP ( 'NONE', ( #38763, #25129, #44891, #2419 ) ) ;
#54682 = EDGE_LOOP ( 'NONE', ( #48914, #41512, #8363, #30011 ) ) ;
#54683 = CARTESIAN_POINT ( 'NONE',  ( -17.04851670312061884, -5.375054281893165253, 3.332051601646770500 ) ) ;
#54684 = CARTESIAN_POINT ( 'NONE',  ( -20.41408287047329750, 20.87219960535384544, 4.314533580056656881 ) ) ;
#54685 = PLANE ( 'NONE',  #47833 ) ;
#54686 = AXIS2_PLACEMENT_3D ( 'NONE', #18016, #4955, #18865 ) ;
#54687 = CARTESIAN_POINT ( 'NONE',  ( -17.83139810946674686, -0.1191753592594197858, 13.85674710641801788 ) ) ;
#54688 = CARTESIAN_POINT ( 'NONE',  ( -20.18318107743349898, 0.000000000000000000, 4.663336943499984066 ) ) ;
#54689 = AXIS2_PLACEMENT_3D ( 'NONE', #4632, #42977, #4377 ) ;
#54690 = DIRECTION ( 'NONE',  ( 0.9999697198139515519, 0.000000000000000000, 0.007781995580013368816 ) ) ;
#54691 = DIRECTION ( 'NONE',  ( 0.005002170337468016433, -0.7660444431189770143, -0.6427681459581293666 ) ) ;
#54692 = EDGE_CURVE ( 'NONE', #49583, #55978, #8049, .T. ) ;
#54693 = LINE ( 'NONE', #50460, #4260 ) ;
#54694 = VECTOR ( 'NONE', #677, 999.9999999999998863 ) ;
#54695 = CARTESIAN_POINT ( 'NONE',  ( -19.54411535461957783, -0.03228989815065526348, 4.471889025059788914 ) ) ;
#54696 = VECTOR ( 'NONE', #23047, 1000.000000000000000 ) ;
#54697 = VECTOR ( 'NONE', #39886, 1000.000000000000227 ) ;
#54698 = ORIENTED_EDGE ( 'NONE', *, *, #45841, .T. ) ;
#54699 = ADVANCED_FACE ( 'NONE', ( #25359 ), #12585, .F. ) ;
#54700 = EDGE_CURVE ( 'NONE', #3988, #27645, #8307, .T. ) ;
#54701 = VECTOR ( 'NONE', #41712, 1000.000000000000114 ) ;
#54702 = EDGE_LOOP ( 'NONE', ( #32422, #44329, #9154, #54168 ) ) ;
#54703 = EDGE_LOOP ( 'NONE', ( #24897, #18007, #34971, #30785 ) ) ;
#54704 = AXIS2_PLACEMENT_3D ( 'NONE', #18105, #49042, #10144 ) ;
#54705 = ORIENTED_EDGE ( 'NONE', *, *, #34840, .F. ) ;
#54706 = EDGE_CURVE ( 'NONE', #53425, #37781, #44, .T. ) ;
#54707 = EDGE_LOOP ( 'NONE', ( #11885, #21557, #27350, #39977 ) ) ;
#54708 = CARTESIAN_POINT ( 'NONE',  ( -12.74767307358684576, 0.000000000000000000, 4.551875772493161776 ) ) ;
#54709 = DIRECTION ( 'NONE',  ( 0.9999697198139515519, 0.000000000000000000, 0.007781995580013368816 ) ) ;
#54710 = ADVANCED_FACE ( 'NONE', ( #46349 ), #7465, .F. ) ;
#54711 = DIRECTION ( 'NONE',  ( 0.5364919789714477361, 0.6444004775717706579, 0.5449076811759711036 ) ) ;
#54712 = ORIENTED_EDGE ( 'NONE', *, *, #45197, .F. ) ;
#54713 = DIRECTION ( 'NONE',  ( -0.9999697198139514409, -0.000000000000000000, -0.007781995580013368816 ) ) ;
#54714 = EDGE_CURVE ( 'NONE', #44660, #21187, #5451, .T. ) ;
#54715 = ORIENTED_EDGE ( 'NONE', *, *, #18160, .F. ) ;
#54716 = CARTESIAN_POINT ( 'NONE',  ( -26.13493519185646008, 0.000000000000000000, 7.033017491833586377 ) ) ;
#54717 = ORIENTED_EDGE ( 'NONE', *, *, #27917, .T. ) ;
#54718 = CARTESIAN_POINT ( 'NONE',  ( -66.08628404271949819, -9.272990844416433731, 5.190771789778323431 ) ) ;
#54719 = VECTOR ( 'NONE', #53476, 1000.000000000000227 ) ;
#54720 = FACE_OUTER_BOUND ( 'NONE', #48542, .T. ) ;
#54721 = DIRECTION ( 'NONE',  ( 0.5364919789714477361, 0.6444004775717706579, 0.5449076811759711036 ) ) ;
#54722 = ORIENTED_EDGE ( 'NONE', *, *, #29222, .F. ) ;
#54723 = PLANE ( 'NONE',  #21034 ) ;
#54724 = AXIS2_PLACEMENT_3D ( 'NONE', #32288, #48766, #14408 ) ;
#54725 = VERTEX_POINT ( 'NONE', #13968 ) ;
#54726 = CARTESIAN_POINT ( 'NONE',  ( -15.90130487007129823, -4.565544526780663581, 2.912263165649522367 ) ) ;
#54728 = VECTOR ( 'NONE', #40539, 1000.000000000000227 ) ;
#54727 = DIRECTION ( 'NONE',  ( 0.005002170337468016433, -0.7660444431189770143, -0.6427681459581293666 ) ) ;
#54729 = CARTESIAN_POINT ( 'NONE',  ( -18.60939481748442859, 0.000000000000000000, 7.260909000724367957 ) ) ;
#54730 = DIRECTION ( 'NONE',  ( 0.005002170337468016433, -0.7660444431189770143, -0.6427681459581293666 ) ) ;
#54731 = CARTESIAN_POINT ( 'NONE',  ( -10.39574805432858895, 0.000000000000000000, 0.8768582987555647579 ) ) ;
#54732 = PLANE ( 'NONE',  #1171 ) ;
#54733 = CARTESIAN_POINT ( 'NONE',  ( -18.60077265696858007, 0.000000000000000000, 6.152979890951074893 ) ) ;
#54734 = CARTESIAN_POINT ( 'NONE',  ( -14.85781100069234917, 0.000000000000000000, 2.858119855775270945 ) ) ;
#54735 = VECTOR ( 'NONE', #26171, 999.9999999999998863 ) ;
#54736 = DIRECTION ( 'NONE',  ( -0.6427681459581293666, -0.7660444431189770143, -0.005002170337467561935 ) ) ;
#54737 = ORIENTED_EDGE ( 'NONE', *, *, #24419, .T. ) ;
#54738 = CARTESIAN_POINT ( 'NONE',  ( -25.20123094555300369, 0.000000000000000000, 6.470945668149052032 ) ) ;
#54739 = ORIENTED_EDGE ( 'NONE', *, *, #12644, .F. ) ;
#54740 = VECTOR ( 'NONE', #4535, 1000.000000000000000 ) ;
#54741 = EDGE_CURVE ( 'NONE', #48042, #5616, #9428, .T. ) ;
#54742 = B_SPLINE_CURVE_WITH_KNOTS ( 'NONE', 3,
 ( #42743, #33412, #7555, #51570, #33669, #55530, #42205, #54684, #20886, #3848, #46745, #33965 ),
 .UNSPECIFIED., .F., .F.,
 ( 4, 1, 1, 2, 2, 1, 1, 4 ),
 ( 0.7429994551377537837, 0.7471935825069564441, 0.7492906461915580518, 0.7498149121127086758, 0.7500770450732842098, 0.7503391780338596329, 0.7513877098761616580, 0.7597759646145790802 ),
 .UNSPECIFIED. ) ;
#54743 = DIRECTION ( 'NONE',  ( -0.6427681459581293666, -0.7660444431189770143, -0.005002170337467561935 ) ) ;
#54744 = DIRECTION ( 'NONE',  ( 0.007781995580012663651, -3.146120232559066537E-19, -0.9999697198139514409 ) ) ;
#54745 = CARTESIAN_POINT ( 'NONE',  ( -17.73140113748535285, 0.000000000000000000, 13.85752530597602039 ) ) ;
#54746 = DIRECTION ( 'NONE',  ( -0.7660212471507179544, -0.6427876096865405842, -0.005961354470445141482 ) ) ;
#54747 = CARTESIAN_POINT ( 'NONE',  ( -10.84028925556084388, -0.1191753592594197858, 11.14116300850493246 ) ) ;
#54748 = EDGE_CURVE ( 'NONE', #10989, #44493, #43507, .T. ) ;
#54749 = ADVANCED_FACE ( 'NONE', ( #52026 ), #26755, .F. ) ;
#54750 = VECTOR ( 'NONE', #43519, 999.9999999999998863 ) ;
#54751 = CARTESIAN_POINT ( 'NONE',  ( -22.36868959911851462, 19.74370688441071309, -4.657437592157546824 ) ) ;
#54752 = VECTOR ( 'NONE', #32763, 999.9999999999998863 ) ;
#54753 = EDGE_LOOP ( 'NONE', ( #15148, #11627, #42645, #35384 ) ) ;
#54754 = DIRECTION ( 'NONE',  ( -0.000000000000000000, -0.000000000000000000, 1.000000000000000000 ) ) ;
#54755 = CARTESIAN_POINT ( 'NONE',  ( -1.246832498358330099E-15, 0.000000000000000000, 0.000000000000000000 ) ) ;
#54756 = CARTESIAN_POINT ( 'NONE',  ( -15.19945166386478519, 1.257817950434004128, 4.849597862992245823 ) ) ;
#54757 = CARTESIAN_POINT ( 'NONE',  ( -12.07527617786294449, 1.419719901456504285, 3.901770690733497915 ) ) ;
#54758 = CARTESIAN_POINT ( 'NONE',  ( -49.27554558092695913, 2.476975532698160620, -5.000000000000000000 ) ) ;
#54759 = CARTESIAN_POINT ( 'NONE',  ( -13.83747589997588712, 2.391131607591507446, 6.180521011059407321 ) ) ;
#54760 = DIRECTION ( 'NONE',  ( -0.6427681459581293666, -0.7660444431189770143, -0.005002170337467561935 ) ) ;
#54761 = CARTESIAN_POINT ( 'NONE',  ( -19.60990026154428278, 0.000000000000000000, 4.498472333781370125 ) ) ;
#54762 = DIRECTION ( 'NONE',  ( 0.005961354470445682716, -0.6427876096865404731, -0.7660212471507180654 ) ) ;
#54763 = EDGE_CURVE ( 'NONE', #13999, #30111, #35548, .T. ) ;
#54764 = VERTEX_POINT ( 'NONE', #39818 ) ;
#54765 = DIRECTION ( 'NONE',  ( -0.9999697198139514409, -0.000000000000000000, -0.007781995580013368816 ) ) ;
#54766 = CARTESIAN_POINT ( 'NONE',  ( -15.62884970628905457, -4.241740624735664156, 2.816763367194973000 ) ) ;
#54767 = VERTEX_POINT ( 'NONE', #43778 ) ;
#54768 = AXIS2_PLACEMENT_3D ( 'NONE', #48360, #10028, #27337 ) ;
#54769 = CARTESIAN_POINT ( 'NONE',  ( -20.87535245856507515, -2.137015261443157232, 8.297833671620280072 ) ) ;
#54770 = CARTESIAN_POINT ( 'NONE',  ( -10.27421835998572064, 0.000000000000000000, 10.96090226820206048 ) ) ;
#54771 = AXIS2_PLACEMENT_3D ( 'NONE', #15769, #32808, #33393 ) ;
#54772 = VERTEX_POINT ( 'NONE', #44614 ) ;
#54773 = VECTOR ( 'NONE', #18981, 1000.000000000000114 ) ;
#54774 = VERTEX_POINT ( 'NONE', #1175 ) ;
#54775 = DIRECTION ( 'NONE',  ( 0.005002170337468016433, -0.7660444431189770143, -0.6427681459581293666 ) ) ;
#54776 = EDGE_CURVE ( 'NONE', #31643, #16374, #47795, .T. ) ;
#54777 = ORIENTED_EDGE ( 'NONE', *, *, #44200, .T. ) ;
#54778 = EDGE_LOOP ( 'NONE', ( #3795, #17792, #37531, #38959, #39782 ) ) ;
#54779 = EDGE_LOOP ( 'NONE', ( #23273, #5175, #14111, #9053 ) ) ;
#54780 = EDGE_CURVE ( 'NONE', #18328, #14930, #35019, .T. ) ;
#54781 = FACE_OUTER_BOUND ( 'NONE', #49671, .T. ) ;
#54782 = AXIS2_PLACEMENT_3D ( 'NONE', #14998, #6470, #14176 ) ;
#54783 = CARTESIAN_POINT ( 'NONE',  ( -66.59971854373151245, -9.331868537061321689, 6.321089406856088111 ) ) ;
#54784 = LINE ( 'NONE', #41999, #52075 ) ;
#54785 = VECTOR ( 'NONE', #27819, 1000.000000000000227 ) ;
#54786 = ORIENTED_EDGE ( 'NONE', *, *, #38217, .T. ) ;
#54787 = EDGE_CURVE ( 'NONE', #8286, #54291, #26204, .T. ) ;
#54788 = ORIENTED_EDGE ( 'NONE', *, *, #37925, .F. ) ;
#54789 = VECTOR ( 'NONE', #55834, 1000.000000000000227 ) ;
#54790 = CARTESIAN_POINT ( 'NONE',  ( -66.57865728943677652, 2.471980953266950110E-14, 5.126821739293251134 ) ) ;
#54791 = DIRECTION ( 'NONE',  ( -0.5364919789714478471, 0.6444004775717705469, -0.5449076811759709926 ) ) ;
#54792 = EDGE_LOOP ( 'NONE', ( #46411, #31944, #27168, #23241 ) ) ;
#54793 = CARTESIAN_POINT ( 'NONE',  ( -17.88167136688104719, 0.000000000000000000, 7.466578369107171653 ) ) ;
#54794 = ORIENTED_EDGE ( 'NONE', *, *, #49105, .T. ) ;
#54795 = PLANE ( 'NONE',  #27627 ) ;
#54796 = CARTESIAN_POINT ( 'NONE',  ( -15.04630770547183971, 2.714935509636507316, 7.181489704315874079 ) ) ;
#54797 = ADVANCED_FACE ( 'NONE', ( #40378 ), #39250, .F. ) ;
#54798 = VERTEX_POINT ( 'NONE', #52859 ) ;
#54799 = PLANE ( 'NONE',  #20980 ) ;
#54800 = EDGE_CURVE ( 'NONE', #29572, #14416, #18505, .T. ) ;
#54801 = EDGE_CURVE ( 'NONE', #10129, #52847, #21576, .T. ) ;
#54802 = VECTOR ( 'NONE', #11654, 1000.000000000000227 ) ;
#54803 = CARTESIAN_POINT ( 'NONE',  ( -21.47263955680318404, 0.000000000000000000, 5.022634149262071190 ) ) ;
#54804 = ORIENTED_EDGE ( 'NONE', *, *, #29100, .T. ) ;
#54805 = CARTESIAN_POINT ( 'NONE',  ( -12.26423545659806003, 0.000000000000000000, 2.139639520751795310 ) ) ;
#54806 = VECTOR ( 'NONE', #48881, 1000.000000000000227 ) ;
#54807 = PLANE ( 'NONE',  #49153 ) ;
#54808 = ADVANCED_FACE ( 'NONE', ( #14280 ), #48315, .F. ) ;
#54809 = VERTEX_POINT ( 'NONE', #9992 ) ;
#54810 = AXIS2_PLACEMENT_3D ( 'NONE', #47791, #21663, #8897 ) ;
#54811 = EDGE_CURVE ( 'NONE', #35804, #1119, #26457, .T. ) ;
#54812 = LINE ( 'NONE', #11383, #48264 ) ;
#54813 = DIRECTION ( 'NONE',  ( -0.6427681459581293666, -0.7660444431189770143, -0.005002170337467561935 ) ) ;
#54814 = LINE ( 'NONE', #23600, #55758 ) ;
#54815 = CARTESIAN_POINT ( 'NONE',  ( 2.072287782118878319, 0.000000000000000000, -2.950529333540147015 ) ) ;
#54816 = DIRECTION ( 'NONE',  ( -0.3313982828793700097, 0.4028455766673915694, -0.8531650599175529814 ) ) ;
#54817 = ADVANCED_FACE ( 'NONE', ( #27300 ), #9735, .F. ) ;
#54818 = LINE ( 'NONE', #33267, #32516 ) ;
#54819 = CARTESIAN_POINT ( 'NONE',  ( -10.41874342548586085, 8.040039804732380446, 0.8286201928109698800 ) ) ;
#54820 = VECTOR ( 'NONE', #49309, 1000.000000000000227 ) ;
#54821 = ORIENTED_EDGE ( 'NONE', *, *, #32325, .F. ) ;
#54822 = CARTESIAN_POINT ( 'NONE',  ( -18.24553309218274322, -0.1191753592594166911, 7.363743684915764476 ) ) ;
#54823 = LINE ( 'NONE', #7395, #30419 ) ;
#54824 = CARTESIAN_POINT ( 'NONE',  ( -69.65680208973252263, -0.6014278869996851906, 7.567125991932363682 ) ) ;
#54825 = ORIENTED_EDGE ( 'NONE', *, *, #16299, .F. ) ;
#54826 = VECTOR ( 'NONE', #14106, 1000.000000000000000 ) ;
#54827 = DIRECTION ( 'NONE',  ( -0.5364919789714478471, 0.6444004775717705469, -0.5449076811759709926 ) ) ;
#54828 = PLANE ( 'NONE',  #45405 ) ;
#54829 = AXIS2_PLACEMENT_3D ( 'NONE', #9085, #47725, #25859 ) ;
#54830 = EDGE_CURVE ( 'NONE', #44660, #51166, #48898, .T. ) ;
#54831 = EDGE_CURVE ( 'NONE', #16476, #18331, #27043, .T. ) ;
#54832 = FACE_OUTER_BOUND ( 'NONE', #36340, .T. ) ;
#54833 = DIRECTION ( 'NONE',  ( 0.7660212471507180654, -0.6427876096865404731, 0.005961354470445141482 ) ) ;
#54834 = CARTESIAN_POINT ( 'NONE',  ( -15.55561282917033594, 0.000000000000000000, 7.115348224689455492 ) ) ;
#54835 = EDGE_CURVE ( 'NONE', #33685, #55481, #45200, .T. ) ;
#54836 = ORIENTED_EDGE ( 'NONE', *, *, #25324, .T. ) ;
#54837 = VECTOR ( 'NONE', #33902, 999.9999999999998863 ) ;
#54838 = VECTOR ( 'NONE', #31660, 1000.000000000000114 ) ;
#54839 = EDGE_LOOP ( 'NONE', ( #2737, #25522, #7898, #2093 ) ) ;
#54840 = CARTESIAN_POINT ( 'NONE',  ( 2.072287782118878319, 0.000000000000000000, -2.950529333540147015 ) ) ;
#54841 = CARTESIAN_POINT ( 'NONE',  ( -11.21901323774118708, 0.000000000000000000, 1.039777472322872098 ) ) ;
#54842 = VERTEX_POINT ( 'NONE', #31848 ) ;
#54843 = FACE_OUTER_BOUND ( 'NONE', #17638, .T. ) ;
#54844 = ORIENTED_EDGE ( 'NONE', *, *, #28090, .T. ) ;
#54845 = DIRECTION ( 'NONE',  ( 0.7660212471507180654, -0.6427876096865404731, 0.005961354470445141482 ) ) ;
#54846 = AXIS2_PLACEMENT_3D ( 'NONE', #51053, #46817, #15860 ) ;
#54847 = EDGE_LOOP ( 'NONE', ( #27424, #37753, #18974, #35765 ) ) ;
#54848 = EDGE_LOOP ( 'NONE', ( #15236, #4333, #40199, #55091 ) ) ;
#54849 = ORIENTED_EDGE ( 'NONE', *, *, #11319, .T. ) ;
#54850 = VECTOR ( 'NONE', #23466, 999.9999999999998863 ) ;
#54851 = CARTESIAN_POINT ( 'NONE',  ( -15.50102849149811135, -0.1191753592594197858, 12.95155240711365430 ) ) ;
#54852 = FACE_OUTER_BOUND ( 'NONE', #11531, .T. ) ;
#54853 = CIRCLE ( 'NONE', #34040, 0.5000000000000004441 ) ;
#54854 = DIRECTION ( 'NONE',  ( 0.007781995580012663651, 0.000000000000000000, -0.9999697198139515519 ) ) ;
#54855 = EDGE_LOOP ( 'NONE', ( #20057, #44309, #18511, #46149, #42454 ) ) ;
#54856 = DIRECTION ( 'NONE',  ( -0.7660212471507179544, -0.6427876096865405842, -0.005961354470445141482 ) ) ;
#54857 = ADVANCED_FACE ( 'NONE', ( #7139 ), #54269, .F. ) ;
#54858 = AXIS2_PLACEMENT_3D ( 'NONE', #34092, #12771, #42022 ) ;
#54859 = ORIENTED_EDGE ( 'NONE', *, *, #17724, .T. ) ;
#54860 = VERTEX_POINT ( 'NONE', #32140 ) ;
#54861 = ORIENTED_EDGE ( 'NONE', *, *, #15121, .T. ) ;
#54862 = VECTOR ( 'NONE', #53483, 1000.000000000000227 ) ;
#54863 = CARTESIAN_POINT ( 'NONE',  ( -19.08133622045208355, 0.000000000000000000, 8.195906439434676116 ) ) ;
#54864 = AXIS2_PLACEMENT_3D ( 'NONE', #46, #340, #5197 ) ;
#54865 = CARTESIAN_POINT ( 'NONE',  ( -17.93139508144814442, 0.000000000000000000, 13.85596890686001537 ) ) ;
#54866 = ORIENTED_EDGE ( 'NONE', *, *, #54945, .F. ) ;
#54867 = VECTOR ( 'NONE', #14545, 999.9999999999998863 ) ;
#54868 = CARTESIAN_POINT ( 'NONE',  ( -10.69044919664899318, 0.000000000000000000, 4.737211577976179200 ) ) ;
#54869 = ORIENTED_EDGE ( 'NONE', *, *, #42916, .T. ) ;
#54870 = FACE_OUTER_BOUND ( 'NONE', #5985, .T. ) ;
#54871 = DIRECTION ( 'NONE',  ( -0.000000000000000000, -0.000000000000000000, 1.000000000000000000 ) ) ;
#54872 = VECTOR ( 'NONE', #28347, 1000.000000000000227 ) ;
#54873 = EDGE_CURVE ( 'NONE', #13455, #156, #28141, .T. ) ;
#54874 = ORIENTED_EDGE ( 'NONE', *, *, #5368, .T. ) ;
#54875 = DIRECTION ( 'NONE',  ( 0.9999697198139515519, 0.000000000000000000, 0.007781995580013368816 ) ) ;
#54876 = VERTEX_POINT ( 'NONE', #53435 ) ;
#54877 = ADVANCED_FACE ( 'NONE', ( #19899 ), #19060, .F. ) ;
#54878 = EDGE_CURVE ( 'NONE', #40214, #50606, #41207, .T. ) ;
#54879 = AXIS2_PLACEMENT_3D ( 'NONE', #13921, #8556, #51700 ) ;
#54880 = PLANE ( 'NONE',  #28303 ) ;
#54881 = VECTOR ( 'NONE', #32682, 1000.000000000000227 ) ;
#54882 = LINE ( 'NONE', #49787, #13000 ) ;
#54883 = CARTESIAN_POINT ( 'NONE',  ( -11.35376238306358410, 0.000000000000000000, 4.562723507797191047 ) ) ;
#54884 = DIRECTION ( 'NONE',  ( 0.5449076811759707706, 0.6444004775717708799, -0.5364919789714476250 ) ) ;
#54885 = DIRECTION ( 'NONE',  ( -0.6427681459581293666, -0.7660444431189770143, -0.005002170337467561935 ) ) ;
#54886 = DIRECTION ( 'NONE',  ( 0.3583679495452941066, 0.9335804264972041855, -0.000000000000000000 ) ) ;
#54887 = ORIENTED_EDGE ( 'NONE', *, *, #12269, .T. ) ;
#54888 = ORIENTED_EDGE ( 'NONE', *, *, #44966, .F. ) ;
#54889 = EDGE_CURVE ( 'NONE', #19083, #9775, #19638, .T. ) ;
#54890 = DIRECTION ( 'NONE',  ( 0.000000000000000000, -1.000000000000000000, 0.000000000000000000 ) ) ;
#54891 = FACE_OUTER_BOUND ( 'NONE', #29437, .T. ) ;
#54892 = CARTESIAN_POINT ( 'NONE',  ( -67.78991508493417939, 0.1329061886590362507, 3.332842667189709562 ) ) ;
#54893 = LINE ( 'NONE', #29048, #33027 ) ;
#54894 = EDGE_CURVE ( 'NONE', #56189, #54483, #36675, .T. ) ;
#54895 = DIRECTION ( 'NONE',  ( 0.005002170337468016433, -0.7660444431189770143, -0.6427681459581293666 ) ) ;
#54896 = AXIS2_PLACEMENT_3D ( 'NONE', #50449, #8131, #16345 ) ;
#54897 = FACE_OUTER_BOUND ( 'NONE', #42160, .T. ) ;
#54898 = ORIENTED_EDGE ( 'NONE', *, *, #3288, .F. ) ;
#54899 = VECTOR ( 'NONE', #18565, 1000.000000000000227 ) ;
#54900 = CARTESIAN_POINT ( 'NONE',  ( -18.76354595665420177, -0.1191753592594177458, 14.21882498613976331 ) ) ;
#54901 = LINE ( 'NONE', #50642, #33191 ) ;
#54902 = ORIENTED_EDGE ( 'NONE', *, *, #6294, .F. ) ;
#54903 = PLANE ( 'NONE',  #23860 ) ;
#54904 = CARTESIAN_POINT ( 'NONE',  ( -18.84739110800622797, 4.981562823951511731, 12.37788115850241333 ) ) ;
#54905 = VECTOR ( 'NONE', #26915, 1000.000000000000227 ) ;
#54906 = ORIENTED_EDGE ( 'NONE', *, *, #37093, .T. ) ;
#54907 = ADVANCED_FACE ( 'NONE', ( #6564 ), #24435, .F. ) ;
#54908 = PLANE ( 'NONE',  #34338 ) ;
#54909 = LINE ( 'NONE', #55451, #34224 ) ;
#54910 = AXIS2_PLACEMENT_3D ( 'NONE', #30316, #48170, #14129 ) ;
#54911 = PLANE ( 'NONE',  #32322 ) ;
#54912 = DIRECTION ( 'NONE',  ( -0.5449076811759708816, 0.6444004775717707689, 0.5364919789714475140 ) ) ;
#54913 = B_SPLINE_CURVE_WITH_KNOTS ( 'NONE', 3,
 ( #43934, #53026, #22081, #48480, #9879, #13304, #43647, #30630, #5058, #9600, #9293, #21798, #39117, #47932, #39957, #44488, #35423, #26616, #193, #26924, #1042, #27182, #26087, #39703, #43393, #17843, #780, #14140, #4759, #44238, #39413, #4490, #35712, #5338, #13565, #30876, #17541, #48185, #22387, #18099, #52726, #13833, #4399, #50941, #47838, #17427, #43001, #21712, #25679, #56079, #30528, #39024, #47543, #8658, #3540, #20597, #43306, #8941, #51246, #38171, #55221, #38458, #12363, #55785, #52078, #26243, #42707, #17166 ),
 .UNSPECIFIED., .F., .F.,
 ( 4, 1, 1, 1, 1, 1, 1, 2, 2, 1, 1, 1, 1, 1, 1, 1, 1, 2, 2, 1, 1, 1, 1, 1, 1, 1, 1, 2, 2, 1, 1, 1, 1, 1, 1, 1, 2, 2, 1, 1, 1, 1, 1, 1, 2, 2, 1, 1, 1, 2, 2, 1, 1, 4 ),
 ( 0.000000000000000000, 0.1249999999999907296, 0.1874999999999860945, 0.2187499999999835687, 0.2343749999999822642, 0.2421874999999815703, 0.2460937499999812095, 0.2480468749999808209, 0.2499999999999804323, 0.3749999999999575340, 0.4374999999999463207, 0.4687499999999407141, 0.4843749999999379385, 0.4921874999999364952, 0.4960937499999357736, 0.4980468749999352740, 0.4990234374999349964, 0.4995117187499349409, 0.4999999999999348299, 0.6249999999999096278, 0.6874999999998971933, 0.7187499999998909761, 0.7343749999998877565, 0.7421874999998862021, 0.7460937499998856470, 0.7480468749998852029, 0.7490234374998852029, 0.7495117187498852029, 0.7499999999998853140, 0.8124999999999193978, 0.8437499999999364952, 0.8593749999999450440, 0.8671874999999493738, 0.8710937499999514833, 0.8730468749999525935, 0.8740234374999530376, 0.8745117187499533706, 0.8749999999999535927, 0.9062499999999694689, 0.9218749999999774625, 0.9296874999999815703, 0.9335937499999836797, 0.9355468749999849010, 0.9365234374999853451, 0.9370117187499856781, 0.9374999999999860112, 0.9531249999999898970, 0.9609374999999920064, 0.9619140624999922284, 0.9624023437499923395, 0.9628906249999924505, 0.9648437499999927836, 0.9687499999999936717, 1.000000000000000000 ),
 .UNSPECIFIED. ) ;
#54914 = FACE_OUTER_BOUND ( 'NONE', #42465, .T. ) ;
#54915 = EDGE_CURVE ( 'NONE', #17921, #41488, #6035, .T. ) ;
#54916 = ORIENTED_EDGE ( 'NONE', *, *, #18004, .F. ) ;
#54917 = VECTOR ( 'NONE', #31355, 1000.000000000000227 ) ;
#54918 = VECTOR ( 'NONE', #37065, 999.9999999999998863 ) ;
#54919 = VERTEX_POINT ( 'NONE', #36968 ) ;
#54920 = CARTESIAN_POINT ( 'NONE',  ( -69.19743948421294988, -0.6012349891692201354, 6.949370683160942974 ) ) ;
#54921 = DIRECTION ( 'NONE',  ( 0.5364919789714477361, 0.6444004775717706579, 0.5449076811759711036 ) ) ;
#54922 = DIRECTION ( 'NONE',  ( -0.9321478471874540261, 0.000000000000000000, 0.3620778797217457656 ) ) ;
#54923 = VECTOR ( 'NONE', #11480, 1000.000000000000114 ) ;
#54924 = CARTESIAN_POINT ( 'NONE',  ( -69.59783862807636012, -0.6008070088998225255, -7.493102809087827332 ) ) ;
#54926 = PLANE ( 'NONE',  #37353 ) ;
#54925 = VECTOR ( 'NONE', #34835, 999.9999999999998863 ) ;
#54927 = LINE ( 'NONE', #16033, #29473 ) ;
#54928 = VECTOR ( 'NONE', #13019, 1000.000000000000227 ) ;
#54929 = ORIENTED_EDGE ( 'NONE', *, *, #18025, .F. ) ;
#54930 = DIRECTION ( 'NONE',  ( 0.5449076811759707706, 0.6444004775717708799, -0.5364919789714476250 ) ) ;
#54931 = VECTOR ( 'NONE', #26569, 999.9999999999998863 ) ;
#54932 = DIRECTION ( 'NONE',  ( -0.5449076811759708816, 0.6444004775717707689, 0.5364919789714475140 ) ) ;
#54933 = VECTOR ( 'NONE', #29124, 1000.000000000000227 ) ;
#54934 = DIRECTION ( 'NONE',  ( 0.5364919789714477361, 0.6444004775717706579, 0.5449076811759711036 ) ) ;
#54935 = ORIENTED_EDGE ( 'NONE', *, *, #49772, .F. ) ;
#54936 = FACE_OUTER_BOUND ( 'NONE', #51498, .T. ) ;
#54937 = DIRECTION ( 'NONE',  ( -0.7660212471507179544, -0.6427876096865405842, -0.005961354470445141482 ) ) ;
#54938 = DIRECTION ( 'NONE',  ( 0.6427681459581294776, -0.7660444431189769032, 0.005002170337467562802 ) ) ;
#54939 = ORIENTED_EDGE ( 'NONE', *, *, #4620, .F. ) ;
#54940 = CARTESIAN_POINT ( 'NONE',  ( -13.46258265577981383, 0.000000000000000000, 2.699651831784322997 ) ) ;
#54941 = ADVANCED_FACE ( 'NONE', ( #53992 ), #15108, .F. ) ;
#54942 = ORIENTED_EDGE ( 'NONE', *, *, #9859, .F. ) ;
#54943 = VECTOR ( 'NONE', #20181, 1000.000000000000000 ) ;
#54944 = ORIENTED_EDGE ( 'NONE', *, *, #49755, .T. ) ;
#54945 = EDGE_CURVE ( 'NONE', #21963, #12571, #15623, .T. ) ;
#54946 = ORIENTED_EDGE ( 'NONE', *, *, #13055, .T. ) ;
#54947 = ADVANCED_FACE ( 'NONE', ( #49461 ), #28723, .F. ) ;
#54948 = EDGE_LOOP ( 'NONE', ( #33633, #47953, #46665, #21823 ) ) ;
#54949 = FACE_OUTER_BOUND ( 'NONE', #50259, .T. ) ;
#54950 = VECTOR ( 'NONE', #33652, 1000.000000000000114 ) ;
#54952 = EDGE_CURVE ( 'NONE', #18056, #36712, #23604, .T. ) ;
#54951 = ORIENTED_EDGE ( 'NONE', *, *, #8270, .F. ) ;
#54953 = EDGE_CURVE ( 'NONE', #29572, #22170, #14532, .T. ) ;
#54954 = ADVANCED_FACE ( 'NONE', ( #27596 ), #23348, .F. ) ;
#54955 = ORIENTED_EDGE ( 'NONE', *, *, #23987, .T. ) ;
#54956 = DIRECTION ( 'NONE',  ( 0.000000000000000000, -1.000000000000000000, 0.000000000000000000 ) ) ;
#54957 = ORIENTED_EDGE ( 'NONE', *, *, #34476, .F. ) ;
#54958 = CIRCLE ( 'NONE', #46763, 1.750000000000003331 ) ;
#54959 = ORIENTED_EDGE ( 'NONE', *, *, #9842, .F. ) ;
#54960 = VECTOR ( 'NONE', #13893, 1000.000000000000000 ) ;
#54961 = VECTOR ( 'NONE', #48953, 999.9999999999998863 ) ;
#54962 = CARTESIAN_POINT ( 'NONE',  ( -17.80573849810343390, 2.714935509636509536, 3.511664592573657373 ) ) ;
#54963 = LINE ( 'NONE', #7521, #46615 ) ;
#54964 = DIRECTION ( 'NONE',  ( -1.000000000000000000, 0.000000000000000000, 0.000000000000000000 ) ) ;
#54965 = CARTESIAN_POINT ( 'NONE',  ( 2.072287782118878319, 0.000000000000000000, -2.950529333540147015 ) ) ;
#54966 = DIRECTION ( 'NONE',  ( 0.007781995580012663651, 0.000000000000000000, -0.9999697198139515519 ) ) ;
#54967 = ORIENTED_EDGE ( 'NONE', *, *, #39714, .F. ) ;
#54968 = AXIS2_PLACEMENT_3D ( 'NONE', #2087, #53509, #10907 ) ;
#54969 = VERTEX_POINT ( 'NONE', #1739 ) ;
#54970 = VECTOR ( 'NONE', #13871, 1000.000000000000114 ) ;
#54971 = EDGE_CURVE ( 'NONE', #23998, #16476, #11670, .T. ) ;
#54972 = DIRECTION ( 'NONE',  ( 0.007781995580012663651, -3.146120232559066537E-19, -0.9999697198139514409 ) ) ;
#54973 = DIRECTION ( 'NONE',  ( -0.005002170337468016433, -0.7660444431189770143, 0.6427681459581293666 ) ) ;
#54974 = AXIS2_PLACEMENT_3D ( 'NONE', #51078, #42843, #16730 ) ;
#54975 = EDGE_CURVE ( 'NONE', #12964, #6316, #47419, .T. ) ;
#54976 = CARTESIAN_POINT ( 'NONE',  ( -28.11332263830040645, 16.42704145284338324, -4.694618095106484645 ) ) ;
#54977 = VECTOR ( 'NONE', #45338, 999.9999999999998863 ) ;
#54978 = CARTESIAN_POINT ( 'NONE',  ( -11.74346145839723654, -0.1191753592594190225, 7.779932815735107532 ) ) ;
#54979 = ADVANCED_FACE ( 'NONE', ( #34104 ), #29842, .F. ) ;
#54980 = CARTESIAN_POINT ( 'NONE',  ( -19.05678739329382054, 0.000000000000000000, 5.041434869409770592 ) ) ;
#54981 = CARTESIAN_POINT ( 'NONE',  ( -28.93137873341882127, 0.000000000000000000, 8.119251130998824451 ) ) ;
#54982 = ORIENTED_EDGE ( 'NONE', *, *, #20794, .F. ) ;
#54983 = CARTESIAN_POINT ( 'NONE',  ( -19.12962290826653700, 0.000000000000000000, 14.40064212555863854 ) ) ;
#54984 = EDGE_LOOP ( 'NONE', ( #14440, #51451, #4304, #20935 ) ) ;
#54985 = EDGE_CURVE ( 'NONE', #2867, #11647, #17059, .T. ) ;
#54986 = CARTESIAN_POINT ( 'NONE',  ( -18.14918837326463219, 0.000000000000000000, 7.833828559712929795 ) ) ;
#54987 = DIRECTION ( 'NONE',  ( 0.000000000000000000, -1.000000000000000000, 0.000000000000000000 ) ) ;
#54988 = DIRECTION ( 'NONE',  ( 0.9999697198139515519, 0.000000000000000000, 0.007781995580013368816 ) ) ;
#54989 = FACE_OUTER_BOUND ( 'NONE', #24461, .T. ) ;
#54990 = CARTESIAN_POINT ( 'NONE',  ( -3.360905869600907092, 1.745854407020028306E-14, 2.600000000000000089 ) ) ;
#54991 = DIRECTION ( 'NONE',  ( 0.005961354470445682716, -0.6427876096865404731, -0.7660212471507180654 ) ) ;
#54992 = VECTOR ( 'NONE', #4445, 999.9999999999998863 ) ;
#54993 = EDGE_LOOP ( 'NONE', ( #28744, #14653, #52953, #39507 ) ) ;
#54994 = ORIENTED_EDGE ( 'NONE', *, *, #6062, .T. ) ;
#54995 = LINE ( 'NONE', #27767, #13024 ) ;
#54996 = FACE_OUTER_BOUND ( 'NONE', #17013, .T. ) ;
#54997 = LINE ( 'NONE', #29130, #43301 ) ;
#54998 = VECTOR ( 'NONE', #35025, 1000.000000000000227 ) ;
#54999 = CARTESIAN_POINT ( 'NONE',  ( -9.999901398370125705, 0.000000000000000000, 1.249270938769537542 ) ) ;
#55000 = VECTOR ( 'NONE', #38585, 1000.000000000000000 ) ;
#55001 = FACE_OUTER_BOUND ( 'NONE', #41896, .T. ) ;
#55002 = DIRECTION ( 'NONE',  ( -0.1139275668495183386, 0.9934890585767658377, 4.694855797473113547E-16 ) ) ;
#55003 = DIRECTION ( 'NONE',  ( 0.007781995580012662783, 0.000000000000000000, -0.9999697198139514409 ) ) ;
#55004 = AXIS2_PLACEMENT_3D ( 'NONE', #4756, #43391, #13301 ) ;
#55005 = LINE ( 'NONE', #3011, #33279 ) ;
#55006 = CARTESIAN_POINT ( 'NONE',  ( -7.034459185439723150, -6.761815089084117325, -0.4859507367995170024 ) ) ;
#55007 = ORIENTED_EDGE ( 'NONE', *, *, #21287, .T. ) ;
#55008 = VERTEX_POINT ( 'NONE', #47138 ) ;
#55009 = AXIS2_PLACEMENT_3D ( 'NONE', #47258, #29956, #46410 ) ;
#55010 = EDGE_CURVE ( 'NONE', #3706, #49287, #20162, .T. ) ;
#55011 = VECTOR ( 'NONE', #47614, 1000.000000000000227 ) ;
#55012 = ORIENTED_EDGE ( 'NONE', *, *, #28944, .T. ) ;
#55013 = VECTOR ( 'NONE', #39338, 999.9999999999998863 ) ;
#55014 = EDGE_LOOP ( 'NONE', ( #29007, #42930, #33557, #14447 ) ) ;
#55015 = EDGE_CURVE ( 'NONE', #36809, #27553, #50831, .T. ) ;
#55016 = ORIENTED_EDGE ( 'NONE', *, *, #45773, .F. ) ;
#55017 = ORIENTED_EDGE ( 'NONE', *, *, #28197, .F. ) ;
#55018 = DIRECTION ( 'NONE',  ( 0.000000000000000000, -0.000000000000000000, -1.000000000000000000 ) ) ;
#55019 = FACE_OUTER_BOUND ( 'NONE', #27115, .T. ) ;
#55020 = DIRECTION ( 'NONE',  ( 0.007781995580012662783, 0.000000000000000000, -0.9999697198139514409 ) ) ;
#55021 = EDGE_CURVE ( 'NONE', #9595, #26049, #25556, .T. ) ;
#55022 = ADVANCED_FACE ( 'NONE', ( #8529 ), #11927, .F. ) ;
#55023 = EDGE_CURVE ( 'NONE', #16052, #18488, #21009, .T. ) ;
#55024 = EDGE_LOOP ( 'NONE', ( #55291, #3407, #36638, #41460 ) ) ;
#55025 = DIRECTION ( 'NONE',  ( 0.007781995580012663651, -3.146120232559066537E-19, -0.9999697198139514409 ) ) ;
#55026 = ORIENTED_EDGE ( 'NONE', *, *, #35223, .F. ) ;
#55027 = CARTESIAN_POINT ( 'NONE',  ( -64.58934917682360322, -11.11443825362803395, 0.6542134465202145144 ) ) ;
#55028 = EDGE_CURVE ( 'NONE', #24728, #52574, #38640, .T. ) ;
#55029 = ORIENTED_EDGE ( 'NONE', *, *, #47979, .F. ) ;
#55030 = AXIS2_PLACEMENT_3D ( 'NONE', #16822, #47469, #25071 ) ;
#55031 = CARTESIAN_POINT ( 'NONE',  ( -67.30865983991493806, -9.413165815805299985, 5.846634436079878760 ) ) ;
#55032 = CARTESIAN_POINT ( 'NONE',  ( -15.37089526832641617, -1.165603555308157846, 2.814709981181112486 ) ) ;
#55033 = CARTESIAN_POINT ( 'NONE',  ( -12.80458192191714595, 0.000000000000000000, 11.86454056839041726 ) ) ;
#55034 = ORIENTED_EDGE ( 'NONE', *, *, #45511, .F. ) ;
#55035 = LINE ( 'NONE', #3041, #21935 ) ;
#55036 = ORIENTED_EDGE ( 'NONE', *, *, #18968, .T. ) ;
#55037 = DIRECTION ( 'NONE',  ( -0.7660212471507179544, -0.6427876096865405842, -0.005961354470445141482 ) ) ;
#55038 = CIRCLE ( 'NONE', #54151, 3.457106781186553235 ) ;
#55039 = DIRECTION ( 'NONE',  ( -0.5364919789714478471, 0.6444004775717705469, -0.5449076811759709926 ) ) ;
#55040 = EDGE_CURVE ( 'NONE', #54376, #48873, #46571, .T. ) ;
#55041 = LINE ( 'NONE', #54195, #17890 ) ;
#55042 = VECTOR ( 'NONE', #54988, 999.9999999999998863 ) ;
#55043 = DIRECTION ( 'NONE',  ( -0.7660212471507179544, -0.6427876096865405842, -0.005961354470445141482 ) ) ;
#55044 = CYLINDRICAL_SURFACE ( 'NONE', #40181, 5.991923709989089630 ) ;
#55045 = CARTESIAN_POINT ( 'NONE',  ( 5.223256457478858472, -6.243920421220472861, 1.967953638240999670 ) ) ;
#55046 = EDGE_CURVE ( 'NONE', #46078, #43561, #16206, .T. ) ;
#55047 = CARTESIAN_POINT ( 'NONE',  ( -19.60912206198628027, -0.1191753592594197858, 4.398475361799976113 ) ) ;
#55048 = DIRECTION ( 'NONE',  ( 0.005002170337468016433, -0.7660444431189770143, -0.6427681459581293666 ) ) ;
#55049 = ORIENTED_EDGE ( 'NONE', *, *, #27520, .F. ) ;
#55050 = DIRECTION ( 'NONE',  ( 0.000000000000000000, 0.000000000000000000, 1.000000000000000000 ) ) ;
#55051 = ORIENTED_EDGE ( 'NONE', *, *, #4342, .F. ) ;
#55052 = ADVANCED_FACE ( 'NONE', ( #46880 ), #51423, .F. ) ;
#55053 = DIRECTION ( 'NONE',  ( -0.005961354470445682716, -0.6427876096865404731, 0.7660212471507180654 ) ) ;
#55054 = PLANE ( 'NONE',  #47756 ) ;
#55055 = FACE_OUTER_BOUND ( 'NONE', #42650, .T. ) ;
#55056 = DIRECTION ( 'NONE',  ( 0.5449076811759707706, 0.6444004775717708799, -0.5364919789714476250 ) ) ;
#55057 = PLANE ( 'NONE',  #14123 ) ;
#55058 = EDGE_CURVE ( 'NONE', #34537, #41838, #55964, .T. ) ;
#55059 = AXIS2_PLACEMENT_3D ( 'NONE', #2593, #7149, #50587 ) ;
#55060 = DIRECTION ( 'NONE',  ( 0.000000000000000000, -0.000000000000000000, -1.000000000000000000 ) ) ;
#55061 = FILL_AREA_STYLE ('',( #7083 ) ) ;
#55062 = ORIENTED_EDGE ( 'NONE', *, *, #52393, .F. ) ;
#55063 = LINE ( 'NONE', #50214, #15607 ) ;
#55064 = DIRECTION ( 'NONE',  ( 0.9999697198139515519, 0.000000000000000000, 0.007781995580013368816 ) ) ;
#55065 = DIRECTION ( 'NONE',  ( -0.5449076811759708816, 0.6444004775717707689, 0.5364919789714475140 ) ) ;
#55066 = DIRECTION ( 'NONE',  ( 1.000000000000000000, 0.000000000000000000, 0.000000000000000000 ) ) ;
#55067 = DIRECTION ( 'NONE',  ( -0.8660254037844380415, -0.5000000000000011102, -0.000000000000000000 ) ) ;
#55068 = CARTESIAN_POINT ( 'NONE',  ( -58.00000000000000711, -9.000000000000000000, -2.749999999999994671 ) ) ;
#55069 = FACE_OUTER_BOUND ( 'NONE', #4987, .T. ) ;
#55070 = FACE_OUTER_BOUND ( 'NONE', #14165, .T. ) ;
#55071 = DIRECTION ( 'NONE',  ( 0.5364919789714477361, 0.6444004775717706579, 0.5449076811759711036 ) ) ;
#55072 = EDGE_LOOP ( 'NONE', ( #34024, #5306, #1362, #18523 ) ) ;
#55073 = CARTESIAN_POINT ( 'NONE',  ( -14.00280974873554030, 0.000000000000000000, 12.40921378708904044 ) ) ;
#55074 = PLANE ( 'NONE',  #13302 ) ;
#55075 = ORIENTED_EDGE ( 'NONE', *, *, #14552, .T. ) ;
#55076 = ORIENTED_EDGE ( 'NONE', *, *, #15279, .T. ) ;
#55077 = CARTESIAN_POINT ( 'NONE',  ( 0.3240706152708093812, -3.670543518250628967, -1.335466778558061241E-15 ) ) ;
#55078 = ORIENTED_EDGE ( 'NONE', *, *, #34153, .T. ) ;
#55079 = EDGE_LOOP ( 'NONE', ( #21495, #21862, #55012, #11916 ) ) ;
#55080 = CARTESIAN_POINT ( 'NONE',  ( -12.80458192191714595, 0.000000000000000000, 11.86454056839041726 ) ) ;
#55081 = VECTOR ( 'NONE', #38802, 999.9999999999998863 ) ;
#55082 = EDGE_LOOP ( 'NONE', ( #16321, #49962, #31570, #24007 ) ) ;
#55083 = ORIENTED_EDGE ( 'NONE', *, *, #44725, .T. ) ;
#55084 = ORIENTED_EDGE ( 'NONE', *, *, #31330, .F. ) ;
#55085 = CARTESIAN_POINT ( 'NONE',  ( -12.28435383113503931, 0.000000000000000000, 4.724807443556146680 ) ) ;
#55086 = CARTESIAN_POINT ( 'NONE',  ( -67.27849890436391433, -9.409707134521932304, 7.454917401049827141 ) ) ;
#55087 = DIRECTION ( 'NONE',  ( 0.9999697198139515519, 0.000000000000000000, 0.007781995580013368816 ) ) ;
#55088 = EDGE_CURVE ( 'NONE', #14403, #7048, #21308, .T. ) ;
#55089 = AXIS2_PLACEMENT_3D ( 'NONE', #26909, #31145, #31987 ) ;
#55090 = ORIENTED_EDGE ( 'NONE', *, *, #10065, .T. ) ;
#55091 = ORIENTED_EDGE ( 'NONE', *, *, #2456, .F. ) ;
#55092 = EDGE_CURVE ( 'NONE', #42292, #1604, #46282, .T. ) ;
#55093 = EDGE_CURVE ( 'NONE', #16077, #13531, #54818, .T. ) ;
#55094 = DIRECTION ( 'NONE',  ( -0.5364919789714478471, 0.6444004775717705469, -0.5449076811759709926 ) ) ;
#55095 = FACE_OUTER_BOUND ( 'NONE', #8018, .T. ) ;
#55096 = ORIENTED_EDGE ( 'NONE', *, *, #31652, .T. ) ;
#55097 = PLANE ( 'NONE',  #13751 ) ;
#55098 = ORIENTED_EDGE ( 'NONE', *, *, #24626, .T. ) ;
#55099 = CARTESIAN_POINT ( 'NONE',  ( -18.66354898467281132, 0.000000000000000000, 14.21960318569776582 ) ) ;
#55100 = FACE_OUTER_BOUND ( 'NONE', #8762, .T. ) ;
#55101 = VERTEX_POINT ( 'NONE', #50575 ) ;
#55102 = DIRECTION ( 'NONE',  ( 0.9999697198139515519, 0.000000000000000000, 0.007781995580013368816 ) ) ;
#55103 = CARTESIAN_POINT ( 'NONE',  ( -21.47419595591918906, 0.000000000000000000, 5.222628093224860102 ) ) ;
#55104 = ORIENTED_EDGE ( 'NONE', *, *, #32393, .T. ) ;
#55105 = DIRECTION ( 'NONE',  ( -0.7660212471507179544, -0.6427876096865405842, -0.005961354470445141482 ) ) ;
#55106 = DIRECTION ( 'NONE',  ( 0.5364919789714477361, 0.6444004775717706579, 0.5449076811759711036 ) ) ;
#55107 = CARTESIAN_POINT ( 'NONE',  ( -14.62190858286687956, 0.000000000000000000, 6.553276401004920260 ) ) ;
#55108 = ORIENTED_EDGE ( 'NONE', *, *, #13124, .F. ) ;
#55109 = CARTESIAN_POINT ( 'NONE',  ( -9.966917453940169480, 0.000000000000000000, 5.481506408911723582 ) ) ;
#55110 = LINE ( 'NONE', #11922, #36878 ) ;
#55111 = DIRECTION ( 'NONE',  ( 0.5449076811759707706, 0.6444004775717708799, -0.5364919789714476250 ) ) ;
#55112 = CARTESIAN_POINT ( 'NONE',  ( -8.574951275837294773, -8.254029952494388311, 0.1124287064424994709 ) ) ;
#55113 = EDGE_CURVE ( 'NONE', #51703, #7720, #7391, .T. ) ;
#55114 = PLANE ( 'NONE',  #4992 ) ;
#55115 = DIRECTION ( 'NONE',  ( 0.000000000000000000, -1.000000000000000000, 0.000000000000000000 ) ) ;
#55116 = LINE ( 'NONE', #7690, #38536 ) ;
#55117 = ORIENTED_EDGE ( 'NONE', *, *, #52441, .T. ) ;
#55119 = EDGE_CURVE ( 'NONE', #12509, #35868, #42340, .T. ) ;
#55118 = DIRECTION ( 'NONE',  ( 0.5449076811759707706, 0.6444004775717708799, -0.5364919789714476250 ) ) ;
#55120 = DIRECTION ( 'NONE',  ( 0.000000000000000000, -0.000000000000000000, -1.000000000000000000 ) ) ;
#55121 = DIRECTION ( 'NONE',  ( -0.7660212471507179544, -0.6427876096865405842, -0.005961354470445141482 ) ) ;
#55122 = ORIENTED_EDGE ( 'NONE', *, *, #47171, .T. ) ;
#55123 = LINE ( 'NONE', #15633, #13900 ) ;
#55124 = CARTESIAN_POINT ( 'NONE',  ( 0.3240706152708106025, -3.670543518250628967, -1.335466778558061241E-15 ) ) ;
#55125 = VECTOR ( 'NONE', #14813, 1000.000000000000114 ) ;
#55126 = EDGE_CURVE ( 'NONE', #27103, #27671, #34633, .T. ) ;
#55127 = LINE ( 'NONE', #2845, #39484 ) ;
#55128 = FACE_OUTER_BOUND ( 'NONE', #12812, .T. ) ;
#55129 = FACE_OUTER_BOUND ( 'NONE', #54778, .T. ) ;
#55130 = EDGE_LOOP ( 'NONE', ( #35970, #33564, #18178, #4254, #30425 ) ) ;
#55131 = ORIENTED_EDGE ( 'NONE', *, *, #54780, .F. ) ;
#55132 = CARTESIAN_POINT ( 'NONE',  ( -15.34544032557569437, 0.000000000000000000, 5.808981570069377653 ) ) ;
#55133 = CARTESIAN_POINT ( 'NONE',  ( -25.20123094555300369, 0.000000000000000000, 6.470945668149052032 ) ) ;
#55134 = ORIENTED_EDGE ( 'NONE', *, *, #54470, .F. ) ;
#55135 = DIRECTION ( 'NONE',  ( -0.5449076811759708816, 0.6444004775717707689, 0.5364919789714475140 ) ) ;
#55136 = VERTEX_POINT ( 'NONE', #18440 ) ;
#55137 = CARTESIAN_POINT ( 'NONE',  ( -23.33693525117809386, 0.000000000000000000, 5.746789908705562944 ) ) ;
#55138 = ORIENTED_EDGE ( 'NONE', *, *, #16732, .T. ) ;
#55139 = ORIENTED_EDGE ( 'NONE', *, *, #53990, .T. ) ;
#55140 = ORIENTED_EDGE ( 'NONE', *, *, #12544, .F. ) ;
#55141 = CARTESIAN_POINT ( 'NONE',  ( -16.33317936670417225, 0.000000000000000000, 13.31440848639340224 ) ) ;
#55142 = ADVANCED_FACE ( 'NONE', ( #30688 ), #48840, .F. ) ;
#55143 = DIRECTION ( 'NONE',  ( -0.005961354470445682716, -0.6427876096865404731, 0.7660212471507180654 ) ) ;
#55144 = CARTESIAN_POINT ( 'NONE',  ( -26.13493519185646008, 0.000000000000000000, 7.033017491833586377 ) ) ;
#55145 = FACE_OUTER_BOUND ( 'NONE', #45905, .T. ) ;
#55146 = ORIENTED_EDGE ( 'NONE', *, *, #68, .F. ) ;
#55147 = EDGE_CURVE ( 'NONE', #46316, #32796, #48245, .T. ) ;
#55148 = ADVANCED_FACE ( 'NONE', ( #44297 ), #4546, .F. ) ;
#55149 = ORIENTED_EDGE ( 'NONE', *, *, #43847, .F. ) ;
#55150 = ORIENTED_EDGE ( 'NONE', *, *, #28036, .F. ) ;
#55151 = LINE ( 'NONE', #46920, #40422 ) ;
#55152 = CARTESIAN_POINT ( 'NONE',  ( -14.01545677930355183, 0.000000000000000000, 2.126011111488108174 ) ) ;
#55153 = ORIENTED_EDGE ( 'NONE', *, *, #20954, .T. ) ;
#55154 = CARTESIAN_POINT ( 'NONE',  ( -16.91060339984674599, 2.714935509636507316, 7.905645463759363167 ) ) ;
#55155 = ORIENTED_EDGE ( 'NONE', *, *, #38819, .T. ) ;
#55156 = CARTESIAN_POINT ( 'NONE',  ( -11.84964020568542686, 0.6102101463440048335, 2.485582596757569984 ) ) ;
#55157 = CARTESIAN_POINT ( 'NONE',  ( -12.80458192191714595, 0.000000000000000000, 11.86454056839041726 ) ) ;
#55158 = AXIS2_PLACEMENT_3D ( 'NONE', #2989, #37939, #40607 ) ;
#55159 = ORIENTED_EDGE ( 'NONE', *, *, #44902, .F. ) ;
#55160 = PRODUCT_RELATED_PRODUCT_CATEGORY ( 'part', '', ( #4656 ) ) ;
#55161 = DIRECTION ( 'NONE',  ( -0.5449076811759708816, 0.6444004775717707689, 0.5364919789714475140 ) ) ;
#55162 = ORIENTED_EDGE ( 'NONE', *, *, #24523, .F. ) ;
#55163 = EDGE_CURVE ( 'NONE', #14660, #50517, #26140, .T. ) ;
#55164 = LINE ( 'NONE', #37268, #10153 ) ;
#55165 = LINE ( 'NONE', #25346, #4845 ) ;
#55166 = DIRECTION ( 'NONE',  ( 0.5449076811759707706, 0.6444004775717708799, -0.5364919789714476250 ) ) ;
#55167 = DIRECTION ( 'NONE',  ( 0.9999697198139515519, 0.000000000000000000, 0.007781995580013368816 ) ) ;
#55168 = CARTESIAN_POINT ( 'NONE',  ( -11.61553128243660105, 0.000000000000000000, 4.191354291887420480 ) ) ;
#55169 = CARTESIAN_POINT ( 'NONE',  ( -18.67619601524082285, 0.000000000000000000, 3.936400510096834893 ) ) ;
#55170 = VERTEX_POINT ( 'NONE', #9086 ) ;
#55171 = ORIENTED_EDGE ( 'NONE', *, *, #4839, .T. ) ;
#55172 = PLANE ( 'NONE',  #31903 ) ;
#55173 = DIRECTION ( 'NONE',  ( -0.5364919789714478471, 0.6444004775717705469, -0.5449076811759709926 ) ) ;
#55174 = CARTESIAN_POINT ( 'NONE',  ( -69.20357155325814347, 0.1329212998141634239, 6.404540763468512310 ) ) ;
#55175 = DIRECTION ( 'NONE',  ( 0.9999697198139515519, 0.000000000000000000, 0.007781995580013368816 ) ) ;
#55176 = DIRECTION ( 'NONE',  ( -0.9999697198139514409, -0.000000000000000000, -0.007781995580013368816 ) ) ;
#55177 = CARTESIAN_POINT ( 'NONE',  ( -15.85491555274374065, 0.9340140483890049250, 4.572784929179271707 ) ) ;
#55178 = EDGE_LOOP ( 'NONE', ( #32110, #12788, #20053, #13633 ) ) ;
#55179 = PLANE ( 'NONE',  #7750 ) ;
#55180 = DIRECTION ( 'NONE',  ( -0.05705673239519650636, 0.9983709377222390602, 2.328063060706355175E-16 ) ) ;
#55181 = VERTEX_POINT ( 'NONE', #26684 ) ;
#55182 = FACE_OUTER_BOUND ( 'NONE', #31354, .T. ) ;
#55183 = ORIENTED_EDGE ( 'NONE', *, *, #50432, .T. ) ;
#55184 = DIRECTION ( 'NONE',  ( 0.007781995580012662783, 0.000000000000000000, -0.9999697198139514409 ) ) ;
#55185 = LINE ( 'NONE', #16552, #14281 ) ;
#55186 = EDGE_CURVE ( 'NONE', #40778, #14783, #31530, .T. ) ;
#55187 = DIRECTION ( 'NONE',  ( -0.005002170337468016433, -0.7660444431189770143, 0.6427681459581293666 ) ) ;
#55188 = FACE_OUTER_BOUND ( 'NONE', #31576, .T. ) ;
#55189 = CARTESIAN_POINT ( 'NONE',  ( -67.80365641637717999, 0.1329308371501277952, -3.375551560958620634 ) ) ;
#55190 = VERTEX_POINT ( 'NONE', #17606 ) ;
#55191 = VERTEX_POINT ( 'NONE', #38918 ) ;
#55192 = CARTESIAN_POINT ( 'NONE',  ( -68.65415923196773917, -0.6013102719389076256, 6.097755213354411730 ) ) ;
#55193 = DIRECTION ( 'NONE',  ( 0.000000000000000000, -1.000000000000000000, 0.000000000000000000 ) ) ;
#55194 = LINE ( 'NONE', #42427, #8851 ) ;
#55195 = EDGE_CURVE ( 'NONE', #27480, #48023, #765, .T. ) ;
#55196 = DIRECTION ( 'NONE',  ( 0.000000000000000000, -0.000000000000000000, -1.000000000000000000 ) ) ;
#55197 = AXIS2_PLACEMENT_3D ( 'NONE', #40096, #1185, #9156 ) ;
#55198 = FACE_OUTER_BOUND ( 'NONE', #15142, .T. ) ;
#55199 = CARTESIAN_POINT ( 'NONE',  ( -3.638580343741060652, 5.221061972330257817, -1.805025403446173682 ) ) ;
#55201 = ADVANCED_FACE ( 'NONE', ( #21604 ), #4291, .F. ) ;
#55200 = ORIENTED_EDGE ( 'NONE', *, *, #39985, .T. ) ;
#55202 = DIRECTION ( 'NONE',  ( 0.5364919789714477361, 0.6444004775717706579, 0.5449076811759711036 ) ) ;
#55203 = EDGE_CURVE ( 'NONE', #4092, #51378, #3, .T. ) ;
#55204 = PLANE ( 'NONE',  #15109 ) ;
#55205 = LINE ( 'NONE', #8077, #40547 ) ;
#55206 = VERTEX_POINT ( 'NONE', #1103 ) ;
#55207 = LINE ( 'NONE', #37312, #8432 ) ;
#55208 = EDGE_CURVE ( 'NONE', #47873, #45359, #30936, .T. ) ;
#55209 = DIRECTION ( 'NONE',  ( 0.007781995580012663651, 0.000000000000000000, -0.9999697198139515519 ) ) ;
#55210 = DIRECTION ( 'NONE',  ( 0.9999697198139515519, 0.000000000000000000, 0.007781995580013368816 ) ) ;
#55211 = EDGE_LOOP ( 'NONE', ( #16718, #52571, #4947, #8794 ) ) ;
#55212 = FACE_OUTER_BOUND ( 'NONE', #38140, .T. ) ;
#55213 = ADVANCED_FACE ( 'NONE', ( #578 ), #17908, .F. ) ;
#55214 = ORIENTED_EDGE ( 'NONE', *, *, #45068, .T. ) ;
#55215 = ADVANCED_FACE ( 'NONE', ( #13371 ), #35232, .F. ) ;
#55216 = VERTEX_POINT ( 'NONE', #839 ) ;
#55217 = ORIENTED_EDGE ( 'NONE', *, *, #44030, .F. ) ;
#55218 = ORIENTED_EDGE ( 'NONE', *, *, #48695, .T. ) ;
#55219 = PLANE ( 'NONE',  #31144 ) ;
#55220 = EDGE_LOOP ( 'NONE', ( #27022, #20864, #24595, #13191 ) ) ;
#55221 = CARTESIAN_POINT ( 'NONE',  ( -12.32171488119139546, 23.81227963477840248, -3.519960964911045931 ) ) ;
#55222 = EDGE_CURVE ( 'NONE', #43469, #40926, #35481, .T. ) ;
#55223 = ORIENTED_EDGE ( 'NONE', *, *, #12515, .T. ) ;
#55224 = DIRECTION ( 'NONE',  ( -0.7660212471507179544, -0.6427876096865405842, -0.005961354470445141482 ) ) ;
#55225 = ORIENTED_EDGE ( 'NONE', *, *, #10, .F. ) ;
#55226 = ORIENTED_EDGE ( 'NONE', *, *, #19962, .T. ) ;
#55227 = ADVANCED_FACE ( 'NONE', ( #31224 ), #26985, .F. ) ;
#55228 = LINE ( 'NONE', #15476, #15689 ) ;
#55229 = CARTESIAN_POINT ( 'NONE',  ( -11.82989549392580031, 0.000000000000000000, 6.036346409060238116 ) ) ;
#55230 = CARTESIAN_POINT ( 'NONE',  ( -18.07890891700271041, -2.137015261443157232, 7.211600032455043774 ) ) ;
#55231 = DIRECTION ( 'NONE',  ( -0.7660212471507179544, -0.6427876096865405842, -0.005961354470445141482 ) ) ;
#55232 = ORIENTED_EDGE ( 'NONE', *, *, #7163, .T. ) ;
#55233 = VECTOR ( 'NONE', #41501, 1000.000000000000227 ) ;
#55234 = ORIENTED_EDGE ( 'NONE', *, *, #43473, .T. ) ;
#55235 = CARTESIAN_POINT ( 'NONE',  ( -15.90596353887472070, 0.4483081953215036219, 3.795487648738061104 ) ) ;
#55236 = CARTESIAN_POINT ( 'NONE',  ( -19.28516736416668920, 0.000000000000000000, 7.994314122122347932 ) ) ;
#55237 = DIRECTION ( 'NONE',  ( 0.007781995580012663651, 0.000000000000000000, -0.9999697198139515519 ) ) ;
#55238 = CARTESIAN_POINT ( 'NONE',  ( -58.00000000000000711, -9.999999999999998224, 2.750000000000013323 ) ) ;
#55239 = FACE_OUTER_BOUND ( 'NONE', #51203, .T. ) ;
#55240 = CARTESIAN_POINT ( 'NONE',  ( -9.110551994824897193, -1.000000000000000000, 3.538847790438064411 ) ) ;
#55241 = ORIENTED_EDGE ( 'NONE', *, *, #2718, .T. ) ;
#55242 = DIRECTION ( 'NONE',  ( 0.5364919789714477361, 0.6444004775717706579, 0.5449076811759711036 ) ) ;
#55243 = FACE_OUTER_BOUND ( 'NONE', #31438, .T. ) ;
#55244 = ORIENTED_EDGE ( 'NONE', *, *, #7375, .T. ) ;
#55245 = PLANE ( 'NONE',  #53350 ) ;
#55246 = CARTESIAN_POINT ( 'NONE',  ( -12.17938695170108154, -0.1191753592594188005, 4.086963208580010054 ) ) ;
#55247 = DIRECTION ( 'NONE',  ( -0.7660212471507179544, -0.6427876096865405842, -0.005961354470445141482 ) ) ;
#55248 = EDGE_CURVE ( 'NONE', #2943, #9219, #43190, .T. ) ;
#55249 = CARTESIAN_POINT ( 'NONE',  ( -27.99767448711536133, 0.000000000000000000, 7.557179307314289218 ) ) ;
#55250 = CARTESIAN_POINT ( 'NONE',  ( -16.90534462099871860, -1.327505506330658891, 3.405576699991005984 ) ) ;
#55251 = ORIENTED_EDGE ( 'NONE', *, *, #28545, .T. ) ;
#55252 = ORIENTED_EDGE ( 'NONE', *, *, #21847, .T. ) ;
#55253 = CARTESIAN_POINT ( 'NONE',  ( -29.86197018149027116, 0.000000000000000000, 8.281335066757780083 ) ) ;
#55254 = CARTESIAN_POINT ( 'NONE',  ( -15.55980453706489541, 0.000000000000000000, 7.653973687242195290 ) ) ;
#55255 = FACE_OUTER_BOUND ( 'NONE', #30880, .T. ) ;
#55256 = EDGE_CURVE ( 'NONE', #48949, #11834, #10506, .T. ) ;
#55257 = ADVANCED_FACE ( 'NONE', ( #16080 ), #23548, .F. ) ;
#55258 = DIRECTION ( 'NONE',  ( 0.007781995580012662783, 0.000000000000000000, -0.9999697198139514409 ) ) ;
#55259 = CARTESIAN_POINT ( 'NONE',  ( -6.567513199491930465, 4.309502646206702536, -0.6673284152940708314 ) ) ;
#55260 = LINE ( 'NONE', #29430, #53663 ) ;
#55261 = LINE ( 'NONE', #45916, #38375 ) ;
#55262 = EDGE_CURVE ( 'NONE', #10688, #42394, #5964, .T. ) ;
#55263 = LINE ( 'NONE', #16353, #15065 ) ;
#55264 = FACE_OUTER_BOUND ( 'NONE', #41335, .T. ) ;
#55265 = PLANE ( 'NONE',  #2002 ) ;
#55266 = ORIENTED_EDGE ( 'NONE', *, *, #41909, .F. ) ;
#55267 = LINE ( 'NONE', #16357, #39540 ) ;
#55268 = AXIS2_PLACEMENT_3D ( 'NONE', #28931, #46224, #3067 ) ;
#55269 = ORIENTED_EDGE ( 'NONE', *, *, #34675, .F. ) ;
#55270 = ADVANCED_FACE ( 'NONE', ( #53379 ), #10775, .F. ) ;
#55271 = ORIENTED_EDGE ( 'NONE', *, *, #30236, .F. ) ;
#55272 = EDGE_CURVE ( 'NONE', #21762, #39510, #6242, .T. ) ;
#55273 = EDGE_LOOP ( 'NONE', ( #43509, #23045, #48504, #7596 ) ) ;
#55274 = EDGE_LOOP ( 'NONE', ( #18917, #47312, #2604, #3426 ) ) ;
#55275 = VERTEX_POINT ( 'NONE', #28083 ) ;
#55276 = ORIENTED_EDGE ( 'NONE', *, *, #16957, .F. ) ;
#55277 = CARTESIAN_POINT ( 'NONE',  ( -15.86710544311044302, 0.000000000000000000, 13.13336954653252953 ) ) ;
#55278 = FACE_OUTER_BOUND ( 'NONE', #12122, .T. ) ;
#55279 = CARTESIAN_POINT ( 'NONE',  ( -21.47263955680318404, 0.000000000000000000, 5.022634149262071190 ) ) ;
#55280 = EDGE_CURVE ( 'NONE', #23505, #27112, #40861, .T. ) ;
#55281 = ORIENTED_EDGE ( 'NONE', *, *, #47519, .F. ) ;
#55282 = DIRECTION ( 'NONE',  ( -0.005002170337468016433, -0.7660444431189770143, 0.6427681459581293666 ) ) ;
#55283 = ORIENTED_EDGE ( 'NONE', *, *, #13909, .T. ) ;
#55284 = CARTESIAN_POINT ( 'NONE',  ( -16.81345671998191449, 0.000000000000000000, 3.412238694616132495 ) ) ;
#55285 = ORIENTED_EDGE ( 'NONE', *, *, #53498, .F. ) ;
#55286 = CARTESIAN_POINT ( 'NONE',  ( -65.08541935831070191, -9.158217483546630788, -0.7600040867655236676 ) ) ;
#55287 = DIRECTION ( 'NONE',  ( 0.9999697198139515519, 0.000000000000000000, 0.007781995580013368816 ) ) ;
#55288 = CARTESIAN_POINT ( 'NONE',  ( -69.35946117089058305, -10.06457831932934965, -7.500828395702386686 ) ) ;
#55289 = VERTEX_POINT ( 'NONE', #36607 ) ;
#55290 = DIRECTION ( 'NONE',  ( 0.5449076811759707706, 0.6444004775717708799, -0.5364919789714476250 ) ) ;
#55291 = ORIENTED_EDGE ( 'NONE', *, *, #13316, .F. ) ;
#55292 = DIRECTION ( 'NONE',  ( 0.9999697198139515519, 0.000000000000000000, 0.007781995580013368816 ) ) ;
#55293 = CARTESIAN_POINT ( 'NONE',  ( -17.36532418587302473, -0.1191753592594177458, 13.67570816655714516 ) ) ;
#55294 = DIRECTION ( 'NONE',  ( 0.5364919789714477361, 0.6444004775717706579, 0.5449076811759711036 ) ) ;
#55295 = CARTESIAN_POINT ( 'NONE',  ( -13.27065584551087163, 0.000000000000000000, 12.04557950825129176 ) ) ;
#55296 = CARTESIAN_POINT ( 'NONE',  ( -14.80174839320972779, 0.000000000000000000, 8.967875321077752204 ) ) ;
#55297 = LINE ( 'NONE', #16390, #5848 ) ;
#55298 = DIRECTION ( 'NONE',  ( -0.6427681459581293666, -0.7660444431189770143, -0.005002170337467561935 ) ) ;
#55299 = LINE ( 'NONE', #16392, #26822 ) ;
#55300 = VERTEX_POINT ( 'NONE', #54986 ) ;
#55301 = DIRECTION ( 'NONE',  ( -0.7660212471507179544, -0.6427876096865405842, -0.005961354470445141482 ) ) ;
#55302 = ORIENTED_EDGE ( 'NONE', *, *, #30027, .F. ) ;
#55303 = EDGE_CURVE ( 'NONE', #51521, #56197, #37658, .T. ) ;
#55304 = PLANE ( 'NONE',  #24712 ) ;
#55305 = CARTESIAN_POINT ( 'NONE',  ( -31.72782227498118601, 0.000000000000000000, 9.205484770164058972 ) ) ;
#55306 = CARTESIAN_POINT ( 'NONE',  ( -18.19747506107908563, 0.000000000000000000, 14.03856424583689311 ) ) ;
#55307 = EDGE_CURVE ( 'NONE', #6779, #28682, #11798, .T. ) ;
#55308 = CARTESIAN_POINT ( 'NONE',  ( -18.50873683370415179, -1.003701604285656579, 5.518599004666138619 ) ) ;
#55309 = CARTESIAN_POINT ( 'NONE',  ( -8.609916609573598834, 0.000000000000000000, 10.23519010964256637 ) ) ;
#55310 = CARTESIAN_POINT ( 'NONE',  ( -22.40634380310664397, 0.000000000000000000, 5.584705972946605534 ) ) ;
#55311 = APPLICATION_PROTOCOL_DEFINITION ( 'draft international standard', 'automotive_design', 1998, #17331 ) ;
#55312 = EDGE_LOOP ( 'NONE', ( #46910, #27275, #34553, #40628 ) ) ;
#55313 = ADVANCED_FACE ( 'NONE', ( #29119 ), #23284, .F. ) ;
#55314 = DIRECTION ( 'NONE',  ( -0.005002170337468016433, -0.7660444431189770143, 0.6427681459581293666 ) ) ;
#55315 = CARTESIAN_POINT ( 'NONE',  ( -11.13054826722768098, 24.50000000000005684, 3.000000000000000444 ) ) ;
#55316 = PLANE ( 'NONE',  #44888 ) ;
#55317 = LINE ( 'NONE', #21245, #39094 ) ;
#55318 = ADVANCED_FACE ( 'NONE', ( #1401 ), #46425, .F. ) ;
#55319 = EDGE_CURVE ( 'NONE', #34341, #29949, #45390, .T. ) ;
#55320 = ADVANCED_FACE ( 'NONE', ( #20628 ), #55245, .F. ) ;
#55321 = CARTESIAN_POINT ( 'NONE',  ( -18.61669932361099455, 0.000000000000000000, 8.199522351202686465 ) ) ;
#55322 = CARTESIAN_POINT ( 'NONE',  ( -56.00000000000000711, 6.050000000000001599, -2.749999999999994671 ) ) ;
#55323 = EDGE_CURVE ( 'NONE', #41560, #12727, #33658, .T. ) ;
#55324 = LINE ( 'NONE', #16417, #25918 ) ;
#55325 = PLANE ( 'NONE',  #43757 ) ;
#55326 = ORIENTED_EDGE ( 'NONE', *, *, #51920, .F. ) ;
#55327 = LINE ( 'NONE', #33219, #55735 ) ;
#55328 = FACE_OUTER_BOUND ( 'NONE', #6090, .T. ) ;
#55329 = ORIENTED_EDGE ( 'NONE', *, *, #24121, .T. ) ;
#55330 = ORIENTED_EDGE ( 'NONE', *, *, #8653, .F. ) ;
#55331 = DIRECTION ( 'NONE',  ( -2.683102249366423030E-17, 4.694855797473116505E-16, -1.000000000000000000 ) ) ;
#55332 = ORIENTED_EDGE ( 'NONE', *, *, #5673, .T. ) ;
#55333 = ADVANCED_FACE ( 'NONE', ( #40308 ), #41889, .T. ) ;
#55334 = ORIENTED_EDGE ( 'NONE', *, *, #48874, .T. ) ;
#55335 = LINE ( 'NONE', #7352, #46503 ) ;
#55336 = AXIS2_PLACEMENT_3D ( 'NONE', #9599, #18675, #36018 ) ;
#55337 = EDGE_CURVE ( 'NONE', #17834, #43208, #31790, .T. ) ;
#55338 = ORIENTED_EDGE ( 'NONE', *, *, #36943, .T. ) ;
#55339 = ORIENTED_EDGE ( 'NONE', *, *, #37233, .T. ) ;
#55340 = VERTEX_POINT ( 'NONE', #14742 ) ;
#55341 = ADVANCED_FACE ( 'NONE', ( #49387 ), #55818, .F. ) ;
#55342 = DIRECTION ( 'NONE',  ( 0.005002170337468016433, -0.7660444431189770143, -0.6427681459581293666 ) ) ;
#55343 = CARTESIAN_POINT ( 'NONE',  ( -65.44640951980584020, -9.199613742922251092, -3.251835480715623117 ) ) ;
#55344 = CARTESIAN_POINT ( 'NONE',  ( -13.27065584551087163, 0.000000000000000000, 12.04557950825129176 ) ) ;
#55345 = EDGE_CURVE ( 'NONE', #41612, #5753, #52109, .T. ) ;
#55346 = ORIENTED_EDGE ( 'NONE', *, *, #8270, .T. ) ;
#55347 = ORIENTED_EDGE ( 'NONE', *, *, #3228, .T. ) ;
#55348 = EDGE_CURVE ( 'NONE', #52427, #36412, #50970, .T. ) ;
#55349 = CARTESIAN_POINT ( 'NONE',  ( -17.36532418587302473, -0.1191753592594177458, 13.67570816655714516 ) ) ;
#55350 = PLANE ( 'NONE',  #56 ) ;
#55351 = ORIENTED_EDGE ( 'NONE', *, *, #37182, .F. ) ;
#55352 = DIRECTION ( 'NONE',  ( 0.007781995580012662783, 0.000000000000000000, -0.9999697198139514409 ) ) ;
#55353 = CARTESIAN_POINT ( 'NONE',  ( -19.61547266693814251, -2.298917212465658277, 8.074162258805023029 ) ) ;
#55354 = ORIENTED_EDGE ( 'NONE', *, *, #44899, .F. ) ;
#55355 = FACE_OUTER_BOUND ( 'NONE', #45638, .T. ) ;
#55356 = PLANE ( 'NONE',  #34892 ) ;
#55357 = ORIENTED_EDGE ( 'NONE', *, *, #23093, .F. ) ;
#55358 = FACE_OUTER_BOUND ( 'NONE', #18935, .T. ) ;
#55359 = DIRECTION ( 'NONE',  ( 0.7660212471507180654, -0.6427876096865404731, 0.005961354470445141482 ) ) ;
#55360 = ORIENTED_EDGE ( 'NONE', *, *, #31750, .T. ) ;
#55361 = CARTESIAN_POINT ( 'NONE',  ( -17.40685591040811175, 0.000000000000000000, 6.162271227139100027 ) ) ;
#55362 = DIRECTION ( 'NONE',  ( -0.3620778797217455991, 0.000000000000000000, -0.9321478471874540261 ) ) ;
#55363 = CARTESIAN_POINT ( 'NONE',  ( -11.68519433167736743, -3.432230869623161595, 1.310741292032489236 ) ) ;
#55364 = CARTESIAN_POINT ( 'NONE',  ( -15.80875956802750260, 0.000000000000000000, 5.636049899006391861 ) ) ;
#55365 = ORIENTED_EDGE ( 'NONE', *, *, #2818, .T. ) ;
#55366 = VECTOR ( 'NONE', #42860, 1000.000000000000227 ) ;
#55367 = DIRECTION ( 'NONE',  ( 0.9999697198139515519, 0.000000000000000000, 0.007781995580013368816 ) ) ;
#55368 = CARTESIAN_POINT ( 'NONE',  ( -17.31082735807079587, 4.819660872929009798, 11.51531893215243230 ) ) ;
#55369 = DIRECTION ( 'NONE',  ( 0.007781995580012662783, 0.000000000000000000, -0.9999697198139514409 ) ) ;
#55370 = LINE ( 'NONE', #46877, #3225 ) ;
#55371 = CARTESIAN_POINT ( 'NONE',  ( -12.13851405436063047, 0.000000000000000000, 11.68505802764555135 ) ) ;
#55372 = DIRECTION ( 'NONE',  ( -0.2426528472758542054, 0.7422098413412800966, -0.6246952433987894571 ) ) ;
#55373 = AXIS2_PLACEMENT_3D ( 'NONE', #16214, #21016, #8538 ) ;
#55374 = CARTESIAN_POINT ( 'NONE',  ( -12.99638935982272514, 0.000000000000000000, 2.503273799589543991 ) ) ;
#55375 = VERTEX_POINT ( 'NONE', #47867 ) ;
#55376 = DIRECTION ( 'NONE',  ( 0.005961354470445682716, -0.6427876096865404731, -0.7660212471507180654 ) ) ;
#55377 = FACE_OUTER_BOUND ( 'NONE', #29373, .T. ) ;
#55378 = ORIENTED_EDGE ( 'NONE', *, *, #31181, .T. ) ;
#55379 = PLANE ( 'NONE',  #22946 ) ;
#55380 = DIRECTION ( 'NONE',  ( 0.000000000000000000, -1.000000000000000000, 0.000000000000000000 ) ) ;
#55381 = EDGE_CURVE ( 'NONE', #40111, #21762, #3569, .T. ) ;
#55382 = EDGE_CURVE ( 'NONE', #1435, #47262, #4146, .T. ) ;
#55383 = CARTESIAN_POINT ( 'NONE',  ( -19.60912206198629804, -0.1191753592594194527, 4.398475361799976113 ) ) ;
#55384 = ADVANCED_FACE ( 'NONE', ( #30560 ), #17461, .F. ) ;
#55385 = CARTESIAN_POINT ( 'NONE',  ( -16.81345671998191449, 0.000000000000000000, 3.412238694616132495 ) ) ;
#55386 = DIRECTION ( 'NONE',  ( 0.005002170337468016433, -0.7660444431189770143, -0.6427681459581293666 ) ) ;
#55387 = ORIENTED_EDGE ( 'NONE', *, *, #45827, .T. ) ;
#55388 = ORIENTED_EDGE ( 'NONE', *, *, #4134, .T. ) ;
#55389 = SHAPE_REPRESENTATION ( 'Swivel Catch Post', ( #2610 ), #38910 ) ;
#55390 = LINE ( 'NONE', #20764, #11406 ) ;
#55391 = DIRECTION ( 'NONE',  ( -0.005002170337468016433, -0.7660444431189770143, 0.6427681459581293666 ) ) ;
#55392 = ORIENTED_EDGE ( 'NONE', *, *, #29292, .T. ) ;
#55393 = DIRECTION ( 'NONE',  ( 0.3583679495452941066, 0.9335804264972041855, -0.000000000000000000 ) ) ;
#55394 = VECTOR ( 'NONE', #49713, 999.9999999999998863 ) ;
#55395 = ORIENTED_EDGE ( 'NONE', *, *, #16253, .T. ) ;
#55396 = CARTESIAN_POINT ( 'NONE',  ( -16.33317936670417225, 0.000000000000000000, 13.31440848639340224 ) ) ;
#55397 = ORIENTED_EDGE ( 'NONE', *, *, #15443, .F. ) ;
#55398 = CARTESIAN_POINT ( 'NONE',  ( -16.83150402712250227, -0.1191753592594197719, 4.789423497415446818 ) ) ;
#55399 = EDGE_LOOP ( 'NONE', ( #5002, #24846, #43907, #46136 ) ) ;
#55400 = ORIENTED_EDGE ( 'NONE', *, *, #42331, .T. ) ;
#55401 = EDGE_LOOP ( 'NONE', ( #38957, #39583, #27639, #7432 ) ) ;
#55402 = DIRECTION ( 'NONE',  ( 0.000000000000000000, 1.000000000000000000, 0.000000000000000000 ) ) ;
#55403 = CARTESIAN_POINT ( 'NONE',  ( -8.840523769800496368, 0.000000000000000000, 5.859604334821510108 ) ) ;
#55404 = CARTESIAN_POINT ( 'NONE',  ( -9.280526530289439080, -2.201020558340975430, 3.101258514253283138 ) ) ;
#55406 = CARTESIAN_POINT ( 'NONE',  ( -2.276746449950904694, -3.901742918183043418, -2.334007935867973949 ) ) ;
#55405 = AXIS2_PLACEMENT_3D ( 'NONE', #48229, #35464, #53078 ) ;
#55407 = ORIENTED_EDGE ( 'NONE', *, *, #26353, .T. ) ;
#55408 = ADVANCED_FACE ( 'NONE', ( #39335 ), #38489, .F. ) ;
#55409 = VECTOR ( 'NONE', #40814, 1000.000000000000114 ) ;
#55410 = ORIENTED_EDGE ( 'NONE', *, *, #46940, .F. ) ;
#55411 = VERTEX_POINT ( 'NONE', #12658 ) ;
#55412 = LINE ( 'NONE', #21355, #53985 ) ;
#55413 = ADVANCED_FACE ( 'NONE', ( #42481 ), #26019, .F. ) ;
#55414 = CARTESIAN_POINT ( 'NONE',  ( -15.88053067323646417, -0.1191753592594197858, 2.950163842912994383 ) ) ;
#55415 = VERTEX_POINT ( 'NONE', #29974 ) ;
#55416 = DIRECTION ( 'NONE',  ( -0.005002170337468016433, -0.7660444431189770143, 0.6427681459581293666 ) ) ;
#55417 = ADVANCED_FACE ( 'NONE', ( #8968 ), #4688, .F. ) ;
#55418 = ORIENTED_EDGE ( 'NONE', *, *, #42389, .T. ) ;
#55419 = DIRECTION ( 'NONE',  ( -0.005961354470445682716, -0.6427876096865404731, 0.7660212471507180654 ) ) ;
#55420 = PLANE ( 'NONE',  #45723 ) ;
#55421 = ORIENTED_EDGE ( 'NONE', *, *, #33192, .F. ) ;
#55422 = EDGE_CURVE ( 'NONE', #42447, #48276, #56105, .T. ) ;
#55423 = DIRECTION ( 'NONE',  ( 0.000000000000000000, 0.000000000000000000, -1.000000000000000000 ) ) ;
#55424 = ORIENTED_EDGE ( 'NONE', *, *, #18890, .F. ) ;
#55425 = FACE_OUTER_BOUND ( 'NONE', #9555, .T. ) ;
#55426 = LINE ( 'NONE', #11982, #26610 ) ;
#55427 = ORIENTED_EDGE ( 'NONE', *, *, #28059, .F. ) ;
#55428 = DIRECTION ( 'NONE',  ( -0.3620778797217456546, 0.000000000000000000, -0.9321478471874540261 ) ) ;
#55429 = LINE ( 'NONE', #48039, #24796 ) ;
#55430 = FACE_OUTER_BOUND ( 'NONE', #30495, .T. ) ;
#55431 = CARTESIAN_POINT ( 'NONE',  ( -20.09291730366250306, -0.1191753592594199662, 5.914810210573124394 ) ) ;
#55432 = ORIENTED_EDGE ( 'NONE', *, *, #7298, .T. ) ;
#55433 = AXIS2_PLACEMENT_3D ( 'NONE', #33476, #38015, #42817 ) ;
#55434 = ORIENTED_EDGE ( 'NONE', *, *, #41735, .F. ) ;
#55435 = VECTOR ( 'NONE', #47123, 999.9999999999998863 ) ;
#55436 = CARTESIAN_POINT ( 'NONE',  ( -12.80458192191714595, 0.000000000000000000, 11.86454056839041726 ) ) ;
#55437 = FACE_OUTER_BOUND ( 'NONE', #19011, .T. ) ;
#55438 = DIRECTION ( 'NONE',  ( 0.9999697198139515519, 0.000000000000000000, 0.007781995580013368816 ) ) ;
#55439 = CARTESIAN_POINT ( 'NONE',  ( -14.42634509152537348, 0.000000000000000000, 7.124136447341477663 ) ) ;
#55440 = FACE_OUTER_BOUND ( 'NONE', #4684, .T. ) ;
#55441 = CARTESIAN_POINT ( 'NONE',  ( -17.93139508144814442, 0.000000000000000000, 13.85596890686001537 ) ) ;
#55442 = ORIENTED_EDGE ( 'NONE', *, *, #54314, .T. ) ;
#55443 = CARTESIAN_POINT ( 'NONE',  ( -18.67619601524082285, 0.000000000000000000, 3.936400510096834893 ) ) ;
#55444 = CARTESIAN_POINT ( 'NONE',  ( -17.73140113748535285, 0.000000000000000000, 13.85752530597602039 ) ) ;
#55445 = ORIENTED_EDGE ( 'NONE', *, *, #33272, .F. ) ;
#55446 = DIRECTION ( 'NONE',  ( 0.2426528472758541499, 0.7422098413412800966, 0.6246952433987894571 ) ) ;
#55447 = ORIENTED_EDGE ( 'NONE', *, *, #3039, .T. ) ;
#55448 = EDGE_CURVE ( 'NONE', #23248, #5370, #21738, .T. ) ;
#55449 = PLANE ( 'NONE',  #24344 ) ;
#55451 = CARTESIAN_POINT ( 'NONE',  ( -13.63673279712320507, -0.1191753592594197858, 12.22739664767016521 ) ) ;
#55450 = B_SPLINE_CURVE_WITH_KNOTS ( 'NONE', 3,
 ( #47585, #8706, #132, #49256 ),
 .UNSPECIFIED., .F., .F.,
 ( 4, 4 ),
 ( 0.3121479134361153651, 0.3384768704940201989 ),
 .UNSPECIFIED. ) ;
#55452 = LINE ( 'NONE', #42121, #9623 ) ;
#55453 = ADVANCED_FACE ( 'NONE', ( #12077 ), #47574, .F. ) ;
#55454 = EDGE_CURVE ( 'NONE', #34450, #36925, #43035, .T. ) ;
#55455 = DIRECTION ( 'NONE',  ( -0.5364919789714478471, 0.6444004775717705469, -0.5449076811759709926 ) ) ;
#55456 = AXIS2_PLACEMENT_3D ( 'NONE', #14790, #39529, #620 ) ;
#55457 = CARTESIAN_POINT ( 'NONE',  ( -69.84500490485720547, 0.1331119800031512479, -7.306024462449258294 ) ) ;
#55458 = VERTEX_POINT ( 'NONE', #17191 ) ;
#55459 = ORIENTED_EDGE ( 'NONE', *, *, #31929, .T. ) ;
#55460 = CARTESIAN_POINT ( 'NONE',  ( -14.94838282604900748, -0.1191753592594197858, 2.588085963191248506 ) ) ;
#55461 = CARTESIAN_POINT ( 'NONE',  ( -14.01701317841955508, 0.000000000000000000, 2.326005055450897085 ) ) ;
#55462 = LINE ( 'NONE', #20264, #37857 ) ;
#55463 = CARTESIAN_POINT ( 'NONE',  ( 4.452747148193316740, -1.000000000000000000, 0.4159841754879232689 ) ) ;
#55464 = LINE ( 'NONE', #21417, #4740 ) ;
#55465 = DIRECTION ( 'NONE',  ( 0.000000000000000000, 0.000000000000000000, -1.000000000000000000 ) ) ;
#55466 = ORIENTED_EDGE ( 'NONE', *, *, #28986, .F. ) ;
#55467 = CARTESIAN_POINT ( 'NONE',  ( -18.86354292863559579, 0.000000000000000000, 14.21804678658176080 ) ) ;
#55468 = EDGE_CURVE ( 'NONE', #49012, #41524, #16624, .T. ) ;
#55469 = DIRECTION ( 'NONE',  ( 0.007781995580012662783, 0.000000000000000000, -0.9999697198139514409 ) ) ;
#55470 = CARTESIAN_POINT ( 'NONE',  ( -18.67697421479882181, -0.1191753592594197858, 4.036397482078229793 ) ) ;
#55471 = ORIENTED_EDGE ( 'NONE', *, *, #38815, .T. ) ;
#55472 = DIRECTION ( 'NONE',  ( -0.6427681459581293666, -0.7660444431189770143, -0.005002170337467561935 ) ) ;
#55473 = LINE ( 'NONE', #16297, #26798 ) ;
#55474 = LINE ( 'NONE', #51231, #44741 ) ;
#55475 = ORIENTED_EDGE ( 'NONE', *, *, #29274, .T. ) ;
#55476 = VECTOR ( 'NONE', #137, 999.9999999999998863 ) ;
#55477 = AXIS2_PLACEMENT_3D ( 'NONE', #15416, #18870, #11153 ) ;
#55478 = LINE ( 'NONE', #38754, #12174 ) ;
#55479 = VERTEX_POINT ( 'NONE', #30259 ) ;
#55480 = EDGE_LOOP ( 'NONE', ( #32490, #49227, #22027, #33423 ) ) ;
#55481 = VERTEX_POINT ( 'NONE', #8123 ) ;
#55482 = VECTOR ( 'NONE', #27365, 999.9999999999998863 ) ;
#55483 = ORIENTED_EDGE ( 'NONE', *, *, #14142, .T. ) ;
#55484 = DIRECTION ( 'NONE',  ( 0.007781995580012663651, -3.146120232559066537E-19, -0.9999697198139514409 ) ) ;
#55485 = EDGE_LOOP ( 'NONE', ( #49352, #53133, #30735, #39141 ) ) ;
#55486 = CARTESIAN_POINT ( 'NONE',  ( -18.29747203306047609, -0.1191753592594177458, 14.03778604627889059 ) ) ;
#55487 = ORIENTED_EDGE ( 'NONE', *, *, #3914, .F. ) ;
#55488 = CARTESIAN_POINT ( 'NONE',  ( -11.20636620717317378, 0.000000000000000000, 11.32298014792380414 ) ) ;
#55489 = EDGE_CURVE ( 'NONE', #54036, #2726, #25427, .T. ) ;
#55490 = VERTEX_POINT ( 'NONE', #4429 ) ;
#55491 = AXIS2_PLACEMENT_3D ( 'NONE', #10416, #49020, #23474 ) ;
#55492 = ORIENTED_EDGE ( 'NONE', *, *, #25017, .F. ) ;
#55493 = AXIS2_PLACEMENT_3D ( 'NONE', #40715, #10636, #27656 ) ;
#55494 = LINE ( 'NONE', #12907, #39300 ) ;
#55495 = LINE ( 'NONE', #13201, #35929 ) ;
#55496 = CARTESIAN_POINT ( 'NONE',  ( -17.68874318431810266, 0.000000000000000000, 8.376069934033679942 ) ) ;
#55497 = CARTESIAN_POINT ( 'NONE',  ( -20.71696439550653324, 1.743523803501507485, 4.673476716096989669 ) ) ;
#55498 = PLANE ( 'NONE',  #35604 ) ;
#55499 = ORIENTED_EDGE ( 'NONE', *, *, #6299, .F. ) ;
#55500 = ADVANCED_FACE ( 'NONE', ( #39051 ), #27379, .F. ) ;
#55501 = VERTEX_POINT ( 'NONE', #35357 ) ;
#55502 = LINE ( 'NONE', #41356, #31299 ) ;
#55503 = CARTESIAN_POINT ( 'NONE',  ( -24.27063949748155380, 0.000000000000000000, 6.308861732390097288 ) ) ;
#55504 = EDGE_CURVE ( 'NONE', #43608, #3029, #38662, .T. ) ;
#55505 = EDGE_CURVE ( 'NONE', #53403, #43303, #9223, .T. ) ;
#55506 = DIRECTION ( 'NONE',  ( -0.6427681459581293666, -0.7660444431189770143, -0.005002170337467561935 ) ) ;
#55507 = DIRECTION ( 'NONE',  ( 0.6427681459581294776, -0.7660444431189769032, 0.005002170337467562802 ) ) ;
#55508 = DIRECTION ( 'NONE',  ( 0.005002170337468016433, -0.7660444431189770143, -0.6427681459581293666 ) ) ;
#55509 = DIRECTION ( 'NONE',  ( 0.005002170337468016433, -0.7660444431189770143, -0.6427681459581293666 ) ) ;
#55510 = ORIENTED_EDGE ( 'NONE', *, *, #31174, .T. ) ;
#55512 = LINE ( 'NONE', #30256, #2037 ) ;
#55511 = VECTOR ( 'NONE', #20694, 1000.000000000000227 ) ;
#55513 = EDGE_CURVE ( 'NONE', #35388, #21352, #40165, .T. ) ;
#55514 = CARTESIAN_POINT ( 'NONE',  ( 5.454418722303246092, 0.000000000000000000, -2.500028562687453437 ) ) ;
#55515 = VERTEX_POINT ( 'NONE', #18294 ) ;
#55516 = VECTOR ( 'NONE', #25380, 999.9999999999998863 ) ;
#55517 = VECTOR ( 'NONE', #36595, 999.9999999999998863 ) ;
#55518 = CARTESIAN_POINT ( 'NONE',  ( -49.27554558092695913, 2.476975532698160620, 5.000000000000000000 ) ) ;
#55519 = CARTESIAN_POINT ( 'NONE',  ( -17.78377024884693469, -0.1191753592594177180, 7.736669299941538291 ) ) ;
#55520 = EDGE_CURVE ( 'NONE', #29513, #27257, #35634, .T. ) ;
#55521 = DIRECTION ( 'NONE',  ( 0.6427681459581294776, -0.7660444431189769032, 0.005002170337467562802 ) ) ;
#55522 = DIRECTION ( 'NONE',  ( 0.9999697198139515519, 0.000000000000000000, 0.007781995580013368816 ) ) ;
#55523 = ADVANCED_FACE ( 'NONE', ( #39637 ), #27680, .F. ) ;
#55524 = DIRECTION ( 'NONE',  ( -0.005002170337468016433, -0.7660444431189770143, 0.6427681459581293666 ) ) ;
#55525 = EDGE_LOOP ( 'NONE', ( #25264, #10851, #14639, #53232, #23633 ) ) ;
#55526 = VECTOR ( 'NONE', #48200, 1000.000000000000227 ) ;
#55527 = VECTOR ( 'NONE', #6559, 1000.000000000000227 ) ;
#55528 = ORIENTED_EDGE ( 'NONE', *, *, #42920, .F. ) ;
#55529 = DIRECTION ( 'NONE',  ( 0.9999697198139515519, 0.000000000000000000, 0.007781995580013368816 ) ) ;
#55530 = CARTESIAN_POINT ( 'NONE',  ( -20.42824791815107943, 20.86402141126400167, 4.315470560068479955 ) ) ;
#55531 = LINE ( 'NONE', #47030, #31544 ) ;
#55532 = EDGE_CURVE ( 'NONE', #16370, #42656, #715, .T. ) ;
#55533 = DIRECTION ( 'NONE',  ( 0.000000000000000000, -0.000000000000000000, -1.000000000000000000 ) ) ;
#55534 = VECTOR ( 'NONE', #19399, 999.9999999999998863 ) ;
#55535 = LINE ( 'NONE', #3005, #14925 ) ;
#55536 = CARTESIAN_POINT ( 'NONE',  ( -15.78995884787980053, 0.000000000000000000, 3.220197735497015934 ) ) ;
#55537 = DIRECTION ( 'NONE',  ( -0.005961354470445682716, -0.6427876096865404731, 0.7660212471507180654 ) ) ;
#55538 = EDGE_CURVE ( 'NONE', #8731, #16665, #52403, .T. ) ;
#55539 = DIRECTION ( 'NONE',  ( -0.9999697198139514409, -0.000000000000000000, -0.007781995580013368816 ) ) ;
#55540 = CARTESIAN_POINT ( 'NONE',  ( -66.80814951898862830, -9.355770193211530028, -5.009371237985869918 ) ) ;
#55541 = CARTESIAN_POINT ( 'NONE',  ( -18.75513958955402316, -4.079838673713163111, 4.036286046993806664 ) ) ;
#55542 = VERTEX_POINT ( 'NONE', #14059 ) ;
#55543 = DIRECTION ( 'NONE',  ( -0.3620778797217457101, 0.000000000000000000, -0.9321478471874540261 ) ) ;
#55544 = ORIENTED_EDGE ( 'NONE', *, *, #4885, .T. ) ;
#55545 = AXIS2_PLACEMENT_3D ( 'NONE', #44706, #35638, #39896 ) ;
#55546 = VERTEX_POINT ( 'NONE', #31390 ) ;
#55547 = VERTEX_POINT ( 'NONE', #48710 ) ;
#55548 = VERTEX_POINT ( 'NONE', #10066 ) ;
#55549 = EDGE_LOOP ( 'NONE', ( #48705, #32788, #3599, #39563 ) ) ;
#55550 = ORIENTED_EDGE ( 'NONE', *, *, #33559, .T. ) ;
#55551 = VECTOR ( 'NONE', #12612, 999.9999999999998863 ) ;
#55552 = LINE ( 'NONE', #24906, #25111 ) ;
#55553 = CARTESIAN_POINT ( 'NONE',  ( -16.50213094388420387, 0.000000000000000000, 9.323974620700020921 ) ) ;
#55554 = CARTESIAN_POINT ( 'NONE',  ( -68.90818038468613338, -0.2025580785338727541, 7.478321023991167493 ) ) ;
#55555 = VECTOR ( 'NONE', #20409, 1000.000000000000114 ) ;
#55556 = VECTOR ( 'NONE', #55242, 999.9999999999998863 ) ;
#55557 = ORIENTED_EDGE ( 'NONE', *, *, #19818, .T. ) ;
#55558 = CARTESIAN_POINT ( 'NONE',  ( -14.87171971942530568, 1.419719901456505395, 4.988004329898734213 ) ) ;
#55559 = ADVANCED_FACE ( 'NONE', ( #9813 ), #13502, .F. ) ;
#55560 = VERTEX_POINT ( 'NONE', #18035 ) ;
#55561 = CARTESIAN_POINT ( 'NONE',  ( -66.39287224736634130, -11.32125582591041280, 6.891331229949073212 ) ) ;
#55562 = ORIENTED_EDGE ( 'NONE', *, *, #998, .T. ) ;
#55563 = AXIS2_PLACEMENT_3D ( 'NONE', #51839, #18057, #35377 ) ;
#55564 = AXIS2_PLACEMENT_3D ( 'NONE', #33722, #29780, #47077 ) ;
#55565 = CARTESIAN_POINT ( 'NONE',  ( -17.89029352739689926, 0.000000000000000000, 8.574507478880466493 ) ) ;
#55566 = DIRECTION ( 'NONE',  ( -0.7660212471507179544, -0.6427876096865405842, -0.005961354470445141482 ) ) ;
#55567 = FACE_OUTER_BOUND ( 'NONE', #29018, .T. ) ;
#55568 = VERTEX_POINT ( 'NONE', #6375 ) ;
#55569 = CARTESIAN_POINT ( 'NONE',  ( -15.09735569160282154, 2.229229656569007290, 6.404192423874666140 ) ) ;
#55570 = ORIENTED_EDGE ( 'NONE', *, *, #53041, .F. ) ;
#55571 = DIRECTION ( 'NONE',  ( 0.000000000000000000, -1.000000000000000000, 0.000000000000000000 ) ) ;
#55572 = AXIS2_PLACEMENT_3D ( 'NONE', #12772, #7975, #32731 ) ;
#55573 = CARTESIAN_POINT ( 'NONE',  ( -17.30371862263972815, 4.333955019861511992, 3.265007825402915120 ) ) ;
#55574 = AXIS2_PLACEMENT_3D ( 'NONE', #466, #17808, #48152 ) ;
#55575 = EDGE_CURVE ( 'NONE', #38023, #26804, #50061, .T. ) ;
#55576 = PLANE ( 'NONE',  #28743 ) ;
#55577 = LINE ( 'NONE', #16686, #27682 ) ;
#55578 = PLANE ( 'NONE',  #28374 ) ;
#55579 = DIRECTION ( 'NONE',  ( 0.9999697198139515519, 0.000000000000000000, 0.007781995580013368816 ) ) ;
#55580 = DIRECTION ( 'NONE',  ( 0.9999697198139515519, 0.000000000000000000, 0.007781995580013368816 ) ) ;
#55581 = CARTESIAN_POINT ( 'NONE',  ( -70.26988861484534254, -8.746188756442855095, 8.208045577613539479 ) ) ;
#55582 = VERTEX_POINT ( 'NONE', #2647 ) ;
#55583 = CARTESIAN_POINT ( 'NONE',  ( -56.04969639603970677, 6.801751789163780870, -1.941170806325171139 ) ) ;
#55584 = ORIENTED_EDGE ( 'NONE', *, *, #11163, .F. ) ;
#55585 = VECTOR ( 'NONE', #29319, 1000.000000000000227 ) ;
#55586 = CARTESIAN_POINT ( 'NONE',  ( -7.094024697029445825, 2.107956770024262294, 8.730276719704061605 ) ) ;
#55587 = CARTESIAN_POINT ( 'NONE',  ( -15.88130887279446490, 0.000000000000000000, 3.050160814894388839 ) ) ;
#55588 = ADVANCED_FACE ( 'NONE', ( #19715 ), #15709, .F. ) ;
#55589 = CARTESIAN_POINT ( 'NONE',  ( -18.67775241435682432, 0.000000000000000000, 4.136394454059623804 ) ) ;
#55590 = VECTOR ( 'NONE', #47148, 1000.000000000000000 ) ;
#55591 = LINE ( 'NONE', #55308, #43961 ) ;
#55592 = DIRECTION ( 'NONE',  ( -0.5449076811759708816, 0.6444004775717707689, 0.5364919789714475140 ) ) ;
#55593 = EDGE_CURVE ( 'NONE', #23151, #47316, #49545, .T. ) ;
#55594 = DIRECTION ( 'NONE',  ( 0.000000000000000000, -0.000000000000000000, -1.000000000000000000 ) ) ;
#55595 = ORIENTED_EDGE ( 'NONE', *, *, #9959, .F. ) ;
#55596 = VECTOR ( 'NONE', #30131, 1000.000000000000227 ) ;
#55597 = LINE ( 'NONE', #8778, #5768 ) ;
#55598 = PLANE ( 'NONE',  #54846 ) ;
#55599 = CARTESIAN_POINT ( 'NONE',  ( -12.94718852056742975, -3.270328918600661883, 1.806108212387832923 ) ) ;
#55600 = VECTOR ( 'NONE', #14080, 999.9999999999998863 ) ;
#55601 = EDGE_CURVE ( 'NONE', #36400, #33244, #36760, .T. ) ;
#55602 = VECTOR ( 'NONE', #2380, 1000.000000000000227 ) ;
#55603 = DIRECTION ( 'NONE',  ( 0.7660212471507180654, -0.6427876096865404731, 0.005961354470445141482 ) ) ;
#55604 = CARTESIAN_POINT ( 'NONE',  ( -27.06708303904391144, 0.000000000000000000, 7.395095371555332697 ) ) ;
#55605 = LINE ( 'NONE', #47667, #3243 ) ;
#55606 = DIRECTION ( 'NONE',  ( 0.000000000000000000, -1.000000000000000000, 0.000000000000000000 ) ) ;
#55607 = ORIENTED_EDGE ( 'NONE', *, *, #45337, .T. ) ;
#55608 = EDGE_CURVE ( 'NONE', #28729, #24227, #54078, .T. ) ;
#55609 = VECTOR ( 'NONE', #24402, 1000.000000000000000 ) ;
#55610 = CARTESIAN_POINT ( 'NONE',  ( -14.10890107943635385, -1.327505506330656670, 2.319343060825770131 ) ) ;
#55611 = AXIS2_PLACEMENT_3D ( 'NONE', #1482, #6043, #905 ) ;
#55612 = LINE ( 'NONE', #33745, #30531 ) ;
#55613 = ORIENTED_EDGE ( 'NONE', *, *, #28869, .T. ) ;
#55614 = ORIENTED_EDGE ( 'NONE', *, *, #48409, .T. ) ;
#55615 = DIRECTION ( 'NONE',  ( 0.000000000000000000, 1.000000000000000000, 0.000000000000000000 ) ) ;
#55616 = ORIENTED_EDGE ( 'NONE', *, *, #42055, .T. ) ;
#55617 = VECTOR ( 'NONE', #55484, 1000.000000000000227 ) ;
#55618 = ORIENTED_EDGE ( 'NONE', *, *, #18334, .F. ) ;
#55619 = ORIENTED_EDGE ( 'NONE', *, *, #22966, .F. ) ;
#55620 = EDGE_LOOP ( 'NONE', ( #3325, #31288, #36788, #26058 ) ) ;
#55621 = CARTESIAN_POINT ( 'NONE',  ( 4.597055792761644888, -1.167435121648761065, 2.076476591771610369 ) ) ;
#55622 = CARTESIAN_POINT ( 'NONE',  ( -65.81766060794319628, -9.242186665891644282, -4.508581566067809909 ) ) ;
#55623 = DIRECTION ( 'NONE',  ( -0.005961354470445682716, -0.6427876096865404731, 0.7660212471507180654 ) ) ;
#55624 = AXIS2_PLACEMENT_3D ( 'NONE', #13815, #19480, #27169 ) ;
#55625 = VERTEX_POINT ( 'NONE', #15188 ) ;
#55627 = ORIENTED_EDGE ( 'NONE', *, *, #8032, .F. ) ;
#55626 = ADVANCED_FACE ( 'NONE', ( #37037 ), #28500, .F. ) ;
#55628 = VECTOR ( 'NONE', #20493, 1000.000000000000227 ) ;
#55629 = ADVANCED_FACE ( 'NONE', ( #37582 ), #54908, .F. ) ;
#55630 = DIRECTION ( 'NONE',  ( 0.000000000000000000, 0.000000000000000000, -1.000000000000000000 ) ) ;
#55631 = DIRECTION ( 'NONE',  ( -0.5449076811759708816, 0.6444004775717707689, 0.5364919789714475140 ) ) ;
#55633 = ADVANCED_FACE ( 'NONE', ( #15432 ), #45819, .F. ) ;
#55632 = ORIENTED_EDGE ( 'NONE', *, *, #19438, .T. ) ;
#55634 = AXIS2_PLACEMENT_3D ( 'NONE', #11505, #50673, #1833 ) ;
#55635 = CARTESIAN_POINT ( 'NONE',  ( -23.33693525117809386, 0.000000000000000000, 5.746789908705562944 ) ) ;
#55636 = CARTESIAN_POINT ( 'NONE',  ( -12.67276438359499124, -0.1191753592594168437, 7.776444329389642363 ) ) ;
#55637 = ORIENTED_EDGE ( 'NONE', *, *, #13639, .T. ) ;
#55638 = CARTESIAN_POINT ( 'NONE',  ( -17.58751131637929177, 5.143464774974010112, 12.15420974568715273 ) ) ;
#55639 = ADVANCED_FACE ( 'NONE', ( #23676 ), #40543, .T. ) ;
#55640 = ADVANCED_FACE ( 'NONE', ( #12006 ), #3222, .F. ) ;
#55641 = EDGE_CURVE ( 'NONE', #31613, #40733, #30185, .T. ) ;
#55642 = VECTOR ( 'NONE', #14335, 999.9999999999998863 ) ;
#55643 = VECTOR ( 'NONE', #41687, 1000.000000000000227 ) ;
#55644 = VERTEX_POINT ( 'NONE', #25370 ) ;
#55645 = FACE_OUTER_BOUND ( 'NONE', #52550, .T. ) ;
#55646 = AXIS2_PLACEMENT_3D ( 'NONE', #44363, #13984, #4624 ) ;
#55647 = DIRECTION ( 'NONE',  ( -0.9999697198139514409, -0.000000000000000000, -0.007781995580013368816 ) ) ;
#55648 = VECTOR ( 'NONE', #46227, 999.9999999999998863 ) ;
#55649 = ORIENTED_EDGE ( 'NONE', *, *, #25010, .T. ) ;
#55650 = DIRECTION ( 'NONE',  ( -0.005002170337468016433, -0.7660444431189770143, 0.6427681459581293666 ) ) ;
#55651 = LINE ( 'NONE', #38906, #14768 ) ;
#55652 = CARTESIAN_POINT ( 'NONE',  ( -14.85936739980835064, 0.000000000000000000, 3.058113799738058969 ) ) ;
#55653 = PLANE ( 'NONE',  #25604 ) ;
#55654 = EDGE_LOOP ( 'NONE', ( #6716, #38369, #626, #12013 ) ) ;
#55655 = CARTESIAN_POINT ( 'NONE',  ( -28.93060053386082231, -0.1191753592594197858, 8.019254159017428663 ) ) ;
#55656 = CARTESIAN_POINT ( 'NONE',  ( -9.213964613319133079, 8.977402042007843974, 6.797390339032328477 ) ) ;
#55657 = DIRECTION ( 'NONE',  ( 0.005961354470445682716, -0.6427876096865404731, -0.7660212471507180654 ) ) ;
#55658 = ADVANCED_FACE ( 'NONE', ( #4368 ), #37881, .F. ) ;
#55659 = DIRECTION ( 'NONE',  ( 1.000000000000000000, 0.000000000000000000, -8.673617379884027583E-16 ) ) ;
#55660 = DIRECTION ( 'NONE',  ( 0.007781995580012663651, 0.000000000000000000, -0.9999697198139515519 ) ) ;
#55661 = DIRECTION ( 'NONE',  ( -0.9999697198139514409, -0.000000000000000000, -0.007781995580013368816 ) ) ;
#55662 = EDGE_CURVE ( 'NONE', #44458, #44358, #3449, .T. ) ;
#55663 = DIRECTION ( 'NONE',  ( 0.005002170337468016433, -0.7660444431189770143, -0.6427681459581293666 ) ) ;
#55664 = AXIS2_PLACEMENT_3D ( 'NONE', #29618, #47177, #42381 ) ;
#55665 = ORIENTED_EDGE ( 'NONE', *, *, #20357, .T. ) ;
#55666 =( LENGTH_UNIT ( ) NAMED_UNIT ( * ) SI_UNIT ( .MILLI., .METRE. ) );
#55667 = ADVANCED_FACE ( 'NONE', ( #52037 ), #21399, .F. ) ;
#55668 = CARTESIAN_POINT ( 'NONE',  ( -68.53670954776376334, 2.081668171172168513E-14, 8.455601507725491572 ) ) ;
#55669 = ORIENTED_EDGE ( 'NONE', *, *, #45998, .F. ) ;
#55670 = DIRECTION ( 'NONE',  ( 0.7660212471507180654, -0.6427876096865404731, 0.005961354470445141482 ) ) ;
#55671 = DIRECTION ( 'NONE',  ( 0.9999697198139515519, 0.000000000000000000, 0.007781995580013368816 ) ) ;
#55672 = AXIS2_PLACEMENT_3D ( 'NONE', #46414, #3557, #41876 ) ;
#55673 = EDGE_CURVE ( 'NONE', #26368, #34449, #26213, .T. ) ;
#55674 = DIRECTION ( 'NONE',  ( 0.5364919789714477361, 0.6444004775717706579, 0.5449076811759711036 ) ) ;
#55675 = VECTOR ( 'NONE', #45326, 1000.000000000000114 ) ;
#55676 = CARTESIAN_POINT ( 'NONE',  ( 2.072287782118878319, 0.000000000000000000, -2.950529333540147015 ) ) ;
#55677 = LINE ( 'NONE', #15943, #14785 ) ;
#55678 = EDGE_LOOP ( 'NONE', ( #25816, #31803, #13926, #380 ) ) ;
#55679 = ORIENTED_EDGE ( 'NONE', *, *, #11972, .T. ) ;
#55680 = CARTESIAN_POINT ( 'NONE',  ( -27.99923088623136636, 0.000000000000000000, 7.757173251277078130 ) ) ;
#55681 = AXIS2_PLACEMENT_3D ( 'NONE', #46059, #28449, #10861 ) ;
#55682 = CARTESIAN_POINT ( 'NONE',  ( -25.83278826518980154, 17.74370858705499288, -4.604226652742015702 ) ) ;
#55683 = VERTEX_POINT ( 'NONE', #20816 ) ;
#55684 =( GEOMETRIC_REPRESENTATION_CONTEXT ( 3 ) GLOBAL_UNCERTAINTY_ASSIGNED_CONTEXT ( ( #54661 ) ) GLOBAL_UNIT_ASSIGNED_CONTEXT ( ( #46273, #37207, #42023 ) ) REPRESENTATION_CONTEXT ( 'NONE', 'WORKASPACE' ) );
#55685 = DIRECTION ( 'NONE',  ( 0.007781995580012663651, -3.146120232559066537E-19, -0.9999697198139514409 ) ) ;
#55686 = ORIENTED_EDGE ( 'NONE', *, *, #50118, .T. ) ;
#55687 = PLANE ( 'NONE',  #6817 ) ;
#55688 = ORIENTED_EDGE ( 'NONE', *, *, #20893, .F. ) ;
#55689 = DIRECTION ( 'NONE',  ( 0.5449076811759707706, 0.6444004775717708799, -0.5364919789714476250 ) ) ;
#55690 = VECTOR ( 'NONE', #5285, 999.9999999999998863 ) ;
#55691 = EDGE_LOOP ( 'NONE', ( #4642, #33917, #11725, #15217 ) ) ;
#55692 = AXIS2_PLACEMENT_3D ( 'NONE', #39899, #5537, #35365 ) ;
#55693 = ORIENTED_EDGE ( 'NONE', *, *, #40781, .F. ) ;
#55694 = ORIENTED_EDGE ( 'NONE', *, *, #10290, .F. ) ;
#55695 = DIRECTION ( 'NONE',  ( -0.005002170337468016433, -0.7660444431189770143, 0.6427681459581293666 ) ) ;
#55696 = FACE_OUTER_BOUND ( 'NONE', #33919, .T. ) ;
#55697 = CARTESIAN_POINT ( 'NONE',  ( -16.89925026227929195, -0.1191753592594197858, 13.49466922669627422 ) ) ;
#55698 = DIRECTION ( 'NONE',  ( 0.005961354470445682716, -0.6427876096865404731, -0.7660212471507180654 ) ) ;
#55699 = ORIENTED_EDGE ( 'NONE', *, *, #16651, .F. ) ;
#55700 = ORIENTED_EDGE ( 'NONE', *, *, #40424, .F. ) ;
#55701 = VECTOR ( 'NONE', #37475, 1000.000000000000000 ) ;
#55702 = ORIENTED_EDGE ( 'NONE', *, *, #34231, .T. ) ;
#55703 = PLANE ( 'NONE',  #43141 ) ;
#55704 = DIRECTION ( 'NONE',  ( 0.9999697198139515519, 0.000000000000000000, 0.007781995580013368816 ) ) ;
#55705 = ORIENTED_EDGE ( 'NONE', *, *, #48767, .T. ) ;
#55706 = CARTESIAN_POINT ( 'NONE',  ( -25.20278734466900517, 0.000000000000000000, 6.670939612111840944 ) ) ;
#55707 = ORIENTED_EDGE ( 'NONE', *, *, #20093, .F. ) ;
#55708 = AXIS2_PLACEMENT_3D ( 'NONE', #24431, #14808, #32135 ) ;
#55709 = DIRECTION ( 'NONE',  ( -0.7660212471507179544, -0.6427876096865405842, -0.005961354470445141482 ) ) ;
#55710 = FACE_OUTER_BOUND ( 'NONE', #41188, .T. ) ;
#55711 = ADVANCED_FACE ( 'NONE', ( #43274 ), #8911, .F. ) ;
#55712 = EDGE_CURVE ( 'NONE', #36408, #37378, #38421, .T. ) ;
#55713 = ORIENTED_EDGE ( 'NONE', *, *, #39732, .F. ) ;
#55714 = CARTESIAN_POINT ( 'NONE',  ( -19.60990026154428278, 0.000000000000000000, 4.498472333781370125 ) ) ;
#55715 = EDGE_LOOP ( 'NONE', ( #55544, #8937, #47732, #22512 ) ) ;
#55716 = EDGE_CURVE ( 'NONE', #55542, #53648, #16274, .T. ) ;
#55717 = LINE ( 'NONE', #51475, #33642 ) ;
#55718 = PLANE ( 'NONE',  #35660 ) ;
#55719 = VECTOR ( 'NONE', #26531, 1000.000000000000227 ) ;
#55720 = ORIENTED_EDGE ( 'NONE', *, *, #19225, .F. ) ;
#55721 = DIRECTION ( 'NONE',  ( -0.005961354470445682716, -0.6427876096865404731, 0.7660212471507180654 ) ) ;
#55722 = DIRECTION ( 'NONE',  ( 0.6427681459581294776, -0.7660444431189769032, 0.005002170337467562802 ) ) ;
#55723 = PLANE ( 'NONE',  #26044 ) ;
#55724 = AXIS2_PLACEMENT_3D ( 'NONE', #35447, #8801, #22418 ) ;
#55725 = PLANE ( 'NONE',  #50931 ) ;
#55726 = VERTEX_POINT ( 'NONE', #50905 ) ;
#55727 = VECTOR ( 'NONE', #45806, 1000.000000000000000 ) ;
#55728 = CARTESIAN_POINT ( 'NONE',  ( -14.01975593143325050, 3.200641362704010451, 2.025563831507627643 ) ) ;
#55729 = FACE_OUTER_BOUND ( 'NONE', #19100, .T. ) ;
#55730 = CARTESIAN_POINT ( 'NONE',  ( -17.26532721389163072, 0.000000000000000000, 13.67648636611514590 ) ) ;
#55731 = LINE ( 'NONE', #47794, #6766 ) ;
#55733 = ADVANCED_FACE ( 'NONE', ( #29346 ), #25636, .F. ) ;
#55732 = LINE ( 'NONE', #16848, #17960 ) ;
#55734 = AXIS2_PLACEMENT_3D ( 'NONE', #19663, #40409, #27327 ) ;
#55735 = VECTOR ( 'NONE', #54765, 1000.000000000000227 ) ;
#55736 = PLANE ( 'NONE',  #17665 ) ;
#55737 = ORIENTED_EDGE ( 'NONE', *, *, #38058, .T. ) ;
#55738 = CARTESIAN_POINT ( 'NONE',  ( -23.33693525117809386, 0.000000000000000000, 5.746789908705562944 ) ) ;
#55739 = CARTESIAN_POINT ( 'NONE',  ( -10.37421533196711465, -0.1191753592594197858, 10.96012406864405975 ) ) ;
#55740 = ADVANCED_FACE ( 'NONE', ( #30488 ), #38729, .F. ) ;
#55741 = FACE_OUTER_BOUND ( 'NONE', #38358, .T. ) ;
#55742 = VERTEX_POINT ( 'NONE', #46657 ) ;
#55743 = LINE ( 'NONE', #51751, #45865 ) ;
#55744 = ORIENTED_EDGE ( 'NONE', *, *, #4568, .T. ) ;
#55745 = CARTESIAN_POINT ( 'NONE',  ( -23.39689275304487737, 18.96061820135890130, -4.493364476181771039 ) ) ;
#55746 = CARTESIAN_POINT ( 'NONE',  ( -15.13495153988577968, 0.000000000000000000, 12.76973526769478084 ) ) ;
#55747 = ADVANCED_FACE ( 'NONE', ( #7781 ), #55449, .F. ) ;
#55748 = DIRECTION ( 'NONE',  ( 0.9999697198139515519, 0.000000000000000000, 0.007781995580013368816 ) ) ;
#55749 = ADVANCED_FACE ( 'NONE', ( #29657 ), #46956, .F. ) ;
#55750 = CARTESIAN_POINT ( 'NONE',  ( -67.33498797961308924, 0.1329898013568112103, 0.6944083026028426975 ) ) ;
#55751 = VECTOR ( 'NONE', #34444, 1000.000000000000227 ) ;
#55752 = ORIENTED_EDGE ( 'NONE', *, *, #17742, .F. ) ;
#55753 = ORIENTED_EDGE ( 'NONE', *, *, #33495, .F. ) ;
#55754 = VECTOR ( 'NONE', #11971, 1000.000000000000227 ) ;
#55755 = CARTESIAN_POINT ( 'NONE',  ( -68.82653453192783388, -0.6013598542774325484, 6.387117138744211609 ) ) ;
#55756 = PLANE ( 'NONE',  #22235 ) ;
#55757 = DIRECTION ( 'NONE',  ( 0.9999697198139515519, 0.000000000000000000, 0.007781995580013368816 ) ) ;
#55758 = VECTOR ( 'NONE', #20466, 999.9999999999998863 ) ;
#55759 = CARTESIAN_POINT ( 'NONE',  ( -9.385817463643999048, -0.1191753592594190225, 3.370039272672538999 ) ) ;
#55760 = CARTESIAN_POINT ( 'NONE',  ( -15.02722544478543831, -4.565544526780662693, 10.01185279549585516 ) ) ;
#55761 = DIRECTION ( 'NONE',  ( 0.9999697198139515519, 0.000000000000000000, 0.007781995580013368816 ) ) ;
#55762 = AXIS2_PLACEMENT_3D ( 'NONE', #46272, #46023, #41485 ) ;
#55763 = EDGE_LOOP ( 'NONE', ( #9447, #53500, #15418, #38080 ) ) ;
#55764 = CARTESIAN_POINT ( 'NONE',  ( -17.74404816805336793, 0.000000000000000000, 3.574322630375089460 ) ) ;
#55765 = CARTESIAN_POINT ( 'NONE',  ( -29.86274838104827367, -0.1191753592594197858, 8.381332038739175871 ) ) ;
#55766 = VECTOR ( 'NONE', #23648, 999.9999999999998863 ) ;
#55768 = VERTEX_POINT ( 'NONE', #56041 ) ;
#55767 = VECTOR ( 'NONE', #47203, 1000.000000000000227 ) ;
#55769 = VECTOR ( 'NONE', #1949, 1000.000000000000227 ) ;
#55770 = VECTOR ( 'NONE', #21201, 999.9999999999998863 ) ;
#55771 = CARTESIAN_POINT ( 'NONE',  ( -11.81265117289410504, 0.000000000000000000, 3.820488189513650656 ) ) ;
#55772 = CARTESIAN_POINT ( 'NONE',  ( -13.90996791376045927, 4.657758921906511418, 9.928600946358965729 ) ) ;
#55773 = DIRECTION ( 'NONE',  ( 0.5449076811759707706, 0.6444004775717708799, -0.5364919789714476250 ) ) ;
#55774 = AXIS2_PLACEMENT_3D ( 'NONE', #48897, #31590, #44351 ) ;
#55775 = EDGE_LOOP ( 'NONE', ( #9378, #11732, #13400, #8729 ) ) ;
#55776 = FACE_OUTER_BOUND ( 'NONE', #44802, .T. ) ;
#55777 = ORIENTED_EDGE ( 'NONE', *, *, #24669, .T. ) ;
#55778 = VECTOR ( 'NONE', #42363, 999.9999999999998863 ) ;
#55779 = ORIENTED_EDGE ( 'NONE', *, *, #15764, .T. ) ;
#55780 = VECTOR ( 'NONE', #703, 1000.000000000000114 ) ;
#55781 = ORIENTED_EDGE ( 'NONE', *, *, #41430, .T. ) ;
#55782 = ORIENTED_EDGE ( 'NONE', *, *, #22506, .T. ) ;
#55783 = CARTESIAN_POINT ( 'NONE',  ( 2.072287782118878319, 0.000000000000000000, -2.950529333540147015 ) ) ;
#55784 = ORIENTED_EDGE ( 'NONE', *, *, #4761, .T. ) ;
#55785 = CARTESIAN_POINT ( 'NONE',  ( -12.24874546236494588, 23.85440854838047642, -3.504140126263841637 ) ) ;
#55786 = ADVANCED_FACE ( 'NONE', ( #17135 ), #51504, .F. ) ;
#55787 = ORIENTED_EDGE ( 'NONE', *, *, #48333, .F. ) ;
#55788 = DIRECTION ( 'NONE',  ( 0.005002170337468016433, -0.7660444431189770143, -0.6427681459581293666 ) ) ;
#55789 = ORIENTED_EDGE ( 'NONE', *, *, #29237, .T. ) ;
#55790 = EDGE_LOOP ( 'NONE', ( #34621, #39358, #28446, #3597 ) ) ;
#55791 = EDGE_CURVE ( 'NONE', #8005, #6902, #48059, .T. ) ;
#55792 = EDGE_CURVE ( 'NONE', #33095, #8533, #22520, .T. ) ;
#55793 = AXIS2_PLACEMENT_3D ( 'NONE', #14904, #40482, #6129 ) ;
#55794 = CARTESIAN_POINT ( 'NONE',  ( -19.54294029912370334, 21.18270206417091828, 4.260498045019209812 ) ) ;
#55795 = VECTOR ( 'NONE', #54430, 999.9999999999998863 ) ;
#55796 = CARTESIAN_POINT ( 'NONE',  ( -21.06406398147228032, -2.946525016555659793, 4.969309331428991783 ) ) ;
#55797 = CARTESIAN_POINT ( 'NONE',  ( -17.11715711133786400, -5.375054281893161701, 12.15219664891527351 ) ) ;
#55798 = DIRECTION ( 'NONE',  ( 0.9999697198139515519, 0.000000000000000000, 0.007781995580013368816 ) ) ;
#55799 = CARTESIAN_POINT ( 'NONE',  ( -18.67775241435682432, 0.000000000000000000, 4.136394454059623804 ) ) ;
#55800 = VECTOR ( 'NONE', #17456, 1000.000000000000227 ) ;
#55801 = ORIENTED_EDGE ( 'NONE', *, *, #6827, .T. ) ;
#55802 = ORIENTED_EDGE ( 'NONE', *, *, #43525, .T. ) ;
#55803 = CARTESIAN_POINT ( 'NONE',  ( -13.21937573182777115, 0.000000000000000000, 5.456195026535657355 ) ) ;
#55804 = FACE_OUTER_BOUND ( 'NONE', #23187, .T. ) ;
#55805 = AXIS2_PLACEMENT_3D ( 'NONE', #49374, #10490, #45128 ) ;
#55806 = UNCERTAINTY_MEASURE_WITH_UNIT (LENGTH_MEASURE( 1.000000000000000082E-05 ), #55666, 'distance_accuracy_value', 'NONE');
#55807 = CARTESIAN_POINT ( 'NONE',  ( -11.70701794508347682, -0.6798977022406563764, 2.345163033079200599 ) ) ;
#55808 = AXIS2_PLACEMENT_3D ( 'NONE', #19320, #882, #53971 ) ;
#55809 = VECTOR ( 'NONE', #34000, 1000.000000000000227 ) ;
#55810 = CARTESIAN_POINT ( 'NONE',  ( -45.77156441860526570, 4.499999999999973355, 5.000000000000000000 ) ) ;
#55811 = LINE ( 'NONE', #35351, #40337 ) ;
#55812 = PLANE ( 'NONE',  #2365 ) ;
#55813 = ORIENTED_EDGE ( 'NONE', *, *, #16285, .F. ) ;
#55814 = LINE ( 'NONE', #16621, #31081 ) ;
#55815 = CARTESIAN_POINT ( 'NONE',  ( -58.00000000000000711, 0.000000000000000000, 7.102951435054649637E-15 ) ) ;
#55816 = ORIENTED_EDGE ( 'NONE', *, *, #50328, .T. ) ;
#55817 = AXIS2_PLACEMENT_3D ( 'NONE', #28082, #28651, #11609 ) ;
#55818 = PLANE ( 'NONE',  #20711 ) ;
#55819 = LINE ( 'NONE', #4147, #5196 ) ;
#55820 = AXIS2_PLACEMENT_3D ( 'NONE', #41534, #32182, #2615 ) ;
#55821 = DIRECTION ( 'NONE',  ( 0.007781995580012663651, 0.000000000000000000, -0.9999697198139515519 ) ) ;
#55822 = ADVANCED_FACE ( 'NONE', ( #5746 ), #52597, .F. ) ;
#55823 = DIRECTION ( 'NONE',  ( 0.007781995580012662783, 0.000000000000000000, -0.9999697198139514409 ) ) ;
#55824 = VECTOR ( 'NONE', #13715, 1000.000000000000227 ) ;
#55825 = EDGE_LOOP ( 'NONE', ( #29270, #19142, #14257, #43313 ) ) ;
#55826 = AXIS2_PLACEMENT_3D ( 'NONE', #54334, #7468, #29338 ) ;
#55827 = ADVANCED_FACE ( 'NONE', ( #5463 ), #908, .F. ) ;
#55828 = ORIENTED_EDGE ( 'NONE', *, *, #44957, .T. ) ;
#55829 = DIRECTION ( 'NONE',  ( 0.000000000000000000, 0.000000000000000000, -1.000000000000000000 ) ) ;
#55830 = DIRECTION ( 'NONE',  ( 0.6427681459581294776, -0.7660444431189769032, 0.005002170337467562802 ) ) ;
#55831 = LINE ( 'NONE', #16941, #5237 ) ;
#55832 = PLANE ( 'NONE',  #46387 ) ;
#55833 = EDGE_CURVE ( 'NONE', #35388, #37328, #35559, .T. ) ;
#55834 = DIRECTION ( 'NONE',  ( 0.007781995580012663651, -3.146120232559066537E-19, -0.9999697198139514409 ) ) ;
#55835 = CARTESIAN_POINT ( 'NONE',  ( -12.81737946304616926, 25.25815836258565383, -3.463348302191213257 ) ) ;
#55836 = CARTESIAN_POINT ( 'NONE',  ( -1.086233639165236964, 0.000000000000000000, -2.796443541562362078 ) ) ;
#55837 = VECTOR ( 'NONE', #360, 1000.000000000000227 ) ;
#55838 = LINE ( 'NONE', #8405, #38654 ) ;
#55839 = CARTESIAN_POINT ( 'NONE',  ( -67.55782011861325032, -8.435184460786505412, -3.909888324369926060 ) ) ;
#55840 = VECTOR ( 'NONE', #39026, 1000.000000000000227 ) ;
#55841 = PLANE ( 'NONE',  #35640 ) ;
#55842 = EDGE_LOOP ( 'NONE', ( #40782, #3256, #37243, #5362 ) ) ;
#55843 = CARTESIAN_POINT ( 'NONE',  ( -13.22799789234362500, 0.000000000000000000, 6.564124136308949531 ) ) ;
#55844 = VECTOR ( 'NONE', #13558, 1000.000000000000227 ) ;
#55845 = EDGE_LOOP ( 'NONE', ( #16434, #4471, #17167 ) ) ;
#55846 = AXIS2_PLACEMENT_3D ( 'NONE', #22450, #18155, #1101 ) ;
#55847 = VERTEX_POINT ( 'NONE', #4622 ) ;
#55848 = EDGE_CURVE ( 'NONE', #3085, #20285, #22776, .T. ) ;
#55849 = VERTEX_POINT ( 'NONE', #9441 ) ;
#55850 = VECTOR ( 'NONE', #41683, 1000.000000000000227 ) ;
#55851 = ORIENTED_EDGE ( 'NONE', *, *, #29003, .T. ) ;
#55852 = AXIS2_PLACEMENT_3D ( 'NONE', #25924, #50882, #3486 ) ;
#55853 = ORIENTED_EDGE ( 'NONE', *, *, #16541, .T. ) ;
#55854 = ORIENTED_EDGE ( 'NONE', *, *, #12613, .F. ) ;
#55855 = PLANE ( 'NONE',  #15922 ) ;
#55856 = VECTOR ( 'NONE', #38190, 999.9999999999998863 ) ;
#55857 = DIRECTION ( 'NONE',  ( -0.6427681459581293666, -0.7660444431189770143, -0.005002170337467561935 ) ) ;
#55858 = EDGE_CURVE ( 'NONE', #866, #42669, #13983, .T. ) ;
#55859 = CARTESIAN_POINT ( 'NONE',  ( -19.35468857659533626, 0.1245042932765041271, 4.195977723824240613 ) ) ;
#55860 = VECTOR ( 'NONE', #20559, 1000.000000000000227 ) ;
#55861 = VECTOR ( 'NONE', #9331, 1000.000000000000000 ) ;
#55863 = EDGE_CURVE ( 'NONE', #33916, #13325, #19808, .T. ) ;
#55862 = ORIENTED_EDGE ( 'NONE', *, *, #49306, .F. ) ;
#55864 = CARTESIAN_POINT ( 'NONE',  ( -19.53399721238895026, -0.1191753592594167188, 7.353716559204084291 ) ) ;
#55865 = ORIENTED_EDGE ( 'NONE', *, *, #31623, .F. ) ;
#55866 = DIRECTION ( 'NONE',  ( -0.005002170337468016433, -0.7660444431189770143, 0.6427681459581293666 ) ) ;
#55867 = VERTEX_POINT ( 'NONE', #9748 ) ;
#55868 = EDGE_CURVE ( 'NONE', #5924, #5706, #31309, .T. ) ;
#55869 = ADVANCED_FACE ( 'NONE', ( #53184 ), #4908, .F. ) ;
#55870 = VECTOR ( 'NONE', #40891, 1000.000000000000000 ) ;
#55871 = VECTOR ( 'NONE', #9602, 1000.000000000000227 ) ;
#55872 = CARTESIAN_POINT ( 'NONE',  ( -16.27914457187915431, 0.000000000000000000, 6.371053393753911109 ) ) ;
#55873 = PLANE ( 'NONE',  #21937 ) ;
#55874 = FACE_OUTER_BOUND ( 'NONE', #47853, .T. ) ;
#55875 = VERTEX_POINT ( 'NONE', #48638 ) ;
#55876 = DIRECTION ( 'NONE',  ( -0.8531650599175527594, 0.4028455766673922356, 0.3313982828793700652 ) ) ;
#55877 = ORIENTED_EDGE ( 'NONE', *, *, #46174, .F. ) ;
#55878 = DIRECTION ( 'NONE',  ( 0.7660212471507180654, -0.6427876096865404731, 0.005961354470445141482 ) ) ;
#55879 = CARTESIAN_POINT ( 'NONE',  ( -29.86274838104827367, -0.1191753592594197858, 8.381332038739175871 ) ) ;
#55880 = VECTOR ( 'NONE', #857, 999.9999999999998863 ) ;
#55881 = ADVANCED_FACE ( 'NONE', ( #10003 ), #35031, .F. ) ;
#55882 = DIRECTION ( 'NONE',  ( 0.007781995580012663651, -3.146120232559066537E-19, -0.9999697198139514409 ) ) ;
#55883 = LINE ( 'NONE', #3360, #31327 ) ;
#55884 = LINE ( 'NONE', #42532, #32917 ) ;
#55885 = CARTESIAN_POINT ( 'NONE',  ( -15.86710544311044302, 0.000000000000000000, 13.13336954653252953 ) ) ;
#55886 = CARTESIAN_POINT ( 'NONE',  ( -21.47341775636118655, -0.1191753592594197858, 5.122631121243466090 ) ) ;
#55887 = FACE_OUTER_BOUND ( 'NONE', #37077, .T. ) ;
#55888 = ORIENTED_EDGE ( 'NONE', *, *, #6967, .T. ) ;
#55889 = DIRECTION ( 'NONE',  ( 0.9999697198139515519, 0.000000000000000000, 0.007781995580013368816 ) ) ;
#55890 = ORIENTED_EDGE ( 'NONE', *, *, #39078, .F. ) ;
#55891 = VECTOR ( 'NONE', #6938, 1000.000000000000114 ) ;
#55892 = LINE ( 'NONE', #25492, #38341 ) ;
#55893 = DIRECTION ( 'NONE',  ( 0.6427681459581294776, -0.7660444431189769032, 0.005002170337467562802 ) ) ;
#55895 = LINE ( 'NONE', #8769, #48988 ) ;
#55894 = VECTOR ( 'NONE', #29067, 999.9999999999998863 ) ;
#55896 = FACE_OUTER_BOUND ( 'NONE', #25089, .T. ) ;
#55897 = LINE ( 'NONE', #43112, #35891 ) ;
#55898 = VECTOR ( 'NONE', #1676, 1000.000000000000000 ) ;
#55899 = DIRECTION ( 'NONE',  ( 0.7660212471507180654, -0.6427876096865404731, 0.005961354470445141482 ) ) ;
#55900 = ORIENTED_EDGE ( 'NONE', *, *, #34203, .F. ) ;
#55901 = PLANE ( 'NONE',  #1205 ) ;
#55902 = DIRECTION ( 'NONE',  ( 0.9999697198139515519, 0.000000000000000000, 0.007781995580013368816 ) ) ;
#55903 = LINE ( 'NONE', #29498, #18205 ) ;
#55904 = VECTOR ( 'NONE', #27248, 1000.000000000000227 ) ;
#55905 = VECTOR ( 'NONE', #55798, 999.9999999999998863 ) ;
#55906 = DIRECTION ( 'NONE',  ( -0.2426528472758542054, 0.7422098413412800966, -0.6246952433987894571 ) ) ;
#55907 = EDGE_CURVE ( 'NONE', #34831, #30960, #27311, .T. ) ;
#55908 = FACE_OUTER_BOUND ( 'NONE', #44290, .T. ) ;
#55909 = PLANE ( 'NONE',  #40425 ) ;
#55910 = CARTESIAN_POINT ( 'NONE',  ( -14.04655669958127362, -0.1191753592594190225, 5.180428671281267050 ) ) ;
#55911 = ORIENTED_EDGE ( 'NONE', *, *, #37915, .T. ) ;
#55912 = VECTOR ( 'NONE', #29148, 1000.000000000000000 ) ;
#55914 = CARTESIAN_POINT ( 'NONE',  ( -13.69993929531127641, 0.000000000000000000, 7.499121575019257691 ) ) ;
#55913 = VECTOR ( 'NONE', #52875, 999.9999999999998863 ) ;
#55915 = DIRECTION ( 'NONE',  ( 0.000000000000000000, -0.000000000000000000, -1.000000000000000000 ) ) ;
#55916 = ORIENTED_EDGE ( 'NONE', *, *, #2961, .F. ) ;
#55917 = ORIENTED_EDGE ( 'NONE', *, *, #26061, .F. ) ;
#55918 = LINE ( 'NONE', #41985, #17415 ) ;
#55919 = EDGE_CURVE ( 'NONE', #21299, #48957, #21932, .T. ) ;
#55920 = ORIENTED_EDGE ( 'NONE', *, *, #12607, .F. ) ;
#55921 = EDGE_CURVE ( 'NONE', #15829, #21263, #26472, .T. ) ;
#55922 = ADVANCED_FACE ( 'NONE', ( #34712 ), #43782, .F. ) ;
#55923 = VECTOR ( 'NONE', #8076, 999.9999999999998863 ) ;
#55924 = ORIENTED_EDGE ( 'NONE', *, *, #43917, .F. ) ;
#55925 = ORIENTED_EDGE ( 'NONE', *, *, #46747, .F. ) ;
#55926 = ORIENTED_EDGE ( 'NONE', *, *, #3850, .F. ) ;
#55927 = PLANE ( 'NONE',  #23030 ) ;
#55928 = VERTEX_POINT ( 'NONE', #4361 ) ;
#55929 = LINE ( 'NONE', #34908, #8787 ) ;
#55930 = EDGE_CURVE ( 'NONE', #2677, #16356, #13147, .T. ) ;
#55931 = LINE ( 'NONE', #29531, #19442 ) ;
#55932 = ADVANCED_FACE ( 'NONE', ( #30752 ), #52029, .F. ) ;
#55933 = VECTOR ( 'NONE', #2106, 999.9999999999998863 ) ;
#55934 = ORIENTED_EDGE ( 'NONE', *, *, #25472, .F. ) ;
#55935 = ORIENTED_EDGE ( 'NONE', *, *, #16918, .F. ) ;
#55936 = EDGE_CURVE ( 'NONE', #47379, #18119, #22224, .T. ) ;
#55937 = VECTOR ( 'NONE', #21796, 1000.000000000000000 ) ;
#55938 = CARTESIAN_POINT ( 'NONE',  ( -65.65478415642573395, -1.821459649775647449E-14, 1.319813854473108838 ) ) ;
#55939 = PLANE ( 'NONE',  #41763 ) ;
#55940 = EDGE_LOOP ( 'NONE', ( #6641, #30359, #10090, #52561 ) ) ;
#55941 = CARTESIAN_POINT ( 'NONE',  ( -14.20280369269832832, 0.000000000000000000, 12.40765738797303719 ) ) ;
#55942 = LINE ( 'NONE', #3672, #10517 ) ;
#55943 = EDGE_LOOP ( 'NONE', ( #17315, #8727, #49506, #19106 ) ) ;
#55944 = DIRECTION ( 'NONE',  ( -0.5449076811759708816, 0.6444004775717707689, 0.5364919789714475140 ) ) ;
#55945 = EDGE_CURVE ( 'NONE', #27546, #30961, #8052, .T. ) ;
#55946 = ORIENTED_EDGE ( 'NONE', *, *, #959, .F. ) ;
#55947 = VECTOR ( 'NONE', #492, 1000.000000000000000 ) ;
#55948 = LINE ( 'NONE', #4803, #45463 ) ;
#55949 = EDGE_CURVE ( 'NONE', #39505, #34282, #47205, .T. ) ;
#55950 = DIRECTION ( 'NONE',  ( -0.9999697198139514409, -0.000000000000000000, -0.007781995580013368816 ) ) ;
#55951 = VECTOR ( 'NONE', #31238, 1000.000000000000000 ) ;
#55952 = ORIENTED_EDGE ( 'NONE', *, *, #38894, .T. ) ;
#55953 = DIRECTION ( 'NONE',  ( -0.9983709377222390602, -0.05705673239519638146, 0.000000000000000000 ) ) ;
#55954 = PLANE ( 'NONE',  #55572 ) ;
#55955 = DIRECTION ( 'NONE',  ( 0.5364919789714477361, 0.6444004775717706579, 0.5449076811759711036 ) ) ;
#55956 = DIRECTION ( 'NONE',  ( 0.9999697198139515519, 0.000000000000000000, 0.007781995580013368816 ) ) ;
#55957 = ORIENTED_EDGE ( 'NONE', *, *, #41119, .T. ) ;
#55958 = CARTESIAN_POINT ( 'NONE',  ( -10.74029228357944987, 0.000000000000000000, 11.14194120806293320 ) ) ;
#55959 = FACE_OUTER_BOUND ( 'NONE', #24470, .T. ) ;
#55960 = CARTESIAN_POINT ( 'NONE',  ( -11.16370825400592359, 0.000000000000000000, 5.841524775981462803 ) ) ;
#55961 = CARTESIAN_POINT ( 'NONE',  ( 2.072287782118878319, 0.000000000000000000, -2.950529333540147015 ) ) ;
#55962 = DIRECTION ( 'NONE',  ( 0.005961354470445682716, -0.6427876096865404731, -0.7660212471507180654 ) ) ;
#55963 = FACE_OUTER_BOUND ( 'NONE', #13353, .T. ) ;
#55964 = LINE ( 'NONE', #20471, #29802 ) ;
#55965 = AXIS2_PLACEMENT_3D ( 'NONE', #9408, #43490, #4589 ) ;
#55966 = PLANE ( 'NONE',  #25694 ) ;
#55967 = CARTESIAN_POINT ( 'NONE',  ( -16.39560766533424641, -0.1191753592594190225, 8.486136441761102489 ) ) ;
#55968 = ORIENTED_EDGE ( 'NONE', *, *, #22720, .F. ) ;
#55969 = CARTESIAN_POINT ( 'NONE',  ( -17.74404816805336793, 0.000000000000000000, 3.574322630375089460 ) ) ;
#55970 = VERTEX_POINT ( 'NONE', #48 ) ;
#55971 = DIRECTION ( 'NONE',  ( 0.005002170337468016433, -0.7660444431189770143, -0.6427681459581293666 ) ) ;
#55972 = DIRECTION ( 'NONE',  ( 0.9999697198139515519, 0.000000000000000000, 0.007781995580013368816 ) ) ;
#55973 = VECTOR ( 'NONE', #19085, 1000.000000000000000 ) ;
#55974 = CARTESIAN_POINT ( 'NONE',  ( -23.29661994227107868, 19.01267450544941084, 4.488313114961025363 ) ) ;
#55975 = EDGE_CURVE ( 'NONE', #13455, #48904, #648, .T. ) ;
#55976 = CARTESIAN_POINT ( 'NONE',  ( -16.43317633868556626, -0.1191753592594197858, 13.31363028683540151 ) ) ;
#55977 = DIRECTION ( 'NONE',  ( 0.005961354470445682716, -0.6427876096865404731, -0.7660212471507180654 ) ) ;
#55978 = VERTEX_POINT ( 'NONE', #4063 ) ;
#55979 = TOROIDAL_SURFACE ( 'NONE', #6098, 2.750000000000006217, 1.000000000000000000 ) ;
#55980 = ORIENTED_EDGE ( 'NONE', *, *, #16669, .F. ) ;
#55981 = DIRECTION ( 'NONE',  ( -0.005961354470445682716, -0.6427876096865404731, 0.7660212471507180654 ) ) ;
#55982 = LINE ( 'NONE', #25883, #19553 ) ;
#55983 = VERTEX_POINT ( 'NONE', #30177 ) ;
#55984 = ADVANCED_FACE ( 'NONE', ( #21389 ), #38722, .F. ) ;
#55985 = ADVANCED_FACE ( 'NONE', ( #13436 ), #56033, .F. ) ;
#55986 = DIRECTION ( 'NONE',  ( -0.6427681459581293666, -0.7660444431189770143, -0.005002170337467561935 ) ) ;
#55987 = VECTOR ( 'NONE', #23207, 1000.000000000000227 ) ;
#55988 = ORIENTED_EDGE ( 'NONE', *, *, #15275, .F. ) ;
#55989 = DIRECTION ( 'NONE',  ( 0.6427681459581294776, -0.7660444431189769032, 0.005002170337467562802 ) ) ;
#55990 = ORIENTED_EDGE ( 'NONE', *, *, #33992, .T. ) ;
#55991 = DIRECTION ( 'NONE',  ( 0.005961354470445682716, -0.6427876096865404731, -0.7660212471507180654 ) ) ;
#55992 = EDGE_CURVE ( 'NONE', #50299, #15763, #52589, .T. ) ;
#55993 = VERTEX_POINT ( 'NONE', #17124 ) ;
#55994 = VERTEX_POINT ( 'NONE', #48052 ) ;
#55995 = ORIENTED_EDGE ( 'NONE', *, *, #42466, .F. ) ;
#55996 = LINE ( 'NONE', #21634, #8479 ) ;
#55997 = PLANE ( 'NONE',  #17817 ) ;
#55998 = DIRECTION ( 'NONE',  ( -0.5449076811759708816, 0.6444004775717707689, 0.5364919789714475140 ) ) ;
#55999 = DIRECTION ( 'NONE',  ( 0.3535533905932752297, -0.6123724356957952475, -0.7071067811865462405 ) ) ;
#56000 = EDGE_CURVE ( 'NONE', #51035, #25453, #21925, .T. ) ;
#56001 = ORIENTED_EDGE ( 'NONE', *, *, #55248, .T. ) ;
#56002 = ORIENTED_EDGE ( 'NONE', *, *, #13346, .F. ) ;
#56003 = ADVANCED_FACE ( 'NONE', ( #16852 ), #34182, .F. ) ;
#56004 = ORIENTED_EDGE ( 'NONE', *, *, #438, .F. ) ;
#56005 = LINE ( 'NONE', #11706, #16826 ) ;
#56006 = CARTESIAN_POINT ( 'NONE',  ( -10.74029228357944987, 0.000000000000000000, 11.14194120806293320 ) ) ;
#56007 = EDGE_CURVE ( 'NONE', #26046, #7889, #51494, .T. ) ;
#56008 = ORIENTED_EDGE ( 'NONE', *, *, #3302, .T. ) ;
#56009 = DIRECTION ( 'NONE',  ( 0.005961354470445682716, -0.6427876096865404731, -0.7660212471507180654 ) ) ;
#56010 = ORIENTED_EDGE ( 'NONE', *, *, #10546, .F. ) ;
#56011 = PLANE ( 'NONE',  #45943 ) ;
#56012 = DIRECTION ( 'NONE',  ( 0.007781995580012663651, -3.146120232559066537E-19, -0.9999697198139514409 ) ) ;
#56013 = ADVANCED_FACE ( 'NONE', ( #51746 ), #39253, .F. ) ;
#56014 = ORIENTED_EDGE ( 'NONE', *, *, #43556, .T. ) ;
#56015 = LINE ( 'NONE', #9411, #48555 ) ;
#56016 = ORIENTED_EDGE ( 'NONE', *, *, #10159, .F. ) ;
#56017 = CIRCLE ( 'NONE', #12488, 2.750000000000006217 ) ;
#56018 = DIRECTION ( 'NONE',  ( 0.005002170337468016433, -0.7660444431189770143, -0.6427681459581293666 ) ) ;
#56019 = LINE ( 'NONE', #33573, #11201 ) ;
#56020 = ORIENTED_EDGE ( 'NONE', *, *, #41719, .F. ) ;
#56021 = DIRECTION ( 'NONE',  ( 0.007781995580012663651, -3.146120232559066537E-19, -0.9999697198139514409 ) ) ;
#56022 = CARTESIAN_POINT ( 'NONE',  ( -10.37421533196711465, -0.1191753592594197858, 10.96012406864405975 ) ) ;
#56023 = DIRECTION ( 'NONE',  ( 0.007781995580012663651, -3.146120232559066537E-19, -0.9999697198139514409 ) ) ;
#56024 = ORIENTED_EDGE ( 'NONE', *, *, #16120, .F. ) ;
#56025 = VECTOR ( 'NONE', #2301, 999.9999999999998863 ) ;
#56026 = CARTESIAN_POINT ( 'NONE',  ( -16.97058086006208555, 0.000000000000000000, 9.810323505063820448 ) ) ;
#56027 = LINE ( 'NONE', #52022, #43956 ) ;
#56028 = PLANE ( 'NONE',  #34942 ) ;
#56029 = DIRECTION ( 'NONE',  ( 0.5449076811759707706, 0.6444004775717708799, -0.5364919789714476250 ) ) ;
#56030 = DIRECTION ( 'NONE',  ( 0.007781995580012663651, 0.000000000000000000, -0.9999697198139515519 ) ) ;
#56031 = FACE_BOUND ( 'NONE', #50846, .T. ) ;
#56032 = ORIENTED_EDGE ( 'NONE', *, *, #19554, .T. ) ;
#56033 = PLANE ( 'NONE',  #21651 ) ;
#56034 = DIRECTION ( 'NONE',  ( 0.9090593428863094072, 0.000000000000000000, -0.4166666666666668517 ) ) ;
#56035 = CARTESIAN_POINT ( 'NONE',  ( -21.47263955680318404, 0.000000000000000000, 5.022634149262071190 ) ) ;
#56036 = VERTEX_POINT ( 'NONE', #21669 ) ;
#56037 = FACE_OUTER_BOUND ( 'NONE', #9044, .T. ) ;
#56038 = DIRECTION ( 'NONE',  ( 0.9999697198139515519, 0.000000000000000000, 0.007781995580013368816 ) ) ;
#56039 = VERTEX_POINT ( 'NONE', #17683 ) ;
#56040 = ADVANCED_FACE ( 'NONE', ( #15113 ), #31302, .F. ) ;
#56041 = CARTESIAN_POINT ( 'NONE',  ( -16.94952351969359583, 0.000000000000000000, 7.104500489385426221 ) ) ;
#56042 = CARTESIAN_POINT ( 'NONE',  ( -20.51565478868101167, 0.9340140483890049250, 6.383174327787997981 ) ) ;
#56043 = EDGE_CURVE ( 'NONE', #33095, #48860, #36138, .T. ) ;
#56044 = CARTESIAN_POINT ( 'NONE',  ( -19.12962290826653700, 0.000000000000000000, 14.40064212555863854 ) ) ;
#56045 = CARTESIAN_POINT ( 'NONE',  ( -65.33723405956592956, 1.999999999999986233, -0.8023217398950600598 ) ) ;
#56046 = ORIENTED_EDGE ( 'NONE', *, *, #54416, .T. ) ;
#56047 = ORIENTED_EDGE ( 'NONE', *, *, #17503, .T. ) ;
#56048 = DIRECTION ( 'NONE',  ( 0.007781995580012662783, 0.000000000000000000, -0.9999697198139514409 ) ) ;
#56049 = DIRECTION ( 'NONE',  ( 0.000000000000000000, -1.000000000000000000, 0.000000000000000000 ) ) ;
#56050 = DIRECTION ( 'NONE',  ( -0.6427681459581293666, -0.7660444431189770143, -0.005002170337467561935 ) ) ;
#56051 = ADVANCED_FACE ( 'NONE', ( #10276 ), #36387, .F. ) ;
#56052 = EDGE_CURVE ( 'NONE', #47466, #51306, #6305, .T. ) ;
#56053 = EDGE_CURVE ( 'NONE', #26718, #47865, #18817, .T. ) ;
#56054 = FACE_OUTER_BOUND ( 'NONE', #9487, .T. ) ;
#56055 = PLANE ( 'NONE',  #1068 ) ;
#56056 = LINE ( 'NONE', #47225, #23114 ) ;
#56058 = EDGE_CURVE ( 'NONE', #29102, #24902, #53701, .T. ) ;
#56057 = EDGE_LOOP ( 'NONE', ( #13274, #407, #2119, #40942 ) ) ;
#56059 = FACE_OUTER_BOUND ( 'NONE', #8505, .T. ) ;
#56060 = FACE_OUTER_BOUND ( 'NONE', #30183, .T. ) ;
#56061 = ORIENTED_EDGE ( 'NONE', *, *, #3906, .T. ) ;
#56062 = DIRECTION ( 'NONE',  ( -0.005002170337468016433, -0.7660444431189770143, 0.6427681459581293666 ) ) ;
#56063 = CARTESIAN_POINT ( 'NONE',  ( -5.316183009807136095, -7.201772371889491708, 5.283359595007837584 ) ) ;
#56064 = CARTESIAN_POINT ( 'NONE',  ( -17.83139810946674686, -0.1191753592594197858, 13.85674710641801788 ) ) ;
#56065 = ORIENTED_EDGE ( 'NONE', *, *, #38087, .F. ) ;
#56066 = AXIS2_PLACEMENT_3D ( 'NONE', #26271, #34793, #34505 ) ;
#56067 = DIRECTION ( 'NONE',  ( -0.005961354470445682716, -0.6427876096865404731, 0.7660212471507180654 ) ) ;
#56068 = ORIENTED_EDGE ( 'NONE', *, *, #54262, .T. ) ;
#56069 = EDGE_CURVE ( 'NONE', #16370, #693, #48901, .T. ) ;
#56071 = ORIENTED_EDGE ( 'NONE', *, *, #42633, .F. ) ;
#56070 = ADVANCED_FACE ( 'NONE', ( #9996 ), #27046, .F. ) ;
#56072 = ORIENTED_EDGE ( 'NONE', *, *, #6930, .T. ) ;
#56073 = B_SPLINE_CURVE_WITH_KNOTS ( 'NONE', 3,
 ( #28241, #2412, #50394, #19156 ),
 .UNSPECIFIED., .F., .F.,
 ( 4, 4 ),
 ( 0.0002402743607020580493, 0.0002683764075209547190 ),
 .UNSPECIFIED. ) ;
#56074 = EDGE_CURVE ( 'NONE', #31761, #40362, #5455, .T. ) ;
#56075 = ORIENTED_EDGE ( 'NONE', *, *, #49199, .T. ) ;
#56076 = DIRECTION ( 'NONE',  ( 0.5364919789714477361, 0.6444004775717706579, 0.5449076811759711036 ) ) ;
#56077 = B_SPLINE_CURVE_WITH_KNOTS ( 'NONE', 3,
 ( #37075, #36505, #49845, #15471 ),
 .UNSPECIFIED., .F., .F.,
 ( 4, 4 ),
 ( 0.5515979657728906638, 0.5753284354475328710 ),
 .UNSPECIFIED. ) ;
#56078 = VERTEX_POINT ( 'NONE', #53439 ) ;
#56079 = CARTESIAN_POINT ( 'NONE',  ( -13.44167438888726984, 23.16567071152870838, -3.718480911511438336 ) ) ;
#56080 = ADVANCED_FACE ( 'NONE', ( #40088 ), #1743, .F. ) ;
#56081 = VERTEX_POINT ( 'NONE', #40383 ) ;
#56082 = LINE ( 'NONE', #17168, #22284 ) ;
#56083 = ORIENTED_EDGE ( 'NONE', *, *, #36953, .F. ) ;
#56084 = PLANE ( 'NONE',  #33885 ) ;
#56085 = ORIENTED_EDGE ( 'NONE', *, *, #28799, .T. ) ;
#56086 = EDGE_CURVE ( 'NONE', #16370, #3478, #9432, .T. ) ;
#56087 = CARTESIAN_POINT ( 'NONE',  ( 1.086233639165236964, 0.000000000000000000, 2.796443541562362078 ) ) ;
#56088 = CARTESIAN_POINT ( 'NONE',  ( -19.25833773637261004, 0.000000000000000000, 5.239872414256555366 ) ) ;
#56089 = CARTESIAN_POINT ( 'NONE',  ( -11.40636015113596180, 0.000000000000000000, 11.32142374880780089 ) ) ;
#56090 = LINE ( 'NONE', #55497, #48652 ) ;
#56091 = CARTESIAN_POINT ( 'NONE',  ( -24.27063949748155380, 0.000000000000000000, 6.308861732390097288 ) ) ;
#56092 = ORIENTED_EDGE ( 'NONE', *, *, #46138, .F. ) ;
#56093 = ORIENTED_EDGE ( 'NONE', *, *, #21708, .T. ) ;
#56094 = DIRECTION ( 'NONE',  ( 0.007781995580012662783, 0.000000000000000000, -0.9999697198139514409 ) ) ;
#56095 = CARTESIAN_POINT ( 'NONE',  ( -19.81966461146206981, -0.3560938001956550081, 4.964973137040187723 ) ) ;
#56096 = PLANE ( 'NONE',  #24242 ) ;
#56097 = CARTESIAN_POINT ( 'NONE',  ( -13.59916412377187811, -0.1191753592594181482, 7.399902802595862639 ) ) ;
#56098 = CARTESIAN_POINT ( 'NONE',  ( -12.09806905913797515, 3.686347215771511365, 1.263618829885089667 ) ) ;
#56099 = CARTESIAN_POINT ( 'NONE',  ( 2.072287782118878319, 0.000000000000000000, -2.950529333540147015 ) ) ;
#56100 = VERTEX_POINT ( 'NONE', #53176 ) ;
#56101 = CARTESIAN_POINT ( 'NONE',  ( 2.072287782118878319, 0.000000000000000000, -2.950529333540147015 ) ) ;
#56102 = CARTESIAN_POINT ( 'NONE',  ( -25.20278734466900517, 0.000000000000000000, 6.670939612111840944 ) ) ;
#56103 = ORIENTED_EDGE ( 'NONE', *, *, #10998, .T. ) ;
#56104 = VECTOR ( 'NONE', #31007, 1000.000000000000227 ) ;
#56105 = LINE ( 'NONE', #47276, #27037 ) ;
#56106 = DIRECTION ( 'NONE',  ( -0.7660212471507179544, -0.6427876096865405842, -0.005961354470445141482 ) ) ;
#56107 = CARTESIAN_POINT ( 'NONE',  ( -22.40634380310664397, 0.000000000000000000, 5.584705972946605534 ) ) ;
#56108 = CARTESIAN_POINT ( 'NONE',  ( -19.53292050415603498, 0.000000000000000000, 6.515057770672818549 ) ) ;
#56109 = VERTEX_POINT ( 'NONE', #19342 ) ;
#56110 = ORIENTED_EDGE ( 'NONE', *, *, #30823, .T. ) ;
#56111 = CARTESIAN_POINT ( 'NONE',  ( -20.54049170961573267, 0.000000000000000000, 4.660556269540326646 ) ) ;
#56112 = DIRECTION ( 'NONE',  ( 0.000000000000000000, -0.000000000000000000, -1.000000000000000000 ) ) ;
#56113 = CARTESIAN_POINT ( 'NONE',  ( -16.35537091626028428, -0.1191753592594193140, 3.315800596152395308 ) ) ;
#56114 = EDGE_CURVE ( 'NONE', #23328, #7205, #9740, .T. ) ;
#56115 = LINE ( 'NONE', #51830, #55476 ) ;
#56116 = LINE ( 'NONE', #29736, #398 ) ;
#56117 = ADVANCED_FACE ( 'NONE', ( #44925 ), #35552, .F. ) ;
#56118 = LINE ( 'NONE', #16640, #21923 ) ;
#56119 = DIRECTION ( 'NONE',  ( -0.6427681459581293666, -0.7660444431189770143, -0.005002170337467561935 ) ) ;
#56120 = EDGE_LOOP ( 'NONE', ( #43432, #10681, #24534, #12947 ) ) ;
#56121 = DIRECTION ( 'NONE',  ( 0.000000000000000000, -0.000000000000000000, -1.000000000000000000 ) ) ;
#56122 = DIRECTION ( 'NONE',  ( 0.9999697198139515519, 0.000000000000000000, 0.007781995580013368816 ) ) ;
#56123 = ORIENTED_EDGE ( 'NONE', *, *, #24359, .T. ) ;
#56124 = PLANE ( 'NONE',  #12935 ) ;
#56125 = ORIENTED_EDGE ( 'NONE', *, *, #24889, .F. ) ;
#56126 = CARTESIAN_POINT ( 'NONE',  ( -11.61684893682587827, 0.000000000000000000, 4.360670051182396811 ) ) ;
#56127 = ORIENTED_EDGE ( 'NONE', *, *, #1345, .T. ) ;
#56128 = ORIENTED_EDGE ( 'NONE', *, *, #28402, .F. ) ;
#56129 = ORIENTED_EDGE ( 'NONE', *, *, #52288, .F. ) ;
#56130 = ORIENTED_EDGE ( 'NONE', *, *, #55345, .F. ) ;
#56131 = ORIENTED_EDGE ( 'NONE', *, *, #55532, .F. ) ;
#56132 = ORIENTED_EDGE ( 'NONE', *, *, #18901, .F. ) ;
#56133 = CARTESIAN_POINT ( 'NONE',  ( -10.69775370277556092, 0.000000000000000000, 5.675824928454496821 ) ) ;
#56134 = FACE_OUTER_BOUND ( 'NONE', #1022, .T. ) ;
#56135 = CARTESIAN_POINT ( 'NONE',  ( -10.42293219026540996, 0.000000000000000000, 4.369961387370421058 ) ) ;
#56136 = STYLED_ITEM ( 'NONE', ( #53637 ), #29299 ) ;
#56137 = ORIENTED_EDGE ( 'NONE', *, *, #21404, .F. ) ;
#56138 = LINE ( 'NONE', #17508, #24948 ) ;
#56139 = ORIENTED_EDGE ( 'NONE', *, *, #27128, .T. ) ;
#56140 = CARTESIAN_POINT ( 'NONE',  ( -16.51037944162269966, 0.6102101463440037232, 4.295971995366294927 ) ) ;
#56141 = EDGE_LOOP ( 'NONE', ( #6985, #15679, #2498, #20960 ) ) ;
#56142 = EDGE_CURVE ( 'NONE', #41467, #608, #901, .T. ) ;
#56143 = LINE ( 'NONE', #12698, #30314 ) ;
#56144 = ADVANCED_FACE ( 'NONE', ( #52862 ), #26759, .F. ) ;
#56145 = LINE ( 'NONE', #51017, #8322 ) ;
#56146 = DIRECTION ( 'NONE',  ( -0.005961354470445682716, -0.6427876096865404731, 0.7660212471507180654 ) ) ;
#56147 = EDGE_CURVE ( 'NONE', #48933, #17177, #13971, .T. ) ;
#56148 = ORIENTED_EDGE ( 'NONE', *, *, #26345, .F. ) ;
#56149 = PLANE ( 'NONE',  #1973 ) ;
#56150 = ORIENTED_EDGE ( 'NONE', *, *, #4786, .T. ) ;
#56151 = DIRECTION ( 'NONE',  ( 0.000000000000000000, -0.000000000000000000, -1.000000000000000000 ) ) ;
#56152 = ADVANCED_FACE ( 'NONE', ( #3436 ), #15365, .F. ) ;
#56153 = CARTESIAN_POINT ( 'NONE',  ( -23.33693525117809386, 0.000000000000000000, 5.746789908705562944 ) ) ;
#56154 = PLANE ( 'NONE',  #39624 ) ;
#56155 = CARTESIAN_POINT ( 'NONE',  ( -29.86197018149027116, 0.000000000000000000, 8.281335066757780083 ) ) ;
#56156 = PLANE ( 'NONE',  #49215 ) ;
#56157 = LINE ( 'NONE', #42792, #21271 ) ;
#56158 = CARTESIAN_POINT ( 'NONE',  ( -8.473787990993519870, -0.1191753592594177180, 5.593129315755143161 ) ) ;
#56159 = CARTESIAN_POINT ( 'NONE',  ( 2.072287782118878319, 0.000000000000000000, -2.950529333540147015 ) ) ;
#56160 = ORIENTED_EDGE ( 'NONE', *, *, #54835, .F. ) ;
#56161 = LINE ( 'NONE', #12459, #25651 ) ;
#56162 = ORIENTED_EDGE ( 'NONE', *, *, #36194, .F. ) ;
#56163 = APPLICATION_CONTEXT ( 'automotive_design' ) ;
#56164 = DIRECTION ( 'NONE',  ( -0.5449076811759708816, 0.6444004775717707689, 0.5364919789714475140 ) ) ;
#56165 = CARTESIAN_POINT ( 'NONE',  ( -19.60912206198628027, -0.1191753592594197858, 4.398475361799976113 ) ) ;
#56166 = LINE ( 'NONE', #17250, #42613 ) ;
#56167 = LINE ( 'NONE', #16700, #10461 ) ;
#56168 = DIRECTION ( 'NONE',  ( -0.6427681459581293666, -0.7660444431189770143, -0.005002170337467561935 ) ) ;
#56169 = LINE ( 'NONE', #26335, #5085 ) ;
#56170 = CARTESIAN_POINT ( 'NONE',  ( -16.81190032086591302, 0.000000000000000000, 3.212244750653343583 ) ) ;
#56171 = EDGE_LOOP ( 'NONE', ( #33831, #42990, #47195, #10667 ) ) ;
#56172 = PLANE ( 'NONE',  #41144 ) ;
#56173 = CARTESIAN_POINT ( 'NONE',  ( -8.975993561185934055, -0.1191753592594197858, 10.41700724906143982 ) ) ;
#56174 = EDGE_CURVE ( 'NONE', #21327, #32882, #20476, .T. ) ;
#56175 = FACE_OUTER_BOUND ( 'NONE', #26314, .T. ) ;
#56176 = EDGE_CURVE ( 'NONE', #41524, #51537, #33271, .T. ) ;
#56177 = DIRECTION ( 'NONE',  ( 0.007781995580012662783, 0.000000000000000000, -0.9999697198139514409 ) ) ;
#56178 = PLANE ( 'NONE',  #12109 ) ;
#56179 = FACE_OUTER_BOUND ( 'NONE', #48265, .T. ) ;
#56180 = EDGE_CURVE ( 'NONE', #32502, #54118, #16209, .T. ) ;
#56181 = ADVANCED_FACE ( 'NONE', ( #7693 ), #37809, .F. ) ;
#56182 = CARTESIAN_POINT ( 'NONE',  ( -11.63852371047886081, 0.000000000000000000, 7.145831917949534429 ) ) ;
#56183 = ORIENTED_EDGE ( 'NONE', *, *, #39376, .T. ) ;
#56184 = DIRECTION ( 'NONE',  ( -0.9932609354084158682, -0.1139014070068027212, -0.02142857142857160571 ) ) ;
#56185 = LINE ( 'NONE', #39134, #42307 ) ;
#56186 = ORIENTED_EDGE ( 'NONE', *, *, #39169, .F. ) ;
#56187 = EDGE_LOOP ( 'NONE', ( #43018, #12400, #6135, #43970 ) ) ;
#56188 = CARTESIAN_POINT ( 'NONE',  ( -18.88751676427461490, -0.3560938001956550081, 4.602895257318442290 ) ) ;
#56189 = VERTEX_POINT ( 'NONE', #54822 ) ;
#56190 = EDGE_CURVE ( 'NONE', #42734, #9627, #49738, .T. ) ;
#56191 = ORIENTED_EDGE ( 'NONE', *, *, #7425, .F. ) ;
#56192 = ORIENTED_EDGE ( 'NONE', *, *, #36965, .T. ) ;
#56193 = ORIENTED_EDGE ( 'NONE', *, *, #33083, .T. ) ;
#56194 = ORIENTED_EDGE ( 'NONE', *, *, #34815, .F. ) ;
#56195 = LINE ( 'NONE', #228, #35091 ) ;
#56196 = DIRECTION ( 'NONE',  ( -0.5449076811759708816, 0.6444004775717707689, 0.5364919789714475140 ) ) ;
#56197 = VERTEX_POINT ( 'NONE', #33527 ) ;
#56198 = LINE ( 'NONE', #25531, #24873 ) ;
#56199 = ORIENTED_EDGE ( 'NONE', *, *, #16105, .F. ) ;
#56200 = PLANE ( 'NONE',  #20996 ) ;
#56201 = CARTESIAN_POINT ( 'NONE',  ( 5.500940387028407486, 0.000000000000000000, -2.400892578144000034 ) ) ;
#56202 = ORIENTED_EDGE ( 'NONE', *, *, #45937, .F. ) ;
#56203 = LINE ( 'NONE', #34612, #53793 ) ;
#56204 = ORIENTED_EDGE ( 'NONE', *, *, #23773, .T. ) ;
#56205 = DIRECTION ( 'NONE',  ( -0.005002170337468016433, -0.7660444431189770143, 0.6427681459581293666 ) ) ;
#56206 = EDGE_CURVE ( 'NONE', #43321, #37328, #50835, .T. ) ;
#56207 = CARTESIAN_POINT ( 'NONE',  ( -27.06630483948590893, -0.1191753592594197858, 7.295098399573937797 ) ) ;
#56208 = ORIENTED_EDGE ( 'NONE', *, *, #34691, .T. ) ;
#56209 = CARTESIAN_POINT ( 'NONE',  ( -11.13939817157438306, 0.000000000000000000, 2.717731390624371635 ) ) ;
#56210 = CARTESIAN_POINT ( 'NONE',  ( -11.59960461579418300, 0.000000000000000000, 2.144811831635808463 ) ) ;
#56211 = DIRECTION ( 'NONE',  ( -0.005002170337468016433, -0.7660444431189770143, 0.6427681459581293666 ) ) ;
#56212 = FACE_OUTER_BOUND ( 'NONE', #54753, .T. ) ;
#56213 = ORIENTED_EDGE ( 'NONE', *, *, #18140, .T. ) ;
#56214 = ADVANCED_FACE ( 'NONE', ( #32681 ), #41748, .F. ) ;
#56215 = CARTESIAN_POINT ( 'NONE',  ( -10.58976041405849422, 0.7721120973665051013, 2.261911183942312054 ) ) ;
#56216 = LINE ( 'NONE', #52784, #3343 ) ;
#56217 = CARTESIAN_POINT ( 'NONE',  ( -49.27554558092695913, 2.476975532698160620, -5.000000000000000000 ) ) ;
#56218 = LINE ( 'NONE', #30933, #18694 ) ;
#56219 = PLANE ( 'NONE',  #9614 ) ;
#56220 = ADVANCED_FACE ( 'NONE', ( #28991 ), #11931, .F. ) ;
#56221 = CARTESIAN_POINT ( 'NONE',  ( -14.66752777490137483, 3.362543313726509719, 8.097193451663571295 ) ) ;
#56223 = EDGE_CURVE ( 'NONE', #17816, #48176, #29260, .T. ) ;
#56222 = DIRECTION ( 'NONE',  ( 0.007781995580012663651, 0.000000000000000000, -0.9999697198139515519 ) ) ;
#56224 = LINE ( 'NONE', #840, #45624 ) ;
#56225 = DIRECTION ( 'NONE',  ( 0.007781995580012663651, 0.000000000000000000, -0.9999697198139515519 ) ) ;
#56226 = VERTEX_POINT ( 'NONE', #46575 ) ;
#56227 = FILL_AREA_STYLE_COLOUR ( '', #16235 ) ;
#56228 = CARTESIAN_POINT ( 'NONE',  ( -12.33850799832341849, 0.000000000000000000, 11.68350162852954632 ) ) ;
#56229 = ORIENTED_EDGE ( 'NONE', *, *, #6415, .F. ) ;
#56230 = CARTESIAN_POINT ( 'NONE',  ( -22.26155278157260042, 19.71499966066964760, -4.429874095009547652 ) ) ;
#56231 = ADVANCED_FACE ( 'NONE', ( #24183 ), #19902, .F. ) ;
#56232 = DIRECTION ( 'NONE',  ( -0.6427681459581293666, -0.7660444431189770143, -0.005002170337467561935 ) ) ;
#56233 = EDGE_CURVE ( 'NONE', #24571, #19740, #42344, .T. ) ;
#56234 = DIRECTION ( 'NONE',  ( 0.005961354470445682716, -0.6427876096865404731, -0.7660212471507180654 ) ) ;
#56235 = CARTESIAN_POINT ( 'NONE',  ( -19.07977982133608208, 0.000000000000000000, 7.995912495471886317 ) ) ;
#56236 = DIRECTION ( 'NONE',  ( -1.000000000000000000, 0.000000000000000000, 0.000000000000000000 ) ) ;
#56237 = NEXT_ASSEMBLY_USAGE_OCCURRENCE ( 'NAUO1', ' ', ' ', #37453, #25667, $ ) ;
#56238 = NEXT_ASSEMBLY_USAGE_OCCURRENCE ( 'NAUO2', ' ', ' ', #37453, #46837, $ ) ;
#56239 = NEXT_ASSEMBLY_USAGE_OCCURRENCE ( 'NAUO3', ' ', ' ', #37453, #18048, $ ) ;
#56240 = NEXT_ASSEMBLY_USAGE_OCCURRENCE ( 'NAUO4', ' ', ' ', #37453, #27394, $ ) ;
#56241 = NEXT_ASSEMBLY_USAGE_OCCURRENCE ( 'NAUO5', ' ', ' ', #37453, #35061, $ ) ;
ENDSEC;
END-ISO-10303-21;
